#49398 = ORIENTED_EDGE ( 'NONE', *, *, #55295, .F. ) ;
#49399 = CARTESIAN_POINT ( 'NONE',  ( -99.92031302022661521, -296.9800116850897780, -225.4955720367904917 ) ) ;
#49400 = CARTESIAN_POINT ( 'NONE',  ( 15.25994442785172289, -290.2846324905020765, -323.3225548165859777 ) ) ;
#49401 = DIRECTION ( 'NONE',  ( 0.000000000000000000, -1.000000000000000000, 0.000000000000000000 ) ) ;
#49402 = ADVANCED_FACE ( 'NONE', ( #29934 ), #18037, .T. ) ;
#49403 = CARTESIAN_POINT ( 'NONE',  ( 44.71564893372296723, -278.0519495502701375, -270.3284710469131937 ) ) ;
#49404 = ORIENTED_EDGE ( 'NONE', *, *, #29058, .F. ) ;
#49405 = CARTESIAN_POINT ( 'NONE',  ( 26.94804623675772248, -273.0300826965657848, -231.3147130844005233 ) ) ;
#49406 = CARTESIAN_POINT ( 'NONE',  ( 14.91509961193351153, -292.7298278018279802, -325.8198169838761373 ) ) ;
#49407 = CARTESIAN_POINT ( 'NONE',  ( -107.2916408948669869, -272.1835785270253041, -248.9534160687415749 ) ) ;
#49408 = CARTESIAN_POINT ( 'NONE',  ( 33.75592638118311584, -289.3282176880996417, -289.9371406849874120 ) ) ;
#49409 = CARTESIAN_POINT ( 'NONE',  ( 0.9046582555454086849, -282.3296963963192070, -206.9362727628315497 ) ) ;
#49410 = CARTESIAN_POINT ( 'NONE',  ( -82.48977217368603476, -291.0807374593202326, -332.0073496755800306 ) ) ;
#49411 = CARTESIAN_POINT ( 'NONE',  ( -93.22107755772663040, -291.1493789675248536, -322.6944440754704146 ) ) ;
#49412 = CARTESIAN_POINT ( 'NONE',  ( -96.68368674968338894, -285.9235182862970532, -316.2463218228793949 ) ) ;
#49413 = CARTESIAN_POINT ( 'NONE',  ( -28.22710978558685113, -280.3313216066584914, -193.8488492315136682 ) ) ;
#49414 = CARTESIAN_POINT ( 'NONE',  ( -16.92002158697798109, -292.8704321592006750, -343.1632966093561663 ) ) ;
#49415 = CARTESIAN_POINT ( 'NONE',  ( 36.98556796121964396, -281.1330518979061708, -250.1999894972327070 ) ) ;
#49416 = CARTESIAN_POINT ( 'NONE',  ( 36.05947611051713153, -277.2675187611154684, -259.1792451408117586 ) ) ;
#49417 = CARTESIAN_POINT ( 'NONE',  ( 17.40634833298267736, -284.6948066931273047, -313.9805196606274080 ) ) ;
#49418 = CARTESIAN_POINT ( 'NONE',  ( 20.04010931073992552, -274.4743582386694243, -320.1934725044154675 ) ) ;
#49419 = DIRECTION ( 'NONE',  ( 0.000000000000000000, 1.000000000000000000, -0.000000000000000000 ) ) ;
#49420 = CARTESIAN_POINT ( 'NONE',  ( 15.30807541936421678, -280.3283352732976255, -219.6332399031979890 ) ) ;
#49421 = CARTESIAN_POINT ( 'NONE',  ( -39.93406478367798940, -278.2890813930548575, -346.9331684537138472 ) ) ;
#49422 = CARTESIAN_POINT ( 'NONE',  ( -35.39393116032591280, -275.3922497951883201, -196.8811905241217062 ) ) ;
#49423 = CARTESIAN_POINT ( 'NONE',  ( -29.47509650015330251, -285.2082409720796363, -194.0005472665238244 ) ) ;
#49424 = CARTESIAN_POINT ( 'NONE',  ( -111.3820781893685137, -292.3370658619879805, -268.4577588059781874 ) ) ;
#49425 = CARTESIAN_POINT ( 'NONE',  ( -97.19745026043671032, -274.7895696984243727, -223.2046805135603904 ) ) ;
#49426 = ADVANCED_FACE ( 'NONE', ( #53566 ), #17116, .T. ) ;
#49427 = CARTESIAN_POINT ( 'NONE',  ( -66.05776078182081790, -274.9993079865130881, -199.4338074242330947 ) ) ;
#49428 = FACE_OUTER_BOUND ( 'NONE', #50156, .T. ) ;
#49429 = EDGE_CURVE ( 'NONE', #19500, #41151, #31785, .T. ) ;
#49430 = CARTESIAN_POINT ( 'NONE',  ( -112.0438826179248366, -298.6093062999666472, -265.9325340999852187 ) ) ;
#49431 = CARTESIAN_POINT ( 'NONE',  ( -110.7835259300970279, -282.3671488988025544, -284.7251930423820454 ) ) ;
#49432 = CARTESIAN_POINT ( 'NONE',  ( -99.18507155737479764, -290.8286594947131789, -224.5008257068041644 ) ) ;
#49433 = CARTESIAN_POINT ( 'NONE',  ( 26.69966959923290872, -273.0552622143658255, -231.9131996019850703 ) ) ;
#49434 = CARTESIAN_POINT ( 'NONE',  ( -4.657533988044860962, -290.2289052117240544, -339.2099297022812152 ) ) ;
#49435 = CARTESIAN_POINT ( 'NONE',  ( -52.41997561662444127, -290.7749421919414772, -198.5672983850029993 ) ) ;
#49436 = ORIENTED_EDGE ( 'NONE', *, *, #40510, .F. ) ;
#49437 = CARTESIAN_POINT ( 'NONE',  ( -112.5565452629291912, -288.9562423503023183, -283.9011273403303335 ) ) ;
#49438 = CARTESIAN_POINT ( 'NONE',  ( -107.7711572187402140, -290.4735449506566738, -251.0795448945729049 ) ) ;
#49439 = VERTEX_POINT ( 'NONE', #58819 ) ;
#49440 = CARTESIAN_POINT ( 'NONE',  ( 0.1207374816257044542, -287.6184339904154399, -203.4278364882096639 ) ) ;
#49441 = CARTESIAN_POINT ( 'NONE',  ( -105.2859206908969298, -278.5277770804569855, -297.1131343331007315 ) ) ;
#49442 = CARTESIAN_POINT ( 'NONE',  ( -4.646843621756564069, -293.5518285725733563, -339.7479930571689124 ) ) ;
#49443 = CARTESIAN_POINT ( 'NONE',  ( -63.86905923309991806, -284.0405893864820541, -342.5387599876568174 ) ) ;
#49444 = CARTESIAN_POINT ( 'NONE',  ( -109.0103503931437814, -285.2432960619930782, -242.1207800228139035 ) ) ;
#49445 = CARTESIAN_POINT ( 'NONE',  ( 30.35571859035506037, -282.2518552521718789, -297.7316675854043524 ) ) ;
#49446 = CARTESIAN_POINT ( 'NONE',  ( -56.14975209998562633, -169.4529236618342622, -364.5118392738439752 ) ) ;
#49447 = CARTESIAN_POINT ( 'NONE',  ( 63.42894017176210752, 48.18213374631179136, -317.6803299212049865 ) ) ;
#49448 = CARTESIAN_POINT ( 'NONE',  ( -103.1447046786039579, -253.6660498445109226, -324.1576556378894907 ) ) ;
#49449 = CARTESIAN_POINT ( 'NONE',  ( -38.07374021736068670, -273.2399129551845363, -197.2033033293363644 ) ) ;
#49450 = CARTESIAN_POINT ( 'NONE',  ( -13.95386475250040093, -273.2831936092418914, -200.8828103631724105 ) ) ;
#49451 = CARTESIAN_POINT ( 'NONE',  ( -98.22960625220127895, -295.4315019411887420, -317.3950396915814736 ) ) ;
#49452 = CARTESIAN_POINT ( 'NONE',  ( -69.19725544157302011, -196.5455075490810657, -357.0703453118406969 ) ) ;
#49453 = CARTESIAN_POINT ( 'NONE',  ( -103.7928402092161235, -271.7338217202679971, -232.3398782779615601 ) ) ;
#49454 = CARTESIAN_POINT ( 'NONE',  ( -97.10864016964349332, -299.0196190437834503, -226.3080874927117918 ) ) ;
#49455 = CARTESIAN_POINT ( 'NONE',  ( -106.0049828406917101, -291.9747131526716544, -244.5347177229220392 ) ) ;
#49456 = ORIENTED_EDGE ( 'NONE', *, *, #51225, .T. ) ;
#49457 = CARTESIAN_POINT ( 'NONE',  ( -73.18147670076969291, -298.5304458648267314, -202.4177599501777536 ) ) ;
#49458 = CARTESIAN_POINT ( 'NONE',  ( 33.08691790676105171, -287.7878789450689965, -250.9240862264044836 ) ) ;
#49459 = CARTESIAN_POINT ( 'NONE',  ( -11.10271919309420063, -295.5216593545654860, -342.6371999761510665 ) ) ;
#49460 = CARTESIAN_POINT ( 'NONE',  ( -3.250406724806273129, -295.1064021985593513, -339.3489709049057410 ) ) ;
#49461 = CARTESIAN_POINT ( 'NONE',  ( 33.11725889488988628, -293.9716102246571268, -289.5014533879905230 ) ) ;
#49462 = ORIENTED_EDGE ( 'NONE', *, *, #2914, .F. ) ;
#49463 = CARTESIAN_POINT ( 'NONE',  ( 36.80095384282484616, -277.2866570656211707, -255.7946818047045952 ) ) ;
#49464 = EDGE_LOOP ( 'NONE', ( #62519, #29883, #93128 ) ) ;
#49465 = CARTESIAN_POINT ( 'NONE',  ( -71.20185806225903491, -279.1247490881081035, -201.2740959868586117 ) ) ;
#49466 = CARTESIAN_POINT ( 'NONE',  ( -16.58541738105294172, -275.2681287427270718, -200.0758771524112660 ) ) ;
#49467 = CARTESIAN_POINT ( 'NONE',  ( 6.630096824065898176, -276.4006525444441991, -208.3251524675641519 ) ) ;
#49468 = CARTESIAN_POINT ( 'NONE',  ( 24.69806964495408153, -274.1503487569419804, -313.2237394437113949 ) ) ;
#49469 = CARTESIAN_POINT ( 'NONE',  ( -68.09796366834507353, -298.2887424294363541, -204.0304306133187993 ) ) ;
#49470 = CARTESIAN_POINT ( 'NONE',  ( -103.3043138675389514, -294.6868285965343830, -303.1000690853238666 ) ) ;
#49471 = DIRECTION ( 'NONE',  ( 0.000000000000000000, 1.000000000000000000, 0.000000000000000000 ) ) ;
#49472 = CARTESIAN_POINT ( 'NONE',  ( -112.0276974366332894, -279.2764862227519416, -251.8265517239939300 ) ) ;
#49473 = CARTESIAN_POINT ( 'NONE',  ( 33.24273632964369796, -275.9647500860138507, -288.9846873093779891 ) ) ;
#49474 = CARTESIAN_POINT ( 'NONE',  ( 37.80894475152727807, -286.0564668012131051, -256.0196101091842706 ) ) ;
#49475 = CARTESIAN_POINT ( 'NONE',  ( 28.74821194883168118, -300.8778160839800648, -195.1719723918581053 ) ) ;
#49476 = CARTESIAN_POINT ( 'NONE',  ( -83.63170945779077670, -298.0521521680024080, -417.1172536214571096 ) ) ;
#49477 = CARTESIAN_POINT ( 'NONE',  ( 26.51329963375439291, -286.2607146584775819, -234.5483269106472903 ) ) ;
#49478 = CARTESIAN_POINT ( 'NONE',  ( -2.654609909276719915, -278.7572074108526863, -204.9649413578463566 ) ) ;
#49480 = CARTESIAN_POINT ( 'NONE',  ( -92.75298635848811557, -281.9342016311511543, -320.0884899109427693 ) ) ;
#49479 = CARTESIAN_POINT ( 'NONE',  ( -27.46143780333180828, -278.7547148109621844, -197.3865714288429274 ) ) ;
#49481 = CARTESIAN_POINT ( 'NONE',  ( 36.83476319661841814, -289.4056295124209441, -258.9370324115632798 ) ) ;
#49482 = CARTESIAN_POINT ( 'NONE',  ( -74.19947292626356727, -278.7589510638653678, -333.8326477372087879 ) ) ;
#49483 = FACE_OUTER_BOUND ( 'NONE', #69338, .T. ) ;
#49484 = CARTESIAN_POINT ( 'NONE',  ( -101.2569455388316726, -276.2445639505675672, -311.5523723529313429 ) ) ;
#49485 = CARTESIAN_POINT ( 'NONE',  ( 22.35929229859623746, -275.6152737403278934, -228.1531491960829214 ) ) ;
#49486 = CARTESIAN_POINT ( 'NONE',  ( 37.35778549759002942, -283.4392933612969045, -261.5392256303246654 ) ) ;
#49487 = DIRECTION ( 'NONE',  ( -0.000000000000000000, -1.000000000000000000, -0.000000000000000000 ) ) ;
#49488 = CARTESIAN_POINT ( 'NONE',  ( -10.06001275522469740, -290.6188696538366116, -340.8240425048663269 ) ) ;
#49489 = CARTESIAN_POINT ( 'NONE',  ( -28.96227084160118892, -290.1580768956535508, -195.7791394156632521 ) ) ;
#49490 = EDGE_CURVE ( 'NONE', #6854, #1135, #9053, .T. ) ;
#49491 = CARTESIAN_POINT ( 'NONE',  ( 82.15009695330279271, -299.4571376875543365, -197.3638982236675190 ) ) ;
#49492 = CARTESIAN_POINT ( 'NONE',  ( -62.18072331723876545, -272.4070535918263545, -201.1927263230633116 ) ) ;
#49493 = CARTESIAN_POINT ( 'NONE',  ( 36.94389710783553937, -291.6972964711824261, -270.7903160613001319 ) ) ;
#49494 = CARTESIAN_POINT ( 'NONE',  ( -105.6472514815422983, -266.3687386123619376, -319.2208520127341558 ) ) ;
#49495 = LINE ( 'NONE', #77925, #32295 ) ;
#49496 = CARTESIAN_POINT ( 'NONE',  ( -112.4542890685213763, -288.8614080061461777, -283.8814648792027242 ) ) ;
#49497 = CARTESIAN_POINT ( 'NONE',  ( -76.53490712612479285, -285.1857482956578451, -332.9542000552448826 ) ) ;
#49498 = CARTESIAN_POINT ( 'NONE',  ( -65.52470493161366960, -284.8532835358356579, -338.3534474379856078 ) ) ;
#49499 = CARTESIAN_POINT ( 'NONE',  ( -76.20425608541822271, -284.3885809887270852, -332.4073438537532184 ) ) ;
#49500 = CARTESIAN_POINT ( 'NONE',  ( -89.66245974754967563, -293.2991109728522474, -216.0581949996354751 ) ) ;
#49501 = CARTESIAN_POINT ( 'NONE',  ( 37.88615260635930326, -273.5349981528704575, -262.7501664701212007 ) ) ;
#49502 = CARTESIAN_POINT ( 'NONE',  ( 37.92382025403457391, -275.6826096186777590, -254.1480993044922911 ) ) ;
#49503 = CARTESIAN_POINT ( 'NONE',  ( -111.9423063141627352, -288.4790296920276091, -282.3637741688511369 ) ) ;
#49504 = CARTESIAN_POINT ( 'NONE',  ( -39.96295261462560688, -277.0842004637141258, -347.3295545798556532 ) ) ;
#49505 = CARTESIAN_POINT ( 'NONE',  ( -50.74228749793972071, -297.2040775523693128, -343.7932026459827739 ) ) ;
#49506 = CARTESIAN_POINT ( 'NONE',  ( -43.50149443762219903, -252.4652299798295019, -489.6847206897468823 ) ) ;
#49507 = CARTESIAN_POINT ( 'NONE',  ( 180.6899167944524436, 8.542400036368780647, 13.00000000000000178 ) ) ;
#49508 = CARTESIAN_POINT ( 'NONE',  ( -109.2057938497800933, -283.0345584545727888, -285.8091130482690119 ) ) ;
#49509 = CARTESIAN_POINT ( 'NONE',  ( -91.60857109470765636, -277.2794066226040854, -218.5171905846226821 ) ) ;
#49510 = DIRECTION ( 'NONE',  ( 0.000000000000000000, 0.000000000000000000, -1.000000000000000000 ) ) ;
#49511 = CARTESIAN_POINT ( 'NONE',  ( 11.35821897250883339, -273.1926209672289474, -211.5470117345105336 ) ) ;
#49512 = CARTESIAN_POINT ( 'NONE',  ( -13.76035386816042028, -276.0865810103486524, -339.6083501210218856 ) ) ;
#49513 = CARTESIAN_POINT ( 'NONE',  ( 1.955781103605104709, -296.0363515956383367, -332.7626873915692158 ) ) ;
#49514 = CARTESIAN_POINT ( 'NONE',  ( 39.40119774083780868, -280.4672661272284131, -269.9457209600016654 ) ) ;
#49515 = CARTESIAN_POINT ( 'NONE',  ( -26.15969492799074558, -295.8475481464012660, -342.7377109343363486 ) ) ;
#49516 = CARTESIAN_POINT ( 'NONE',  ( -108.9698912448646269, -297.5233737609799505, -297.3935862412163829 ) ) ;
#49517 = CARTESIAN_POINT ( 'NONE',  ( -35.81345161516997422, -297.9051277492375789, -197.3611626661092657 ) ) ;
#49518 = CARTESIAN_POINT ( 'NONE',  ( -78.36997468091350072, -293.5002010129019254, -207.5783071637992521 ) ) ;
#49519 = CARTESIAN_POINT ( 'NONE',  ( -46.50760314449774313, -286.1055498940846178, -193.9086083678337218 ) ) ;
#49520 = CARTESIAN_POINT ( 'NONE',  ( -32.73366931883641229, -272.2492001938284147, -194.7236352448972525 ) ) ;
#49521 = CARTESIAN_POINT ( 'NONE',  ( 2.742822895989173393, -286.4076286265218414, -204.6174413403601022 ) ) ;
#49522 = CARTESIAN_POINT ( 'NONE',  ( -100.8807796076376775, -281.0614440071479407, -231.0880770847348913 ) ) ;
#49523 = CARTESIAN_POINT ( 'NONE',  ( -91.68780161778320803, -284.3124121309485304, -221.1957865600609523 ) ) ;
#49524 = CARTESIAN_POINT ( 'NONE',  ( -34.76180697620001325, -287.0195713852256745, -345.3167368700294446 ) ) ;
#49525 = CARTESIAN_POINT ( 'NONE',  ( -69.18520112214993389, -196.4157418647702968, -356.4528236438462159 ) ) ;
#49526 = CARTESIAN_POINT ( 'NONE',  ( -2.151243864010800699, -286.0386496698555447, -206.2760749116829118 ) ) ;
#49527 = CARTESIAN_POINT ( 'NONE',  ( -113.8789064103646780, -289.5286037834381432, -276.9215164603783137 ) ) ;
#49528 = CARTESIAN_POINT ( 'NONE',  ( -106.8380299810364562, -279.7474731427586789, -301.7416430411084320 ) ) ;
#49529 = EDGE_CURVE ( 'NONE', #35152, #13924, #42222, .T. ) ;
#49530 = CARTESIAN_POINT ( 'NONE',  ( -109.2673725027800202, -279.5340802466330388, -296.5927324422127640 ) ) ;
#49531 = CARTESIAN_POINT ( 'NONE',  ( 21.81069152926886900, -281.9841633384567103, -313.1609556136323249 ) ) ;
#49532 = CARTESIAN_POINT ( 'NONE',  ( 36.59306450925804910, -277.3896077751226130, -257.6893042480007239 ) ) ;
#49533 = CARTESIAN_POINT ( 'NONE',  ( 11.19831191540491311, -294.4013019165051332, -330.2032949994159594 ) ) ;
#49534 = CARTESIAN_POINT ( 'NONE',  ( -64.44102773373909088, -287.4275611035830593, -339.9684785925542769 ) ) ;
#49535 = CARTESIAN_POINT ( 'NONE',  ( -98.69878289298003438, -296.0272434787479483, -230.1502765364316474 ) ) ;
#49536 = ORIENTED_EDGE ( 'NONE', *, *, #28070, .T. ) ;
#49537 = VERTEX_POINT ( 'NONE', #45981 ) ;
#49538 = CARTESIAN_POINT ( 'NONE',  ( -64.55956109852400004, -285.3304219374083459, -339.6467748141643597 ) ) ;
#49539 = CARTESIAN_POINT ( 'NONE',  ( -50.47917533872814744, -294.8912765312112469, -342.1907374426260162 ) ) ;
#49540 = CARTESIAN_POINT ( 'NONE',  ( 37.77063626484817149, -294.8261971509081718, -285.8410867322615445 ) ) ;
#49541 = CARTESIAN_POINT ( 'NONE',  ( -67.81931484460747583, -284.1145029419897696, -336.8066420584136154 ) ) ;
#49542 = CARTESIAN_POINT ( 'NONE',  ( -38.34228576782813036, -273.0986494635421877, -193.6029324753430103 ) ) ;
#49543 = CARTESIAN_POINT ( 'NONE',  ( 5.507411626225722223, -289.1397416561646878, -334.2145940682265746 ) ) ;
#49544 = CARTESIAN_POINT ( 'NONE',  ( -47.12077928171004260, -281.3147074676109582, -345.4921707492155178 ) ) ;
#49545 = CARTESIAN_POINT ( 'NONE',  ( -109.4555248953025028, -291.2278475023503006, -243.2770414514255037 ) ) ;
#49546 = CARTESIAN_POINT ( 'NONE',  ( 27.05111373861568680, -288.3559616659129574, -304.9020584416039696 ) ) ;
#49547 = CARTESIAN_POINT ( 'NONE',  ( 175.2296996224750103, 161.0000000000000853, 0.000000000000000000 ) ) ;
#49548 = DIRECTION ( 'NONE',  ( -0.000000000000000000, -1.000000000000000000, -0.000000000000000000 ) ) ;
#49549 = CARTESIAN_POINT ( 'NONE',  ( 153.3117529583858527, 204.6325910983726999, -214.2920792270980996 ) ) ;
#49550 = CARTESIAN_POINT ( 'NONE',  ( -106.6379572354042296, -282.4809262143061233, -236.9535640164627353 ) ) ;
#49551 = EDGE_LOOP ( 'NONE', ( #33450, #83967, #62867, #85210 ) ) ;
#49552 = CARTESIAN_POINT ( 'NONE',  ( -57.18372481543556773, -278.7103655612335729, -199.7883177753582800 ) ) ;
#49553 = CARTESIAN_POINT ( 'NONE',  ( 38.19881901303173777, -275.0335861821708363, -255.5498297369316276 ) ) ;
#49554 = CARTESIAN_POINT ( 'NONE',  ( -43.32900050412526127, -279.1281170140257473, -344.9545537593516542 ) ) ;
#49555 = CARTESIAN_POINT ( 'NONE',  ( -96.95435030675994881, -248.2403463976193621, -332.6261155525420463 ) ) ;
#49556 = CARTESIAN_POINT ( 'NONE',  ( 21.52843624158481362, -279.4670369831338235, -221.6485596558759994 ) ) ;
#49557 = CARTESIAN_POINT ( 'NONE',  ( -69.74548977179161113, -281.5010251890507789, -337.6198718618985595 ) ) ;
#49558 = CARTESIAN_POINT ( 'NONE',  ( -91.95294407782000690, -297.5787675882438634, -323.1965800079927931 ) ) ;
#49559 = CARTESIAN_POINT ( 'NONE',  ( 8.271472623199930041, -294.9011670952120312, -327.5000151657403080 ) ) ;
#49560 = ORIENTED_EDGE ( 'NONE', *, *, #39491, .T. ) ;
#49561 = CARTESIAN_POINT ( 'NONE',  ( -110.2809895493547998, -289.1189689047381535, -279.3668681743888556 ) ) ;
#49562 = CARTESIAN_POINT ( 'NONE',  ( -2.611013291941904235, -275.1506583338693304, -201.7381837791727435 ) ) ;
#49563 = CARTESIAN_POINT ( 'NONE',  ( -41.87046271344525650, -298.1601761463480216, -197.5017307084477238 ) ) ;
#49564 = ORIENTED_EDGE ( 'NONE', *, *, #43456, .T. ) ;
#49565 = CYLINDRICAL_SURFACE ( 'NONE', #11429, 4.999999999999986677 ) ;
#49566 = CARTESIAN_POINT ( 'NONE',  ( -113.5000000000000568, -296.0521521680024080, -537.7509286889328450 ) ) ;
#49567 = CARTESIAN_POINT ( 'NONE',  ( 202.9738562182569694, 293.9636489450776367, -44.00000000000000000 ) ) ;
#49568 = CARTESIAN_POINT ( 'NONE',  ( -64.94520369595728937, -280.7625471628977607, -202.4474031323467500 ) ) ;
#49569 = CARTESIAN_POINT ( 'NONE',  ( 3.261310291122220928, -282.3494526346327689, -206.0699364363243262 ) ) ;
#49570 = CARTESIAN_POINT ( 'NONE',  ( -73.92469122968472561, -282.6092327882400355, -333.8625342478071047 ) ) ;
#49571 = CARTESIAN_POINT ( 'NONE',  ( 19.77148438193743729, -282.7509526114511118, -222.9183055582599877 ) ) ;
#49572 = CARTESIAN_POINT ( 'NONE',  ( 31.90669141675908804, -274.3664828682270809, -295.7158029609094569 ) ) ;
#49573 = LINE ( 'NONE', #11718, #32169 ) ;
#49574 = CARTESIAN_POINT ( 'NONE',  ( 210.1640492649794396, 37.84931640281016030, 15.00000000000000000 ) ) ;
#49575 = CARTESIAN_POINT ( 'NONE',  ( -14.62765082341001310, -277.5680316141420576, -343.8213981323971780 ) ) ;
#49576 = ORIENTED_EDGE ( 'NONE', *, *, #21333, .F. ) ;
#49577 = VERTEX_POINT ( 'NONE', #44586 ) ;
#49578 = CARTESIAN_POINT ( 'NONE',  ( 175.2296996224750103, 20.99999999999998934, 0.000000000000000000 ) ) ;
#49579 = CARTESIAN_POINT ( 'NONE',  ( -35.90472487002985957, -285.0141347437764239, -345.7154563273417693 ) ) ;
#49580 = CARTESIAN_POINT ( 'NONE',  ( -1.167960896321708075, -291.7424252701682690, -206.7536673425425420 ) ) ;
#49581 = CARTESIAN_POINT ( 'NONE',  ( 0.6616879887054784026, -287.9082371396405620, -337.2722809867586875 ) ) ;
#49582 = CARTESIAN_POINT ( 'NONE',  ( -84.27335583830985399, -283.6365492073206269, -213.0634882587885102 ) ) ;
#49584 = CARTESIAN_POINT ( 'NONE',  ( -98.19466404581379493, -288.2128417990739422, -312.5128459672343411 ) ) ;
#49583 = CARTESIAN_POINT ( 'NONE',  ( -60.14411520869510497, -284.3254146904577624, -200.3938057380328814 ) ) ;
#49585 = CARTESIAN_POINT ( 'NONE',  ( -42.94801503898276707, -284.3294240698869544, -343.5941236076088217 ) ) ;
#49586 = CARTESIAN_POINT ( 'NONE',  ( 34.67285453171767529, -273.2801550712969743, -249.2293634457164728 ) ) ;
#49587 = CARTESIAN_POINT ( 'NONE',  ( -113.5554106382944468, -282.9211639783850387, -272.8030521181833592 ) ) ;
#49588 = CARTESIAN_POINT ( 'NONE',  ( -82.94830302127458310, -297.6758264042525752, -329.9668054032773057 ) ) ;
#49589 = CARTESIAN_POINT ( 'NONE',  ( -13.26622357517111617, -284.3639863414972524, -199.1543777550592722 ) ) ;
#49590 = CARTESIAN_POINT ( 'NONE',  ( -108.2032837142395749, -279.7373841354975639, -251.8173843365363211 ) ) ;
#49591 = CARTESIAN_POINT ( 'NONE',  ( 17.00785990269967840, -288.8241946479862463, -218.3615801760174122 ) ) ;
#49592 = CARTESIAN_POINT ( 'NONE',  ( 195.4781563537916043, 27.48493576247232895, 13.99999999999999822 ) ) ;
#49593 = CARTESIAN_POINT ( 'NONE',  ( 143.6449502718966755, -26.00396092263537540, 10.00000000000000178 ) ) ;
#49594 = CARTESIAN_POINT ( 'NONE',  ( 25.33126874728590039, -296.0389554458250245, -312.5679085555575512 ) ) ;
#49595 = CARTESIAN_POINT ( 'NONE',  ( -109.9012063239138683, -276.7964472443777026, -251.3339455880679338 ) ) ;
#49596 = CARTESIAN_POINT ( 'NONE',  ( -95.53192449113932128, -290.4285580735957524, -220.1607689647812833 ) ) ;
#49597 = CARTESIAN_POINT ( 'NONE',  ( 25.09330174392906798, -292.4908341288756901, -309.8056540410530033 ) ) ;
#49598 = CARTESIAN_POINT ( 'NONE',  ( -35.63466596294345123, -278.7588033778637282, -196.8753064768455658 ) ) ;
#49599 = CARTESIAN_POINT ( 'NONE',  ( -78.17190898149146960, -295.6367116617522584, -208.3012988245606891 ) ) ;
#49600 = CARTESIAN_POINT ( 'NONE',  ( -79.82936358749519457, -292.7796340671091571, -210.3317237195485916 ) ) ;
#49601 = CARTESIAN_POINT ( 'NONE',  ( -69.91165696735023971, -282.1233781216988064, -202.8022627189028810 ) ) ;
#49602 = CARTESIAN_POINT ( 'NONE',  ( -104.0066924283642322, -294.5451093671936746, -307.5971586733796812 ) ) ;
#49603 = CARTESIAN_POINT ( 'NONE',  ( -58.90361246526235561, -290.9357826069282282, -340.9944099585647450 ) ) ;
#49604 = CARTESIAN_POINT ( 'NONE',  ( 19.63394104791870731, -291.1019812454345583, -220.0647154533644994 ) ) ;
#49605 = CARTESIAN_POINT ( 'NONE',  ( -75.29896657940909677, -292.9610962875026985, -207.2570240953997143 ) ) ;
#49606 = CARTESIAN_POINT ( 'NONE',  ( 208.4306832106270804, -142.7221692137691775, 0.000000000000000000 ) ) ;
#49607 = CARTESIAN_POINT ( 'NONE',  ( -110.4671951191295989, -291.3080536491619910, -273.9269992693220388 ) ) ;
#49608 = LINE ( 'NONE', #64792, #14290 ) ;
#49609 = CIRCLE ( 'NONE', #63234, 25.00000000000000355 ) ;
#49610 = CARTESIAN_POINT ( 'NONE',  ( -99.71669408052348160, -292.3492262705923963, -225.8935022547664460 ) ) ;
#49612 = CARTESIAN_POINT ( 'NONE',  ( 34.06757603069395657, -293.7528807033340854, -285.5774379089120885 ) ) ;
#49611 = CARTESIAN_POINT ( 'NONE',  ( 34.89456460024948115, -279.8493962182371888, -291.9956943013424961 ) ) ;
#49613 = CARTESIAN_POINT ( 'NONE',  ( 33.17294455255802887, -281.1576968875261855, -239.4307949069247172 ) ) ;
#49614 = CARTESIAN_POINT ( 'NONE',  ( 39.50776930507541351, -281.2852057226770057, -275.6636721458789907 ) ) ;
#49615 = CARTESIAN_POINT ( 'NONE',  ( 8.159987322417903144, -284.6737996474529950, -210.6750414418727928 ) ) ;
#49616 = CARTESIAN_POINT ( 'NONE',  ( 35.14141974038829375, -279.8997213074912338, -286.3942966432434787 ) ) ;
#49617 = CARTESIAN_POINT ( 'NONE',  ( -59.88388321257586000, -283.7600525532362212, -198.7748273930347693 ) ) ;
#49618 = DIRECTION ( 'NONE',  ( 0.000000000000000000, -0.000000000000000000, 1.000000000000000000 ) ) ;
#49619 = CARTESIAN_POINT ( 'NONE',  ( -35.33468722438668408, -278.5567669666513666, -194.0678292584169640 ) ) ;
#49620 = CARTESIAN_POINT ( 'NONE',  ( -64.42511264268087245, -284.6271620021917101, -198.5975743485952023 ) ) ;
#49621 = CARTESIAN_POINT ( 'NONE',  ( -31.33662544711657461, -274.9327347012768428, -197.4338273301233073 ) ) ;
#49622 = FACE_OUTER_BOUND ( 'NONE', #76816, .T. ) ;
#49623 = CARTESIAN_POINT ( 'NONE',  ( 17.31711840160693328, -294.4487299873505322, -220.6993588358198508 ) ) ;
#49624 = CARTESIAN_POINT ( 'NONE',  ( 39.04135970047725124, -276.9514893513464813, -268.3033370053312865 ) ) ;
#49625 = CARTESIAN_POINT ( 'NONE',  ( -100.6032727243791811, -277.7177423027198984, -306.9326810004016011 ) ) ;
#49626 = CARTESIAN_POINT ( 'NONE',  ( -113.1329248472795399, -290.5479374808705302, -284.0256608303066059 ) ) ;
#49627 = CARTESIAN_POINT ( 'NONE',  ( -1.790921918066832985, -278.5992873217503529, -203.6868623150331246 ) ) ;
#49628 = CARTESIAN_POINT ( 'NONE',  ( -27.84698658338809096, -292.0027258700518473, -193.8950725848873162 ) ) ;
#49629 = EDGE_CURVE ( 'NONE', #31036, #14296, #64991, .T. ) ;
#49630 = CARTESIAN_POINT ( 'NONE',  ( -98.48941110709382940, -290.1691730303283521, -229.9656015824488406 ) ) ;
#49631 = CARTESIAN_POINT ( 'NONE',  ( -1.680188893756997093, -292.5794578047132291, -336.3548329139419479 ) ) ;
#49632 = ORIENTED_EDGE ( 'NONE', *, *, #79909, .F. ) ;
#49633 = CARTESIAN_POINT ( 'NONE',  ( 151.7498149058253887, 20.88232504567505288, 8.615841630451626543 ) ) ;
#49634 = CARTESIAN_POINT ( 'NONE',  ( 6.718338184219007303, -292.1777447237187175, -212.0798905985906515 ) ) ;
#49635 = CARTESIAN_POINT ( 'NONE',  ( 209.2890703971520452, 28.92173720827219086, 12.90116063919741407 ) ) ;
#49636 = CARTESIAN_POINT ( 'NONE',  ( -105.5937364680635966, -275.8380690714489560, -285.9065529553535612 ) ) ;
#49637 = CARTESIAN_POINT ( 'NONE',  ( -100.5500932208516929, -296.1880342579137846, -226.7774985727764658 ) ) ;
#49638 = CARTESIAN_POINT ( 'NONE',  ( -83.57180211223099775, -284.9862033013532709, -331.3872817576119019 ) ) ;
#49639 = CARTESIAN_POINT ( 'NONE',  ( 34.99643936965391333, -287.2512179996217014, -260.1839862995061594 ) ) ;
#49640 = CARTESIAN_POINT ( 'NONE',  ( 33.52141173430761967, -276.8052013668915379, -249.9520608366478598 ) ) ;
#49641 = CARTESIAN_POINT ( 'NONE',  ( -95.23384881368116339, -293.9198106378700572, -317.5017610726400221 ) ) ;
#49642 = CARTESIAN_POINT ( 'NONE',  ( -107.6766929757261266, -298.6158341756103027, -247.1558544014971233 ) ) ;
#49643 = CARTESIAN_POINT ( 'NONE',  ( -7.359414719053728682, -275.4448656147606016, -337.3550958277109544 ) ) ;
#49644 = EDGE_LOOP ( 'NONE', ( #30553, #25102, #21478, #10938 ) ) ;
#49645 = CARTESIAN_POINT ( 'NONE',  ( 195.0629117428269126, 293.9636489450776367, -54.00000000000000000 ) ) ;
#49646 = CARTESIAN_POINT ( 'NONE',  ( -114.2883800339493945, -296.2642707458900873, -266.7320425566662152 ) ) ;
#49647 = CARTESIAN_POINT ( 'NONE',  ( 32.31355466127269693, -289.1269743330070128, -243.9581742184847997 ) ) ;
#49648 = CARTESIAN_POINT ( 'NONE',  ( -71.68231431399064491, -295.5982969377303107, -203.6706444086711656 ) ) ;
#49649 = EDGE_CURVE ( 'NONE', #69300, #85724, #89055, .T. ) ;
#49650 = CARTESIAN_POINT ( 'NONE',  ( 24.32878666437833104, -288.7455111955325719, -309.6121527064545376 ) ) ;
#49651 = EDGE_LOOP ( 'NONE', ( #54403, #12775 ) ) ;
#49652 = CARTESIAN_POINT ( 'NONE',  ( -94.77775522932822128, -278.3030756798927996, -219.4305791311844871 ) ) ;
#49653 = CARTESIAN_POINT ( 'NONE',  ( 21.29530990945289659, -294.8750403548178838, -320.1106289427427782 ) ) ;
#49654 = CARTESIAN_POINT ( 'NONE',  ( -97.19856780072755953, -288.0613605313578773, -316.8095934867362757 ) ) ;
#49655 = CARTESIAN_POINT ( 'NONE',  ( -66.91239187261079735, -295.7624826590495672, -341.4479435667584539 ) ) ;
#49656 = CARTESIAN_POINT ( 'NONE',  ( 35.72916729967085558, -293.8906406244881282, -270.7558028428315424 ) ) ;
#49657 = DIRECTION ( 'NONE',  ( -0.000000000000000000, -0.000000000000000000, 1.000000000000000000 ) ) ;
#49658 = PRESENTATION_STYLE_ASSIGNMENT (( #78091 ) ) ;
#49659 = CARTESIAN_POINT ( 'NONE',  ( 139.4823848151520735, 130.0000000000000568, 12.50000000000000000 ) ) ;
#49660 = CARTESIAN_POINT ( 'NONE',  ( -48.74608349352957504, -290.7148443258338943, -345.8642122658699236 ) ) ;
#49661 = CARTESIAN_POINT ( 'NONE',  ( -115.3288506153726871, -280.8376638359844151, -288.1938231032136741 ) ) ;
#49662 = CARTESIAN_POINT ( 'NONE',  ( -84.49787322702056258, -278.7709811839317240, -209.5515938806253189 ) ) ;
#49663 = CARTESIAN_POINT ( 'NONE',  ( -104.6508006407196802, -286.1190163151418915, -303.1834571744745972 ) ) ;
#49664 = CARTESIAN_POINT ( 'NONE',  ( 22.54152070417518772, -285.4866857326896366, -222.8786281705411625 ) ) ;
#49665 = CARTESIAN_POINT ( 'NONE',  ( 35.93496382104577691, -285.8015801664035394, -283.4700737045235428 ) ) ;
#49666 = CARTESIAN_POINT ( 'NONE',  ( 18.97519612362179586, -278.1118691077887206, -321.0630098132747889 ) ) ;
#49668 = CARTESIAN_POINT ( 'NONE',  ( 29.06875212512782625, -280.4876672165820537, -239.6858164139459575 ) ) ;
#49667 = CARTESIAN_POINT ( 'NONE',  ( -93.94052838712022435, -279.2047528621832839, -224.2571849648247735 ) ) ;
#49669 = CARTESIAN_POINT ( 'NONE',  ( 1.028806970584595248, -275.6313910885928635, -203.9441133298500688 ) ) ;
#49670 = CARTESIAN_POINT ( 'NONE',  ( -101.5499708662807166, -277.8996932533872268, -228.4882948711697850 ) ) ;
#49671 = CARTESIAN_POINT ( 'NONE',  ( -40.74239786503150640, -139.1097897353693043, -361.8818269458895998 ) ) ;
#49672 = CARTESIAN_POINT ( 'NONE',  ( -29.87373460061922970, -275.0857525414263591, -193.9605309191074412 ) ) ;
#49673 = CARTESIAN_POINT ( 'NONE',  ( -106.2257198045210771, -274.4969280293119596, -237.5327829029802444 ) ) ;
#49674 = CARTESIAN_POINT ( 'NONE',  ( -114.2704648735229114, -287.0519495502703080, -270.3937649182068981 ) ) ;
#49675 = EDGE_LOOP ( 'NONE', ( #35595, #32058, #46453, #9948, #11003 ) ) ;
#49676 = VECTOR ( 'NONE', #31258, 1000.000000000000000 ) ;
#49677 = CARTESIAN_POINT ( 'NONE',  ( 82.62056641594917039, -301.7796436375890039, -194.2090517697148186 ) ) ;
#49678 = CARTESIAN_POINT ( 'NONE',  ( -2.049596653466665863, -287.6104143716297585, -206.0492558786767461 ) ) ;
#49679 = CARTESIAN_POINT ( 'NONE',  ( -52.00005431648487075, -287.6273099305882965, -195.7480235018652195 ) ) ;
#49680 = CARTESIAN_POINT ( 'NONE',  ( -18.45515703022170939, -288.1510543174051122, -341.0338234723051301 ) ) ;
#49681 = CARTESIAN_POINT ( 'NONE',  ( -88.28548820939360553, -283.2506877295736558, -328.0886325323236292 ) ) ;
#49682 = CARTESIAN_POINT ( 'NONE',  ( 25.83152688473413505, -279.4314095742582822, -232.1099269025458796 ) ) ;
#49683 = CARTESIAN_POINT ( 'NONE',  ( -41.41398145405877074, -287.8607831278534945, -196.2249841810826751 ) ) ;
#49684 = CARTESIAN_POINT ( 'NONE',  ( 33.40558350444596414, -279.7617100432004236, -249.7327488801840900 ) ) ;
#49685 = CARTESIAN_POINT ( 'NONE',  ( -6.051555397364877464, -277.9472573267697157, -336.8743821977475363 ) ) ;
#49686 = CARTESIAN_POINT ( 'NONE',  ( -11.47429486009469279, -274.8906215937448110, -201.9779292118369369 ) ) ;
#49687 = CARTESIAN_POINT ( 'NONE',  ( 36.00076146474930994, -286.6265590629299709, -292.5175486488519709 ) ) ;
#49688 = CARTESIAN_POINT ( 'NONE',  ( 23.28183560395387985, -282.9872311641152578, -317.5940955169109543 ) ) ;
#49689 = CARTESIAN_POINT ( 'NONE',  ( -104.3603271607003080, -284.5525202608938571, -308.2583003458410076 ) ) ;
#49690 = CARTESIAN_POINT ( 'NONE',  ( 35.35213792486316464, -281.6236964745351088, -263.1492342920464012 ) ) ;
#49691 = EDGE_LOOP ( 'NONE', ( #28744, #2059, #28949, #17902 ) ) ;
#49692 = ORIENTED_EDGE ( 'NONE', *, *, #42029, .T. ) ;
#49693 = CARTESIAN_POINT ( 'NONE',  ( 208.3936076804783966, 28.69480487596609919, 12.02381566707519944 ) ) ;
#49694 = CARTESIAN_POINT ( 'NONE',  ( -68.82211440461092877, -291.3219884770352337, -339.2903931898455880 ) ) ;
#49695 = CARTESIAN_POINT ( 'NONE',  ( -100.9160869950618746, -272.1086698645432875, -233.9038964900763915 ) ) ;
#49696 = CARTESIAN_POINT ( 'NONE',  ( 30.80817011324824861, -293.3609315278985719, -305.9828525328463797 ) ) ;
#49697 = CARTESIAN_POINT ( 'NONE',  ( -110.1067658829752673, -288.8786206709077646, -282.1005037632070298 ) ) ;
#49698 = CARTESIAN_POINT ( 'NONE',  ( 22.63890038393446602, -291.1934726271103386, -226.9771136712184330 ) ) ;
#49699 = CARTESIAN_POINT ( 'NONE',  ( 28.59114552718344981, -289.1916847768924868, -302.6099996284083886 ) ) ;
#49700 = CARTESIAN_POINT ( 'NONE',  ( -114.2704648735229114, -293.0519495502703080, -270.3937649182068981 ) ) ;
#49701 = CARTESIAN_POINT ( 'NONE',  ( -103.3825209483136689, -292.0804366682577893, -305.9084193053351441 ) ) ;
#49702 = CARTESIAN_POINT ( 'NONE',  ( -111.0747440640663655, -288.3639759312362116, -285.0369665777968748 ) ) ;
#49703 = CARTESIAN_POINT ( 'NONE',  ( -83.50245649666280201, -293.4198109312240490, -211.1843974535695168 ) ) ;
#49704 = CARTESIAN_POINT ( 'NONE',  ( -9.414723203474760993, -287.3675725798953522, -202.6460727989379507 ) ) ;
#49705 = CARTESIAN_POINT ( 'NONE',  ( 34.93415448850418414, -295.2866542660498226, -249.6689545277754121 ) ) ;
#49706 = CARTESIAN_POINT ( 'NONE',  ( -114.3276611901150659, -272.2616898454610350, -270.3574197013679168 ) ) ;
#49707 = DIRECTION ( 'NONE',  ( 0.000000000000000000, 1.000000000000000000, 0.000000000000000000 ) ) ;
#49708 = CARTESIAN_POINT ( 'NONE',  ( -111.9202768220849578, -274.6745027186147468, -259.2135409318198640 ) ) ;
#49709 = PRODUCT_DEFINITION_SHAPE ( 'NONE', 'NONE',  #12282 ) ;
#49710 = CARTESIAN_POINT ( 'NONE',  ( -3.959231174534847408, -280.6116839024791716, -337.5222035863770884 ) ) ;
#49711 = CARTESIAN_POINT ( 'NONE',  ( -113.4404092577192102, -295.8838235641732695, -259.6290520699915305 ) ) ;
#49712 = CARTESIAN_POINT ( 'NONE',  ( 20.66346370439013214, -273.1518255304276863, -224.3693719893715581 ) ) ;
#49713 = CARTESIAN_POINT ( 'NONE',  ( -51.57979615484179448, -275.3155206882368589, -343.4267789771403727 ) ) ;
#49714 = CARTESIAN_POINT ( 'NONE',  ( -101.6541489594178671, -298.3501832310023474, -234.7921370840643362 ) ) ;
#49715 = CARTESIAN_POINT ( 'NONE',  ( 17.67802907595304518, -273.3946276828778537, -217.2621713217016293 ) ) ;
#49716 = CARTESIAN_POINT ( 'NONE',  ( -109.7183769884873783, -297.8024216431435320, -283.7346490028505741 ) ) ;
#49717 = CARTESIAN_POINT ( 'NONE',  ( 196.0143093133015384, 24.42324672360809856, 11.99999999999998934 ) ) ;
#49718 = CARTESIAN_POINT ( 'NONE',  ( -101.6042868250468132, -296.8787084771199147, -305.3314150575736221 ) ) ;
#49719 = DIRECTION ( 'NONE',  ( 2.312964634635742267E-15, 0.000000000000000000, 1.000000000000000000 ) ) ;
#49721 = CARTESIAN_POINT ( 'NONE',  ( -65.57271514531647938, -297.6724027894083520, -203.0409145433498566 ) ) ;
#49720 = CARTESIAN_POINT ( 'NONE',  ( 37.70702564139116220, -285.6590223072589083, -277.1504891859455597 ) ) ;
#49722 = CARTESIAN_POINT ( 'NONE',  ( -68.50075781982525314, -285.6539466809196597, -199.9328714335240136 ) ) ;
#49723 = CARTESIAN_POINT ( 'NONE',  ( 37.12288259716916627, -287.4631987071650769, -289.8744521711566904 ) ) ;
#49724 = CARTESIAN_POINT ( 'NONE',  ( -111.2798307700559377, -298.7187674465575924, -255.7495586203262690 ) ) ;
#49725 = CARTESIAN_POINT ( 'NONE',  ( 24.43233675399941163, -292.1264055033022942, -312.6890782453603492 ) ) ;
#49726 = CARTESIAN_POINT ( 'NONE',  ( -98.44172566682247805, -278.3720035304528437, -223.7462797582116139 ) ) ;
#49727 = CARTESIAN_POINT ( 'NONE',  ( -95.99890600148557951, -287.4094976428776249, -317.0979686699210447 ) ) ;
#49728 = CARTESIAN_POINT ( 'NONE',  ( -23.40286736638519471, -135.2391364535880598, 22.50000000000000000 ) ) ;
#49729 = CARTESIAN_POINT ( 'NONE',  ( 16.27496074099764201, -285.6297388381625524, -220.2188778058160779 ) ) ;
#49730 = CARTESIAN_POINT ( 'NONE',  ( 197.3748232817348764, 214.9910457053126720, -12.45182892472558756 ) ) ;
#49731 = CARTESIAN_POINT ( 'NONE',  ( -81.60792948368583666, -287.6540168532412736, -330.9691453748866365 ) ) ;
#49732 = CARTESIAN_POINT ( 'NONE',  ( -72.05916672277926693, -299.1851909532456943, -205.2227431646824982 ) ) ;
#49733 = CARTESIAN_POINT ( 'NONE',  ( -11.72412971190821906, -281.8044268473148009, -198.3170543768111145 ) ) ;
#49735 = CARTESIAN_POINT ( 'NONE',  ( 3.390220919244847142, -282.4879635587228108, -331.0020504551936824 ) ) ;
#49734 = CARTESIAN_POINT ( 'NONE',  ( -111.0027954374962889, -294.3692174197221902, -286.2497883133154346 ) ) ;
#49736 = CARTESIAN_POINT ( 'NONE',  ( -113.6020565022060964, -296.8531797794875047, -259.6187472219308461 ) ) ;
#49737 = CARTESIAN_POINT ( 'NONE',  ( -110.9309288753746898, -273.9771951043131253, -270.3792229722685647 ) ) ;
#49738 = CARTESIAN_POINT ( 'NONE',  ( -4.555522512807772983, -282.4842437307777345, -202.8927937204268517 ) ) ;
#49739 = EDGE_CURVE ( 'NONE', #62133, #37419, #36222, .T. ) ;
#49741 = CARTESIAN_POINT ( 'NONE',  ( -97.06770705644282771, -296.2008161783655851, -227.9793702028909763 ) ) ;
#49740 = AXIS2_PLACEMENT_3D ( 'NONE', #24322, #67438, #1620 ) ;
#49742 = VERTEX_POINT ( 'NONE', #88128 ) ;
#49743 = DIRECTION ( 'NONE',  ( -1.000000000000000000, 0.000000000000000000, -0.000000000000000000 ) ) ;
#49744 = CARTESIAN_POINT ( 'NONE',  ( -18.29207605295991712, -284.7855113607416797, -342.5878238165592506 ) ) ;
#49745 = DIRECTION ( 'NONE',  ( 0.000000000000000000, 0.000000000000000000, 1.000000000000000000 ) ) ;
#49746 = CARTESIAN_POINT ( 'NONE',  ( 31.98288692825983404, -284.6237833571634042, -237.0123917617631264 ) ) ;
#49747 = CARTESIAN_POINT ( 'NONE',  ( 38.06226357854495035, -274.5641106988937850, -255.5827189383154803 ) ) ;
#49748 = CARTESIAN_POINT ( 'NONE',  ( -4.831172163236261419, -292.3259308427347491, -204.9861529717488509 ) ) ;
#49749 = CARTESIAN_POINT ( 'NONE',  ( 32.62886164679441237, -282.7662583247020507, -247.0740623273265442 ) ) ;
#49750 = CARTESIAN_POINT ( 'NONE',  ( 16.19206890419980382, -277.8765737109999918, -321.1604879431225754 ) ) ;
#49751 = CARTESIAN_POINT ( 'NONE',  ( -52.78067841596896415, -284.6713877280255360, -345.2499698865493087 ) ) ;
#49752 = CARTESIAN_POINT ( 'NONE',  ( 32.35849621574372037, -280.0415000291916954, -247.2005414872594997 ) ) ;
#49753 = CARTESIAN_POINT ( 'NONE',  ( -95.13123691389665737, -279.8924247039564079, -318.1867755589982494 ) ) ;
#49754 = CARTESIAN_POINT ( 'NONE',  ( 76.38675318495047861, -299.4392170424915776, -193.3610342431294384 ) ) ;
#49755 = CARTESIAN_POINT ( 'NONE',  ( 37.23821526959913086, -275.6251632670080767, -289.5140870422535500 ) ) ;
#49756 = CARTESIAN_POINT ( 'NONE',  ( 21.30251398466877077, -294.8382676646551204, -224.4910585793413418 ) ) ;
#49757 = CARTESIAN_POINT ( 'NONE',  ( 128.9467878515196162, -299.5541904835127980, -195.3611179825600175 ) ) ;
#49758 = ADVANCED_FACE ( 'NONE', ( #30866, #67775, #9527 ), #8147, .F. ) ;
#49759 = EDGE_CURVE ( 'NONE', #41101, #86528, #77050, .T. ) ;
#49760 = FACE_OUTER_BOUND ( 'NONE', #63339, .T. ) ;
#49761 = CARTESIAN_POINT ( 'NONE',  ( -113.0739147689394173, -294.7373817827403286, -266.7698167784902807 ) ) ;
#49762 = CARTESIAN_POINT ( 'NONE',  ( -43.48104944718411247, -273.4803023304604039, -197.5072270856211105 ) ) ;
#49763 = CARTESIAN_POINT ( 'NONE',  ( 38.96195801657260205, -295.0354543878029858, -267.4436248985124962 ) ) ;
#49764 = CARTESIAN_POINT ( 'NONE',  ( 37.96971742631737357, -294.9342013471664359, -284.4391780805657959 ) ) ;
#49765 = CARTESIAN_POINT ( 'NONE',  ( 35.80805840993487266, -289.7561556815304584, -286.2055236481873521 ) ) ;
#49766 = CARTESIAN_POINT ( 'NONE',  ( -108.1719323841925871, -276.8668976351476658, -246.0545505532937796 ) ) ;
#49767 = CARTESIAN_POINT ( 'NONE',  ( -29.53863327607716371, -278.8728663359054281, -344.4429308395170892 ) ) ;
#49768 = CARTESIAN_POINT ( 'NONE',  ( -38.38655828616665389, -293.1451975357958872, -344.7937887181799965 ) ) ;
#49769 = CARTESIAN_POINT ( 'NONE',  ( 38.05151388181356253, -283.5142879931343600, -278.3641237027651982 ) ) ;
#49770 = CARTESIAN_POINT ( 'NONE',  ( -89.87480949249908235, -284.2094730787247272, -219.1561191593192461 ) ) ;
#49771 = CARTESIAN_POINT ( 'NONE',  ( 204.9738562182569979, 293.9636489450776367, -54.00000000001201528 ) ) ;
#49772 = ORIENTED_EDGE ( 'NONE', *, *, #68258, .T. ) ;
#49773 = CARTESIAN_POINT ( 'NONE',  ( -87.70601829063315336, -284.9914670230021443, -217.4884129000527651 ) ) ;
#49774 = CARTESIAN_POINT ( 'NONE',  ( 24.01609537645098769, -283.2465998793716153, -316.3688721279685865 ) ) ;
#49775 = CARTESIAN_POINT ( 'NONE',  ( -107.8676054081266500, -282.9629749341521006, -300.3984759287489510 ) ) ;
#49776 = CARTESIAN_POINT ( 'NONE',  ( -96.64334107210639502, -280.1503675080806488, -221.5950525213766866 ) ) ;
#49777 = CARTESIAN_POINT ( 'NONE',  ( -77.43399729802185050, -279.0993625569138317, -335.3479731977087681 ) ) ;
#49778 = CARTESIAN_POINT ( 'NONE',  ( 7.450504543161046378, -296.9090924074130839, -326.4764044574609443 ) ) ;
#49779 = CARTESIAN_POINT ( 'NONE',  ( -55.29403410364363225, -169.9286504849079904, -364.5147574933134251 ) ) ;
#49780 = ORIENTED_EDGE ( 'NONE', *, *, #66104, .F. ) ;
#49781 = CARTESIAN_POINT ( 'NONE',  ( -106.0734115640449318, -274.9418047119115727, -240.6327310223400957 ) ) ;
#49782 = CARTESIAN_POINT ( 'NONE',  ( -46.63682837063362996, -277.9538278851993027, -196.2450598393899668 ) ) ;
#49783 = CARTESIAN_POINT ( 'NONE',  ( -74.20715666390071874, -293.3291786543345552, -203.9163128504025053 ) ) ;
#49784 = CARTESIAN_POINT ( 'NONE',  ( 19.43019322377892166, -292.2498925517618318, -224.2886864290337030 ) ) ;
#49785 = CARTESIAN_POINT ( 'NONE',  ( -68.03509219607683178, -288.9521356912331385, -340.9121107944810660 ) ) ;
#49786 = CARTESIAN_POINT ( 'NONE',  ( 200.4644824113734387, 249.5000000000000568, -2.942835885954282471 ) ) ;
#49788 = CARTESIAN_POINT ( 'NONE',  ( -73.93479024045835502, -283.9573723216579424, -206.2575723485693686 ) ) ;
#49787 = CARTESIAN_POINT ( 'NONE',  ( -41.92847484860295282, -293.6834815892525512, -346.6860920940337110 ) ) ;
#49789 = CARTESIAN_POINT ( 'NONE',  ( -90.72068405743362973, -293.1456056904294769, -218.7709100491314302 ) ) ;
#49790 = CARTESIAN_POINT ( 'NONE',  ( -23.95937649564948302, -284.1927967358367937, -342.6256105837574637 ) ) ;
#49791 = VERTEX_POINT ( 'NONE', #24204 ) ;
#49792 = CARTESIAN_POINT ( 'NONE',  ( -72.07655293769614957, -292.5454155814339856, -201.8899322832148471 ) ) ;
#49793 = CARTESIAN_POINT ( 'NONE',  ( -7.980464836452424215, -280.9398203629957607, -203.4452201630073773 ) ) ;
#49794 = CARTESIAN_POINT ( 'NONE',  ( 8.655424666131757760, -293.2322592690497913, -331.6169195703292871 ) ) ;
#49795 = CARTESIAN_POINT ( 'NONE',  ( -48.83472583511090903, -289.9976704382382877, -346.3890832113571605 ) ) ;
#49796 = CARTESIAN_POINT ( 'NONE',  ( -38.91262770159233497, -289.5637108024761233, -347.2835405265697659 ) ) ;
#49797 = CARTESIAN_POINT ( 'NONE',  ( 16.88919303119128301, -287.0189286124443129, -221.4751854650539826 ) ) ;
#49798 = ORIENTED_EDGE ( 'NONE', *, *, #82272, .F. ) ;
#49799 = CARTESIAN_POINT ( 'NONE',  ( 195.6201958373143270, 24.53660424933035955, 12.66340435719105351 ) ) ;
#49800 = CARTESIAN_POINT ( 'NONE',  ( 33.30836724089176926, -295.7648982284252952, -297.7266704035982912 ) ) ;
#49801 = CARTESIAN_POINT ( 'NONE',  ( -36.88358882543816009, -296.7426073036224352, -193.8543649343474158 ) ) ;
#49802 = CARTESIAN_POINT ( 'NONE',  ( -80.96912369364359563, -276.7200135657021178, -329.1833617382810644 ) ) ;
#49803 = CARTESIAN_POINT ( 'NONE',  ( -108.0184868496298662, -272.4489215396031341, -239.8237985079902614 ) ) ;
#49804 = CIRCLE ( 'NONE', #66445, 4.999999999999986677 ) ;
#49805 = CARTESIAN_POINT ( 'NONE',  ( -7.727282633707822868, -293.1367174796890254, -337.8558865948379548 ) ) ;
#49806 = CARTESIAN_POINT ( 'NONE',  ( 33.87899892761087273, -277.5754339134395536, -290.5467157374345675 ) ) ;
#49807 = CARTESIAN_POINT ( 'NONE',  ( -91.07459420315046827, -271.4183436200209485, -219.1210316221652477 ) ) ;
#49808 = CARTESIAN_POINT ( 'NONE',  ( 29.85973774946995363, -295.1521382093529269, -299.8754746736206016 ) ) ;
#49809 = CARTESIAN_POINT ( 'NONE',  ( -90.62248221880751942, -296.9088923129604041, -320.7868083438918347 ) ) ;
#49810 = CARTESIAN_POINT ( 'NONE',  ( -93.30409020842159862, -293.8543926363487344, -320.5623643558286631 ) ) ;
#49811 = CARTESIAN_POINT ( 'NONE',  ( 98.95318904190033038, -300.3680452193383417, -193.4483179873065808 ) ) ;
#49812 = CARTESIAN_POINT ( 'NONE',  ( 20.81201258752314587, -286.7571403089615956, -315.4760875844818315 ) ) ;
#49813 = CARTESIAN_POINT ( 'NONE',  ( 189.9243309297870610, 249.5000000000000568, 24.72542485937348644 ) ) ;
#49814 = CARTESIAN_POINT ( 'NONE',  ( -101.1610145235557070, -273.6121516511580580, -227.2939191672174957 ) ) ;
#49815 = CARTESIAN_POINT ( 'NONE',  ( -96.11986373800614558, -297.4927311286100462, -227.0131676883118530 ) ) ;
#49816 = CARTESIAN_POINT ( 'NONE',  ( 23.25376937781267728, -282.9236957762963129, -225.5660749455804819 ) ) ;
#49817 = CARTESIAN_POINT ( 'NONE',  ( 23.36628573990366320, -279.6116999667987102, -223.7796556094168068 ) ) ;
#49818 = ORIENTED_EDGE ( 'NONE', *, *, #8683, .F. ) ;
#49819 = CARTESIAN_POINT ( 'NONE',  ( 22.43877872555829711, -281.5504122552567878, -318.7513761988834631 ) ) ;
#49820 = CARTESIAN_POINT ( 'NONE',  ( 12.63207654232220101, -275.7249403157621828, -328.8071138383847369 ) ) ;
#49821 = CARTESIAN_POINT ( 'NONE',  ( 36.76552342114966621, -280.1768266888805670, -288.1525459193726419 ) ) ;
#49822 = CARTESIAN_POINT ( 'NONE',  ( -97.10289916224024864, -277.1748693176369329, -224.7481918372506868 ) ) ;
#49823 = EDGE_CURVE ( 'NONE', #27414, #1443, #34328, .T. ) ;
#49824 = CARTESIAN_POINT ( 'NONE',  ( 21.96674687273048932, -273.5214148574976321, -226.7964185958797714 ) ) ;
#49825 = CARTESIAN_POINT ( 'NONE',  ( -44.55529877465829713, -275.9611683749261033, -195.6574348565242758 ) ) ;
#49826 = CARTESIAN_POINT ( 'NONE',  ( 153.9143451375467748, 19.64542168185916537, 13.06799429260036050 ) ) ;
#49827 = CARTESIAN_POINT ( 'NONE',  ( -44.71056285174318390, -289.9795714653202481, -195.3152822124797012 ) ) ;
#49828 = CARTESIAN_POINT ( 'NONE',  ( -90.78593627599708782, -291.3195377114608391, -214.8550547389671692 ) ) ;
#49829 = CARTESIAN_POINT ( 'NONE',  ( 37.79212958427492453, -277.5980497971481213, -273.9308769174308509 ) ) ;
#49830 = CARTESIAN_POINT ( 'NONE',  ( 25.48235028399638580, -272.9995144579729072, -229.3960189570080104 ) ) ;
#49831 = CARTESIAN_POINT ( 'NONE',  ( 192.9623460957494956, 250.0000000000000568, 16.90571646082667812 ) ) ;
#49832 = FACE_BOUND ( 'NONE', #18428, .T. ) ;
#49833 = CARTESIAN_POINT ( 'NONE',  ( -111.9640761502929820, -282.4491171551121624, -278.3730152255371877 ) ) ;
#49834 = DIRECTION ( 'NONE',  ( 0.000000000000000000, 0.000000000000000000, 1.000000000000000000 ) ) ;
#49835 = CARTESIAN_POINT ( 'NONE',  ( 31.90961710675410501, -292.6706815374907933, -294.8316252812142011 ) ) ;
#49836 = CARTESIAN_POINT ( 'NONE',  ( 28.10849718413521003, -286.1626175983739699, -305.5009759754066749 ) ) ;
#49837 = CARTESIAN_POINT ( 'NONE',  ( 208.3332195429246383, 35.82735008953291356, 14.32883950752262514 ) ) ;
#49838 = DIRECTION ( 'NONE',  ( 0.000000000000000000, 0.000000000000000000, 1.000000000000000000 ) ) ;
#49839 = CARTESIAN_POINT ( 'NONE',  ( -76.72950313944535594, -293.5788096785367429, -334.2464492861664098 ) ) ;
#49840 = CARTESIAN_POINT ( 'NONE',  ( -37.33393347205793589, -281.5319053493707315, -346.6807339980219353 ) ) ;
#49841 = CARTESIAN_POINT ( 'NONE',  ( -46.57654910983590923, -281.5332717048788140, -197.0895256130339988 ) ) ;
#49842 = CARTESIAN_POINT ( 'NONE',  ( -64.42125486780727783, -286.9115405945510702, -198.6901562599271927 ) ) ;
#49843 = CARTESIAN_POINT ( 'NONE',  ( 27.00534518478758983, -279.2546664424246501, -229.8467278986334748 ) ) ;
#49844 = CARTESIAN_POINT ( 'NONE',  ( 35.68036566243934971, -287.5251269647072263, -268.3124598845219566 ) ) ;
#49845 = CARTESIAN_POINT ( 'NONE',  ( -36.44089622264606021, -278.4659548948858401, -343.9574030452341731 ) ) ;
#49846 = CARTESIAN_POINT ( 'NONE',  ( -108.3262700791548383, -279.1211240471191104, -288.1269243049661668 ) ) ;
#49847 = CARTESIAN_POINT ( 'NONE',  ( -102.6283106583776714, -287.0330868518112197, -232.6266498743745217 ) ) ;
#49848 = ORIENTED_EDGE ( 'NONE', *, *, #6789, .T. ) ;
#49849 = CARTESIAN_POINT ( 'NONE',  ( -57.38767208902535089, -297.6338203442297754, -195.9609744393078472 ) ) ;
#49850 = CARTESIAN_POINT ( 'NONE',  ( 21.67303688889696645, -290.1617528743838079, -316.0885798910165931 ) ) ;
#49851 = DIRECTION ( 'NONE',  ( -0.000000000000000000, -1.000000000000000000, -0.000000000000000000 ) ) ;
#49852 = CARTESIAN_POINT ( 'NONE',  ( 40.64545035920995986, -283.8376638359844719, -252.5284128619064461 ) ) ;
#49853 = EDGE_LOOP ( 'NONE', ( #7994, #31952, #51960, #5686, #77704, #86802, #853, #66700, #53512, #41617, #53975, #86951, #61626, #88215, #35671, #79612, #46147, #22169, #70084, #92499, #23692, #39272 ) ) ;
#49854 = CARTESIAN_POINT ( 'NONE',  ( 18.68676554844735094, -272.8551857226655102, -220.1763184737467043 ) ) ;
#49855 = CARTESIAN_POINT ( 'NONE',  ( 10.67820443440623279, -292.8014310114523369, -329.5943707563055227 ) ) ;
#49856 = CARTESIAN_POINT ( 'NONE',  ( -98.78845351809526676, -295.5121547124304584, -309.9795603880564840 ) ) ;
#49857 = CARTESIAN_POINT ( 'NONE',  ( 20.04300439882612395, -288.4244788781235229, -224.1058253997332770 ) ) ;
#49858 = CARTESIAN_POINT ( 'NONE',  ( 35.48653156009788745, -283.4848606421106183, -283.6240168736629244 ) ) ;
#49859 = CARTESIAN_POINT ( 'NONE',  ( -9.758969124533837913, -290.1240677433547148, -341.6197963537935607 ) ) ;
#49860 = CARTESIAN_POINT ( 'NONE',  ( -48.77862924457342331, -290.5099293751202367, -346.0618892339080048 ) ) ;
#49861 = CARTESIAN_POINT ( 'NONE',  ( -68.59519717577731512, -285.4630320083518882, -338.5389705067708519 ) ) ;
#49862 = CARTESIAN_POINT ( 'NONE',  ( -106.3444376767037198, -278.2783111592956402, -304.6515609684820447 ) ) ;
#49863 = CARTESIAN_POINT ( 'NONE',  ( 34.11644967576441445, -291.9492431073694547, -295.0783180677186692 ) ) ;
#49864 = CARTESIAN_POINT ( 'NONE',  ( -7.535029617025729820, -280.2655665605205968, -199.3498964331015486 ) ) ;
#49865 = CARTESIAN_POINT ( 'NONE',  ( -54.51997738608783806, -275.6895067215083373, -198.1408142731350779 ) ) ;
#49866 = CARTESIAN_POINT ( 'NONE',  ( 35.78497577281001440, -290.2662352645559167, -287.0191576251351080 ) ) ;
#49867 = VECTOR ( 'NONE', #2816, 1000.000000000000000 ) ;
#49868 = CARTESIAN_POINT ( 'NONE',  ( 30.35777514462878912, -273.3416883002064424, -235.8537990613072566 ) ) ;
#49869 = DIRECTION ( 'NONE',  ( 0.000000000000000000, 0.000000000000000000, 1.000000000000000000 ) ) ;
#49870 = CARTESIAN_POINT ( 'NONE',  ( 18.88747793414631815, -280.3985701247459019, -223.6912113599244947 ) ) ;
#49871 = CARTESIAN_POINT ( 'NONE',  ( 37.24475432140723541, -276.5370697889363214, -252.8435944168766980 ) ) ;
#49872 = VECTOR ( 'NONE', #49487, 1000.000000000000000 ) ;
#49873 = CARTESIAN_POINT ( 'NONE',  ( -96.58539395881665257, -298.5845457343937142, -226.6871207229745551 ) ) ;
#49874 = CARTESIAN_POINT ( 'NONE',  ( -90.28456718528400415, -282.8376740532990539, -326.0206415007153851 ) ) ;
#49875 = CARTESIAN_POINT ( 'NONE',  ( -106.0454413714065254, -291.9472761082202510, -298.0261843923643141 ) ) ;
#49876 = CARTESIAN_POINT ( 'NONE',  ( -10.64716429470371928, -275.9945981632093890, -198.9338323928342334 ) ) ;
#49877 = CARTESIAN_POINT ( 'NONE',  ( -107.6311005046765956, -274.2561518344775209, -240.0161713817290945 ) ) ;
#49878 = FACE_BOUND ( 'NONE', #52581, .T. ) ;
#49879 = CARTESIAN_POINT ( 'NONE',  ( 11.50704648305693567, -296.3728436974096212, -327.0517554645664973 ) ) ;
#49880 = CARTESIAN_POINT ( 'NONE',  ( -103.4013038288097874, -282.0833372669978303, -305.6305016335276719 ) ) ;
#49881 = CARTESIAN_POINT ( 'NONE',  ( -94.69271820775296078, -290.9155900141443567, -219.0132356817496486 ) ) ;
#49882 = CARTESIAN_POINT ( 'NONE',  ( 36.98965680128517164, -273.6604138287934802, -277.1945781595177891 ) ) ;
#49883 = CARTESIAN_POINT ( 'NONE',  ( 25.68409957670541388, -288.5813889267474224, -227.5103852169342247 ) ) ;
#49884 = EDGE_CURVE ( 'NONE', #38497, #55253, #43778, .T. ) ;
#49885 = CARTESIAN_POINT ( 'NONE',  ( -97.00495677743501233, -290.0661575415214202, -227.6780694355106505 ) ) ;
#49886 = EDGE_LOOP ( 'NONE', ( #59960, #15309, #74479, #41476 ) ) ;
#49887 = CARTESIAN_POINT ( 'NONE',  ( -107.8166305711135493, -289.5053653399637028, -240.8333264887179155 ) ) ;
#49888 = CARTESIAN_POINT ( 'NONE',  ( -109.6444847925146320, -290.0829406724311639, -280.6682380794902087 ) ) ;
#49889 = EDGE_LOOP ( 'NONE', ( #5768, #8548, #72077, #26852, #17496, #82008, #1428, #18813 ) ) ;
#49890 = CARTESIAN_POINT ( 'NONE',  ( 31.41640632547085232, -289.0714297820604202, -304.4487862585778544 ) ) ;
#49891 = CARTESIAN_POINT ( 'NONE',  ( 16.54962570921479781, -276.5922205805587737, -319.6526059576839316 ) ) ;
#49892 = EDGE_CURVE ( 'NONE', #15778, #36174, #83044, .T. ) ;
#49893 = CARTESIAN_POINT ( 'NONE',  ( -61.50725645781604101, -294.2790779780762591, -343.2006902315841899 ) ) ;
#49894 = CARTESIAN_POINT ( 'NONE',  ( -97.95894348735140511, -284.5704908871134080, -317.6777386843335194 ) ) ;
#49895 = CARTESIAN_POINT ( 'NONE',  ( -99.32974058128755246, -285.4929659885997353, -224.6310229122993576 ) ) ;
#49896 = CARTESIAN_POINT ( 'NONE',  ( 25.57940460067867861, -282.3954333990724308, -307.5153564327474101 ) ) ;
#49897 = CARTESIAN_POINT ( 'NONE',  ( 167.9348045515096999, 232.6400991984046982, -192.7129745902395541 ) ) ;
#49898 = CARTESIAN_POINT ( 'NONE',  ( 166.7220858323138657, 232.6500979171330243, -192.0954861747825362 ) ) ;
#49899 = CARTESIAN_POINT ( 'NONE',  ( 201.2091912597866781, 293.0223957429525399, -68.25549348882485390 ) ) ;
#49900 = CARTESIAN_POINT ( 'NONE',  ( -109.2866109036451547, -271.9277654570573191, -256.8038092756640935 ) ) ;
#49901 = CARTESIAN_POINT ( 'NONE',  ( -40.77571630126477942, -272.9284093343463837, -197.0825670178670634 ) ) ;
#49902 = CARTESIAN_POINT ( 'NONE',  ( -0.7409784574130733326, -294.0870274742118795, -338.0510532825337577 ) ) ;
#49903 = CARTESIAN_POINT ( 'NONE',  ( 194.1843140057649180, 275.6304509567530090, -124.2126573568886130 ) ) ;
#49904 = CARTESIAN_POINT ( 'NONE',  ( -46.80330380301038673, -272.6192283555371887, -194.4415794704493123 ) ) ;
#49905 = CARTESIAN_POINT ( 'NONE',  ( -94.58089565245009567, -299.0716829612376841, -223.0704147883828909 ) ) ;
#49906 = CARTESIAN_POINT ( 'NONE',  ( 6.149853404731024931, -289.7634432556220645, -329.6675105043229905 ) ) ;
#49907 = CARTESIAN_POINT ( 'NONE',  ( -93.68620571708281375, -292.2945742797382991, -223.4424461779046851 ) ) ;
#49908 = EDGE_LOOP ( 'NONE', ( #20779, #51629, #34908, #83150 ) ) ;
#49909 = CARTESIAN_POINT ( 'NONE',  ( -108.1533424280992790, -297.1136974343089037, -300.1386756128952129 ) ) ;
#49910 = CARTESIAN_POINT ( 'NONE',  ( -5.777737175144225468, -286.9710166889316838, -204.4557096529882756 ) ) ;
#49911 = CARTESIAN_POINT ( 'NONE',  ( -0.7739967851248829023, -295.3819980031690875, -337.9552737183033742 ) ) ;
#49912 = CARTESIAN_POINT ( 'NONE',  ( -98.22191719684298050, -296.4160370038868564, -317.4049919001111562 ) ) ;
#49913 = CARTESIAN_POINT ( 'NONE',  ( 35.62126243195009323, -293.6881613454568765, -268.0360160606145996 ) ) ;
#49914 = ORIENTED_EDGE ( 'NONE', *, *, #29336, .T. ) ;
#49915 = CARTESIAN_POINT ( 'NONE',  ( -94.94605581947607220, -275.1441773710411667, -221.4427998460582216 ) ) ;
#49916 = EDGE_LOOP ( 'NONE', ( #31567, #59491, #21241, #42805, #64829 ) ) ;
#49917 = CARTESIAN_POINT ( 'NONE',  ( -96.76589954008809968, -278.7170006614438194, -221.4704843348012560 ) ) ;
#49918 = CARTESIAN_POINT ( 'NONE',  ( 12.09740312572577459, -273.1529084986812563, -215.4998132229447378 ) ) ;
#49919 = CARTESIAN_POINT ( 'NONE',  ( 31.48700090851100342, -276.8274603059280707, -295.5289102498280727 ) ) ;
#49920 = CARTESIAN_POINT ( 'NONE',  ( 37.49020875899221750, -277.1441014553167861, -257.0899434384185724 ) ) ;
#49921 = CARTESIAN_POINT ( 'NONE',  ( 37.10662818347357472, -273.4222446961183550, -258.6221591936090931 ) ) ;
#49922 = CARTESIAN_POINT ( 'NONE',  ( -93.69746017186588460, -297.8628762267681509, -223.7807039619924581 ) ) ;
#49923 = CARTESIAN_POINT ( 'NONE',  ( -108.7422698158706709, -295.3606841369601170, -252.4957229784031085 ) ) ;
#49924 = LINE ( 'NONE', #22000, #57798 ) ;
#49925 = CARTESIAN_POINT ( 'NONE',  ( -110.4931335231892859, -279.3465685677120405, -246.3509518847648394 ) ) ;
#49926 = CARTESIAN_POINT ( 'NONE',  ( 18.30978838515730089, -276.3905736382098439, -317.6042320923178295 ) ) ;
#49927 = CARTESIAN_POINT ( 'NONE',  ( -29.49674674230796256, -284.8343792380504169, -194.2575373921601454 ) ) ;
#49928 = CARTESIAN_POINT ( 'NONE',  ( -110.4982369779130238, -274.7645059412130308, -253.8347218290428771 ) ) ;
#49929 = CARTESIAN_POINT ( 'NONE',  ( 82.67722570198282028, -297.3296337185574316, -196.5151116418807931 ) ) ;
#49930 = CARTESIAN_POINT ( 'NONE',  ( 24.36907679217138423, -287.2914998494832162, -309.6597405889123706 ) ) ;
#49931 = CARTESIAN_POINT ( 'NONE',  ( -38.34538218574085278, -278.2792632068584453, -196.3420145611505632 ) ) ;
#49932 = CARTESIAN_POINT ( 'NONE',  ( -14.10575345053863572, -278.9341216763961029, -200.4827074408945577 ) ) ;
#49934 = CARTESIAN_POINT ( 'NONE',  ( -93.97195694407641042, -285.8698452214187000, -319.5537570489542532 ) ) ;
#49933 = AXIS2_PLACEMENT_3D ( 'NONE', #3522, #59911, #9690 ) ;
#49935 = CARTESIAN_POINT ( 'NONE',  ( -59.29924859845507257, -278.5479144188467444, -340.3967986692132399 ) ) ;
#49936 = B_SPLINE_CURVE_WITH_KNOTS ( 'NONE', 3,
 ( #56300, #20776, #393, #79484, #92727, #49187, #72373, #13682, #93203, #7490, #70974, #27899, #6107, #36375, #71444, #65288, #85630, #29282, #6581, #49648, #50107, #28355, #86087, #79002, #5482, #68936, #26779, #77920, #11158, #55200, #13062, #84986, #19664, #56621, #85472, #12577, #34354, #70356, #40472, #49023, #76502, #4067, #63259, #41898, #83579, #12095, #11626, #92090, #48532, #76030, #54702, #32937, #77433, #34816, #47117, #26305, #18741, #55665, #84055, #19202, #40019, #27725, #41424, #47600, #76966, #61829, #90662, #25822, #27247, #62791, #91626, #69389, #56133, #4522, #69862, #33398, #62297, #33882, #92554, #91138, #48062, #5000, #40942, #84517, #20141, #70812, #5944, #63729, #93039, #35758, #78838, #50888, #7787, #58472, #28652, #13520, #232, #85923, #72668, #21074, #51336, #13984, #93499, #37143, #57543, #65595, #14462, #708, #80230, #71760, #29593, #86386, #66050, #49945, #79769, #36673, #21537, #7331, #29112, #57084, #1163, #42845, #50420, #30046, #79324, #87316, #43319, #22464, #15366, #6885, #44227, #72215, #36211, #73137, #8262, #58927, #65130, #58008, #64671, #78379, #86863, #22018, #14912, #20619, #49489, #42368, #43767, #71280, #6407, #64209, #35282, #28196, #23408, #9169, #17234, #10575, #44700, #32375, #31443, #8712, #9649, #45613, #1619, #30502, #51797, #38533, #81610, #24801, #67437, #46096, #15842, #2564, #53686, #80689, #2095, #82554, #31901, #60332, #3482, #87777, #53198, #45151, #23861, #3015, #89169, #24321, #73601, #75001, #17702, #59397, #52727, #52275, #38979, #82076, #22927, #88251, #37589, #10113, #75455, #66500, #66956, #46555, #39438, #81154, #16298, #38047, #68354, #67892, #74050, #16759, #30985, #59873, #88713, #60793, #89631, #74514, #68831, #55561, #90110, #83952, #3960, #25262, #33769, #54139, #41308, #4885, #19102, #32834, #83008, #61724, #62191, #76399, #11986, #39911, #11522, #25714, #91515, #5835, #47957, #76861, #61275, #69286, #26671, #40835, #40369, #84409, #41793, #27135, #91021, #47491, #69754, #62681, #55084, #56019, #19557, #47013, #18160, #75916, #48423, #90556, #54598, #11041, #77328, #12461, #83469, #70245, #34245, #26190, #18625, #4415, #5379, #33293, #91982, #63151, #20026, #84875, #48903, #77805, #12955, #70704, #43661, #64090, #35650, #56507, #6300, #78730, #120, #92446, #35168, #595, #21906, #22353, #92930, #28091, #13873, #51227, #86275, #56977, #58365, #87205, #73017, #27609, #29477, #72111, #57434, #71641, #42725, #63621, #93391, #79665, #64566, #85815, #6774, #7227, #20966, #20514, #49382, #28543, #85365, #36101, #78275, #13413, #65020, #42257, #49833, #21428, #29003, #50301, #79207, #80115, #15254, #57888, #14350, #44115, #43209, #86744, #50779, #14806, #72556, #7678, #71171, #65477, #36563, #34707, #38868, #88599, #9995, #87663, #30389, #81493, #73488, #59281, #1503, #9052, #53565, #66387, #60678, #16184, #74885, #51682, #89054, #37029, #15724, #29933, #74396, #89518, #46437, #81040, #44585, #16640, #45035, #73937, #1054, #67774, #45494, #30865, #37930, #66839, #65943, #1973, #53080, #23748, #52611, #8600, #2450, #58818, #59759, #37477, #22812, #9525, #82440, #88126, #80570, #38411, #23285, #52158, #67320, #31328, #60215, #24203, #2901, #81958, #17114, #45980, #31784, #24681, #17588, #8146, #54958, #46898, #33650, #75799, #12340, #10923, #19445, #41188, #62070, #77212, #61158, #3843, #83835, #32725, #68713, #76280, #27021, #39790, #34132, #83353, #48311, #25149, #62558, #18989, #19912, #33181, #90904, #75340, #70126, #10456, #61612, #5263, #91400, #55910, #63036, #11406, #90444, #47841, #76743, #69174, #91867, #26555, #89994, #68240, #54023, #26071, #82890, #18046, #39322, #11871, #4303, #84762, #40723, #3363, #40258, #32251, #25601, #69639, #54484, #18503, #55443, #47365, #4767, #84295, #59596, #44427, #23113, #2291, #37777, #30696, #43953, #74240, #24047, #52462, #51068, #87500, #52922, #9360, #22649, #16948, #45339, #36872, #87050, #38244, #51521, #8444, #16483, #9841, #72850, #31629, #88446, #7978, #8899, #44882, #896, #29779, #79955, #66683, #80883, #81801, #1810, #67158, #15093, #23595, #45812, #65787, #1345, #74721, #31174, #81336, #2749, #22199, #60060, #73333, #51996, #88898, #38714, #67621, #58658, #80408, #15555, #37323, #16031, #66231, #30228, #59119, #87960, #73784, #82279, #33021, #48146, #5088, #39624, #84137, #19287, #60520, #39167, #10766, #41022, #90747, #3204, #90295, #69945, #53394, #89356, #47685, #76116, #11249, #68079, #54787, #24512, #83199, #32088, #17431, #61911, #46280, #40561, #4150, #18347, #60989, #75184, #89837, #61464, #75643, #40103, #24998, #68548, #53870, #25905, #76586, #4607, #3687, #10297, #47202, #69019, #82736, #17888, #46740, #32572, #25447, #77048, #54324, #11709, #83666, #69475, #26395, #18830, #33480, #62383, #91228, #12178 ),
 .UNSPECIFIED., .F., .F.,
 ( 4, 1, 1, 1, 2, 2, 2, 2, 2, 2, 2, 2, 2, 2, 2, 2, 2, 2, 2, 2, 2, 2, 2, 2, 2, 2, 2, 2, 2, 2, 2, 2, 2, 2, 2, 2, 2, 2, 2, 2, 2, 2, 2, 2, 2, 2, 2, 2, 2, 2, 2, 2, 2, 2, 2, 2, 2, 2, 2, 2, 2, 2, 2, 2, 2, 2, 2, 2, 2, 2, 2, 2, 2, 2, 2, 2, 2, 2, 2, 2, 2, 2, 2, 2, 2, 2, 2, 2, 2, 2, 2, 2, 2, 2, 2, 2, 2, 2, 2, 2, 2, 2, 2, 2, 2, 2, 2, 2, 2, 2, 2, 2, 2, 2, 2, 2, 2, 2, 2, 2, 2, 2, 2, 2, 2, 2, 2, 2, 2, 2, 2, 2, 2, 2, 2, 2, 2, 2, 2, 2, 2, 2, 2, 2, 2, 2, 2, 2, 2, 2, 2, 2, 2, 2, 2, 2, 2, 2, 2, 2, 2, 2, 2, 2, 2, 2, 2, 2, 2, 2, 2, 2, 2, 2, 2, 2, 2, 2, 2, 2, 2, 2, 2, 2, 2, 2, 2, 2, 2, 2, 2, 2, 2, 2, 2, 2, 2, 2, 2, 2, 2, 2, 2, 2, 2, 2, 2, 2, 2, 2, 2, 2, 2, 2, 2, 2, 2, 2, 2, 2, 2, 2, 2, 2, 2, 2, 2, 2, 2, 2, 2, 2, 2, 2, 2, 2, 2, 2, 2, 2, 2, 2, 2, 2, 2, 2, 2, 2, 2, 2, 2, 2, 2, 2, 2, 2, 2, 2, 2, 2, 2, 2, 2, 2, 2, 2, 2, 2, 2, 2, 2, 2, 2, 2, 2, 2, 2, 2, 2, 2, 2, 2, 2, 2, 2, 2, 2, 2, 2, 2, 2, 2, 2, 2, 2, 2, 2, 2, 2, 2, 4 ),
 ( -0.05114148247438684430, -0.02298081116268822083, -0.008900475506838909090, -0.001860307678914256690, -0.0001002657219330849170, 0.0007797552565574905614, 0.001659776235048066040, 0.005179860149010367953, 0.008699944062972676806, 0.01222002797693497872, 0.01398006993391614355, 0.01574011189089730839, 0.01926019580485965194, 0.02278027971882199548, 0.02630036363278432515, 0.02806040558976548999, 0.02982044754674665482, 0.03334053146070899837, 0.03686061537467134192, 0.04038069928863367158, 0.04214074124561486417, 0.04390078320259605676, 0.04742086711655842807, 0.05094095103052078549, 0.05446103494448314292, 0.05622107690146430775, 0.05798111885844545871, 0.06150120277240774674, 0.06502128668637005560, 0.06854137060033232975, 0.07030141255731350847, 0.07206145451429465942, 0.07558153842825710012, 0.07910162234221954081, 0.08262170625618195374, 0.08438174821316321572, 0.08614179017014442219, 0.08966187408410689064, 0.09318195799806935908, 0.09670204191203182753, 0.09846208386901306175, 0.1002221258259942960, 0.1037422097399567644, 0.1072622936539192606, 0.1107823775678817291, 0.1143024614818441975, 0.1178225453958066660, 0.1213426293097691622, 0.1248627132237316306, 0.1283827971376941268, 0.1301428390946753610, 0.1319028810516565953, 0.1354229649656189804, 0.1389430488795813934, 0.1424631327935438063, 0.1442231747505249573, 0.1459832167075061360, 0.1495033006214684657, 0.1530233845354307953, 0.1565434684493930972, 0.1583035104063742760, 0.1600635523633553992, 0.1635836362773177288, 0.1671037201912800307, 0.1706238041052423327, 0.1723838460622234836, 0.1741438880192046346, 0.1776639719331669642, 0.1811840558471292661, 0.1847041397610916236, 0.1864641817180728023, 0.1882242236750539255, 0.1917443075890162829, 0.1952643915029785848, 0.1987844754169409145, 0.2005445173739221210, 0.2023045593309032719, 0.2058246432448655738, 0.2093447271588279313, 0.2128648110727902332, 0.2146248530297713841, 0.2163848949867525906, 0.2199049789007148925, 0.2234250628146771944, 0.2269451467286395518, 0.2287051886856207028, 0.2304652306426018538, 0.2339853145565642112, 0.2375053984705265131, 0.2410254823844888705, 0.2427855243414700215, 0.2445455662984512279, 0.2480656502124134744, 0.2515857341263758040, 0.2551058180403380504, 0.2568658599973192014, 0.2586259019543003523, 0.2621459858682626543, 0.2656660697822250117, 0.2691861536961873691, 0.2709461956531685756, 0.2727062376101497820, 0.2762263215241121950, 0.2797464054380744969, 0.2832664893520369098, 0.2850265313090181718, 0.2867865732659993228, 0.2903066571799617912, 0.2938267410939241486, 0.2973468250078865061, 0.2991068669648677680, 0.3008669089218489745, 0.3043869928358113319, 0.3079070767497736894, 0.3114271606637361023, 0.3131872026207173088, 0.3149472445776985152, 0.3184673284916609282, 0.3219874124056232856, 0.3255074963195856430, 0.3272675382765669050, 0.3290275802335480559, 0.3325476641475105244, 0.3360677480614729373, 0.3395878319754353503, 0.3413478739324165567, 0.3431079158893978187, 0.3466279998033601761, 0.3501480837173225336, 0.3536681676312848910, 0.3571882515452473039, 0.3607083354592097169, 0.3642284193731720188, 0.3677485032871344317, 0.3712685872010967891, 0.3730286291580779956, 0.3747886711150591466, 0.3783087550290215040, 0.3818288389429838059, 0.3853489228569461633, 0.3871089648139272588, 0.3888690067709084652, 0.3923890906848707671, 0.3959091745988330691, 0.3994292585127954265, 0.4011893004697765774, 0.4029493424267577839, 0.4064694263407201413, 0.4099895102546823877, 0.4135095941686447452, 0.4152696361256259516, 0.4170296780826071026, 0.4205497619965694045, 0.4240698459105317619, 0.4275899298244940083, 0.4293499717814752703, 0.4311100137384563658, 0.4346300976524188342, 0.4381501815663812471, 0.4416702654803436046, 0.4434303074373248665, 0.4451903493943059620, 0.4487104333082684304, 0.4522305172222308989, 0.4557506011361933118, 0.4575106430931744073, 0.4592706850501556137, 0.4627907689641180267, 0.4663108528780804396, 0.4698309367920429636, 0.4715909787490241700, 0.4733510207060054875, 0.4768711046199679005, 0.4803911885339304244, 0.4839112724478930594, 0.4856713144048742659, 0.4874313563618555833, 0.4909514402758181073, 0.4944715241897805202, 0.4979916081037431552, 0.4997516500607243617, 0.5015116920177056237, 0.5050317759316681476, 0.5085518598456305606, 0.5120719437595931955, 0.5138319857165745130, 0.5155920276735557195, 0.5191121115875182435, 0.5226321955014807674, 0.5261522794154432914, 0.5279123213724246089, 0.5296723633294058153, 0.5331924472433682283, 0.5367125311573306412, 0.5402326150712931652, 0.5419926570282743716, 0.5437526989852555781, 0.5472727828992179910, 0.5507928668131805150, 0.5543129507271429279, 0.5560729926841241344, 0.5578330346411054519, 0.5613531185550678648, 0.5648732024690302778, 0.5683932863829926907, 0.5701533283399738972, 0.5719133702969553257, 0.5754334542109176276, 0.5789535381248800405, 0.5824736220388425645, 0.5842336639958237710, 0.5859937059528050884, 0.5895137898667675014, 0.5930338737807299143, 0.5965539576946923273, 0.6000740416086547402, 0.6035941255226172641, 0.6071142094365796771, 0.6106342933505419790, 0.6141543772645045030, 0.6176744611784669159, 0.6211945450924293288, 0.6247146290063917418, 0.6282347129203541547, 0.6299947548773354722, 0.6317547968343166787, 0.6352748807482792026, 0.6387949646622416155, 0.6423150485762039175, 0.6440750905331852350, 0.6458351324901665524, 0.6493552164041290764, 0.6528753003180916004, 0.6563953842320541243, 0.6581554261890353308, 0.6599154681460166483, 0.6634355520599792833, 0.6669556359739419182, 0.6704757198879045532, 0.6722357618448857597, 0.6739958038018670772, 0.6775158877158296011, 0.6810359716297923471, 0.6845560555437549821, 0.6863160975007362996, 0.6880761394577177281, 0.6915962233716802521, 0.6951163072856428871, 0.6986363911996055220, 0.7003964331565868395, 0.7021564751135682680, 0.7056765590275310140, 0.7091966429414936490, 0.7127167268554563950, 0.7144767688124378235, 0.7162368107694191410, 0.7197568946833818870, 0.7232769785973446330, 0.7267970625113073790, 0.7303171464252701250, 0.7338372303392328710, 0.7373573142531956170, 0.7408773981671583631, 0.7426374401241396805, 0.7443974820811209980, 0.7479175659950836330, 0.7514376499090462680, 0.7549577338230089030, 0.7567177757799902205, 0.7584778177369715380, 0.7619979016509341729, 0.7655179855648969189, 0.7690380694788595539, 0.7707981114358408714, 0.7725581533928222999, 0.7760782373067848239, 0.7795983212207474589, 0.7831184051347100938, 0.7848784470916913003, 0.7866384890486726178, 0.7901585729626353638, 0.7936786568765978878, 0.7971987407905605227, 0.7989587827475419513, 0.8007188247045232687, 0.8042389086184859037, 0.8077589925324485387, 0.8112790764464110627, 0.8130391184033924912, 0.8147991603603738087, 0.8183192442743365547, 0.8218393281882991896, 0.8253594121022617136, 0.8271194540592430311, 0.8288794960162242376, 0.8323995799301868725, 0.8359196638441495075, 0.8394397477581122535, 0.8429598316720747775, 0.8464799155860374125, 0.8499999995000000474 ),
 .UNSPECIFIED. ) ;
#49937 = CARTESIAN_POINT ( 'NONE',  ( 0.000000000000000000, 0.000000000000000000, -10.00000000000000000 ) ) ;
#49938 = CARTESIAN_POINT ( 'NONE',  ( -98.84297425056954012, -276.1918105779139978, -315.0102310916517467 ) ) ;
#49939 = AXIS2_PLACEMENT_3D ( 'NONE', #48900, #5832, #85362 ) ;
#49940 = CARTESIAN_POINT ( 'NONE',  ( -40.78803848670462173, -274.6592142832270724, -197.2906976340829885 ) ) ;
#49941 = CARTESIAN_POINT ( 'NONE',  ( 32.60874082869640489, -283.1933631683393742, -242.7061953222809620 ) ) ;
#49942 = EDGE_CURVE ( 'NONE', #16833, #85072, #5025, .T. ) ;
#49943 = LINE ( 'NONE', #78836, #49872 ) ;
#49944 = CARTESIAN_POINT ( 'NONE',  ( -26.32980674612250382, -290.8331944710387233, -345.1143948346768866 ) ) ;
#49945 = CARTESIAN_POINT ( 'NONE',  ( 37.58299951730145949, -291.4960744939204460, -266.0064704915159268 ) ) ;
#49946 = CARTESIAN_POINT ( 'NONE',  ( 82.17440492340898572, -297.5479941798179766, -195.4018648718562758 ) ) ;
#49947 = CARTESIAN_POINT ( 'NONE',  ( 23.46973980794102133, -273.6666490244173815, -229.0685454680651958 ) ) ;
#49948 = CARTESIAN_POINT ( 'NONE',  ( 28.59433252085374377, -291.2356437154830360, -236.2538595750842205 ) ) ;
#49949 = CARTESIAN_POINT ( 'NONE',  ( 10.80643407470098794, -61.58976173765800155, -353.1561788127373802 ) ) ;
#49950 = CARTESIAN_POINT ( 'NONE',  ( 184.7149167944524493, 8.542400036368780647, 10.00000000000000000 ) ) ;
#49951 = CARTESIAN_POINT ( 'NONE',  ( -59.84147477128698256, -287.8183871765951949, -343.2752311041638222 ) ) ;
#49952 = CARTESIAN_POINT ( 'NONE',  ( -64.32915313783280453, -285.0104479084794207, -339.0496744937643712 ) ) ;
#49953 = CARTESIAN_POINT ( 'NONE',  ( -2.665074207940166140, -284.7440948665608857, -202.7336474404863225 ) ) ;
#49954 = CARTESIAN_POINT ( 'NONE',  ( -40.23953651559801870, -284.5145646323277333, -343.8932705592785055 ) ) ;
#49955 = CARTESIAN_POINT ( 'NONE',  ( -105.3602928414461957, -284.9936877729901994, -297.4447114687678209 ) ) ;
#49956 = CARTESIAN_POINT ( 'NONE',  ( -44.76074966074679651, -293.9387174026987850, -195.3202298937241039 ) ) ;
#49957 = CARTESIAN_POINT ( 'NONE',  ( 31.69400916265432144, -274.0315022388318766, -301.0756916892908635 ) ) ;
#49958 = CARTESIAN_POINT ( 'NONE',  ( 18.07142704441768544, -275.1528975929713283, -216.8511909310712440 ) ) ;
#49959 = CARTESIAN_POINT ( 'NONE',  ( -111.7496423533197145, -288.7995213023934298, -257.2168289779902466 ) ) ;
#49960 = CARTESIAN_POINT ( 'NONE',  ( -96.14919039427111613, -277.8822763525339496, -320.0873948776813904 ) ) ;
#49961 = CARTESIAN_POINT ( 'NONE',  ( 37.17494982320157249, -295.4651766209661901, -265.1775562567756310 ) ) ;
#49962 = PLANE ( 'NONE',  #89251 ) ;
#49963 = CARTESIAN_POINT ( 'NONE',  ( 10.59707575819634329, -295.1948066931273615, -210.1954327657594490 ) ) ;
#49964 = CARTESIAN_POINT ( 'NONE',  ( -93.62202789313710127, -283.9036784939293057, -223.0983611230452084 ) ) ;
#49965 = CARTESIAN_POINT ( 'NONE',  ( -36.74227282106746628, -278.0595291278528975, -195.3508019111592091 ) ) ;
#49966 = CARTESIAN_POINT ( 'NONE',  ( -68.54269788882368175, -272.1294591379420922, -200.7106174634450042 ) ) ;
#49967 = CARTESIAN_POINT ( 'NONE',  ( -59.23341496180492527, -276.6917244709753163, -340.1081285966567975 ) ) ;
#49968 = CARTESIAN_POINT ( 'NONE',  ( 7.078905814450073386, -294.1898900028027128, -211.5604588173541174 ) ) ;
#49969 = CARTESIAN_POINT ( 'NONE',  ( 32.57499248578534434, -294.7813057824154725, -292.1570933492282052 ) ) ;
#49970 = CARTESIAN_POINT ( 'NONE',  ( -70.57839402521152294, -296.7963447966814101, -339.2857686870148655 ) ) ;
#49971 = CARTESIAN_POINT ( 'NONE',  ( -110.0501054498872691, -296.4786513967191013, -263.2975445926482507 ) ) ;
#49972 = CARTESIAN_POINT ( 'NONE',  ( -26.15201131581959970, -290.9099957412431081, -344.5741468933361489 ) ) ;
#49973 = CARTESIAN_POINT ( 'NONE',  ( -110.6848982627649178, -284.4235528446827743, -293.8518830798702197 ) ) ;
#49974 = CARTESIAN_POINT ( 'NONE',  ( -94.14446629654599974, -271.3817415821985719, -220.2237941849799654 ) ) ;
#49975 = CARTESIAN_POINT ( 'NONE',  ( 23.86272689839336891, -286.7623067945394268, -223.6167196894971312 ) ) ;
#49976 = CARTESIAN_POINT ( 'NONE',  ( -107.8087820482681565, -280.2099084882878515, -295.1396067773449090 ) ) ;
#49977 = CARTESIAN_POINT ( 'NONE',  ( -98.29628346355481483, -284.1726373679227891, -229.7662018160411606 ) ) ;
#49978 = CARTESIAN_POINT ( 'NONE',  ( -107.9904147739487712, -288.2239917004074528, -295.6898193521115559 ) ) ;
#49979 = CARTESIAN_POINT ( 'NONE',  ( -51.00049622308160480, -154.6998088915060237, -359.8797964913271130 ) ) ;
#49980 = CARTESIAN_POINT ( 'NONE',  ( 16.02369730450794094, -286.3423523712069141, -220.4415237970370356 ) ) ;
#49981 = CARTESIAN_POINT ( 'NONE',  ( 23.22468854747723910, -283.1256281732290745, -317.5473166582940507 ) ) ;
#49982 = CARTESIAN_POINT ( 'NONE',  ( -114.1331516043878480, -289.6361445254684668, -268.3488820958181122 ) ) ;
#49983 = CARTESIAN_POINT ( 'NONE',  ( -73.40519736204895196, -281.1821234153238152, -203.2205836637277514 ) ) ;
#49984 = CARTESIAN_POINT ( 'NONE',  ( -110.8679762718638955, -280.1341592762694859, -249.2143690663019981 ) ) ;
#49985 = CARTESIAN_POINT ( 'NONE',  ( -1.964219354252200178, -280.3680026367551932, -206.5063307022557240 ) ) ;
#49986 = CARTESIAN_POINT ( 'NONE',  ( 21.12850565075724774, -276.8912531468064344, -223.9393622968399598 ) ) ;
#49987 = CARTESIAN_POINT ( 'NONE',  ( 6.614001572301820175, -294.4729801561877025, -333.6470975303669775 ) ) ;
#49988 = CARTESIAN_POINT ( 'NONE',  ( -61.81761491615411330, -287.3919497729942805, -340.8790334142558436 ) ) ;
#49989 = CARTESIAN_POINT ( 'NONE',  ( -68.02551635220173409, -293.2561245674103247, -200.5977489755723582 ) ) ;
#49990 = CARTESIAN_POINT ( 'NONE',  ( -88.72829054802704718, -294.7142789891280472, -322.7167368490790409 ) ) ;
#49991 = ORIENTED_EDGE ( 'NONE', *, *, #52504, .F. ) ;
#49992 = CARTESIAN_POINT ( 'NONE',  ( -5.393159943599763473, -284.5487333360299544, -337.6105856441724313 ) ) ;
#49993 = CARTESIAN_POINT ( 'NONE',  ( -106.7255447496959846, -296.5227493353484647, -247.4419006604565823 ) ) ;
#49994 = CARTESIAN_POINT ( 'NONE',  ( -22.26805625430534974, -293.3203818394849804, -195.1120797738107910 ) ) ;
#49995 = CARTESIAN_POINT ( 'NONE',  ( 35.78914642240709298, -282.1800118415428074, -268.5728174589726791 ) ) ;
#49996 = CARTESIAN_POINT ( 'NONE',  ( -60.78781625148388912, -272.8140667961619670, -197.2091506282590956 ) ) ;
#49997 = CARTESIAN_POINT ( 'NONE',  ( -41.74641657612756518, -289.7576548684417617, -347.1461356101472120 ) ) ;
#49998 = CARTESIAN_POINT ( 'NONE',  ( -97.08527888746390033, -282.0590682803995151, -316.9552193414020280 ) ) ;
#49999 = AXIS2_PLACEMENT_3D ( 'NONE', #69790, #12989, #63657 ) ;
#50000 = CARTESIAN_POINT ( 'NONE',  ( -88.63855353245243407, -291.6885423064632619, -212.9644532514443540 ) ) ;
#50001 = CARTESIAN_POINT ( 'NONE',  ( 16.02931784716777486, -288.6026706362052323, -320.2710579388211727 ) ) ;
#50002 = DIRECTION ( 'NONE',  ( 0.000000000000000000, 0.000000000000000000, 1.000000000000000000 ) ) ;
#50003 = DIRECTION ( 'NONE',  ( 0.000000000000000000, 0.000000000000000000, 1.000000000000000000 ) ) ;
#50004 = CARTESIAN_POINT ( 'NONE',  ( 196.6421184343808193, 281.7221770927952207, -110.2479207600687516 ) ) ;
#50005 = CIRCLE ( 'NONE', #68131, 0.5000000000000004441 ) ;
#50006 = CARTESIAN_POINT ( 'NONE',  ( -85.28047601435909542, -270.9094976428775681, -210.1954327657594206 ) ) ;
#50007 = CARTESIAN_POINT ( 'NONE',  ( -87.63422226383934799, -278.5255360678094689, -217.1567198283532889 ) ) ;
#50008 = ORIENTED_EDGE ( 'NONE', *, *, #8199, .T. ) ;
#50009 = CARTESIAN_POINT ( 'NONE',  ( -74.65131410698072045, -278.4637608769353960, -207.1979521230794887 ) ) ;
#50010 = CARTESIAN_POINT ( 'NONE',  ( 22.74451162792970393, -274.5739322906576945, -222.2216988036958014 ) ) ;
#50011 = CARTESIAN_POINT ( 'NONE',  ( -110.3740690499103749, -272.8271011984412553, -283.8530902933177913 ) ) ;
#50012 = CARTESIAN_POINT ( 'NONE',  ( -94.50880747682556660, -277.8191335602747927, -219.6607419386456570 ) ) ;
#50013 = CARTESIAN_POINT ( 'NONE',  ( -5.350386419023300810, -280.6493188996844879, -337.8170228336247760 ) ) ;
#50014 = CARTESIAN_POINT ( 'NONE',  ( -112.3922847719415188, -298.4640266242891471, -258.3880479038497242 ) ) ;
#50015 = CARTESIAN_POINT ( 'NONE',  ( 22.98734806831856048, -294.6185109508961659, -311.6611798477420621 ) ) ;
#50016 = ORIENTED_EDGE ( 'NONE', *, *, #91848, .F. ) ;
#50017 = CARTESIAN_POINT ( 'NONE',  ( -98.53048209343150177, -288.6754195420510314, -311.0924680925500638 ) ) ;
#50018 = CARTESIAN_POINT ( 'NONE',  ( -1.356548821269418781, -275.1681274408801414, -202.4024417720908673 ) ) ;
#50019 = CARTESIAN_POINT ( 'NONE',  ( -76.56422738799662397, -273.5111542454246205, -208.7933231922218056 ) ) ;
#50020 = VERTEX_POINT ( 'NONE', #69416 ) ;
#50021 = FACE_OUTER_BOUND ( 'NONE', #27323, .T. ) ;
#50022 = CARTESIAN_POINT ( 'NONE',  ( 184.7149167944524493, -12.49482340714361506, 10.00000000000000000 ) ) ;
#50023 = CARTESIAN_POINT ( 'NONE',  ( 154.4364498827612806, 20.25578850495988092, 11.06489058133685788 ) ) ;
#50024 = CARTESIAN_POINT ( 'NONE',  ( 19.90883224788790073, -281.9876375116658096, -224.5724445204919277 ) ) ;
#50025 = CARTESIAN_POINT ( 'NONE',  ( -53.56626286476127774, -281.6070426620511284, -196.0729217802764310 ) ) ;
#50026 = CARTESIAN_POINT ( 'NONE',  ( -107.9913014393528812, -283.3563270936316485, -289.6968913261640068 ) ) ;
#50027 = CARTESIAN_POINT ( 'NONE',  ( -43.88315029685729485, -281.8291573199855975, -196.3636013321710436 ) ) ;
#50028 = CARTESIAN_POINT ( 'NONE',  ( 32.72703048520246227, -273.7300393484001120, -247.3696343110754867 ) ) ;
#50029 = CARTESIAN_POINT ( 'NONE',  ( 175.2296996224750103, 20.00000000000000000, 0.000000000000000000 ) ) ;
#50030 = CARTESIAN_POINT ( 'NONE',  ( 207.2842799582832356, 30.47689859374760957, 12.00000000000000000 ) ) ;
#50031 = CARTESIAN_POINT ( 'NONE',  ( -51.27328725340623805, -278.0287571111343823, -345.9261211268482725 ) ) ;
#50032 = CARTESIAN_POINT ( 'NONE',  ( 197.8563597697584839, 24.47698789593438917, 12.00000000000000178 ) ) ;
#50033 = ORIENTED_EDGE ( 'NONE', *, *, #45323, .T. ) ;
#50034 = CARTESIAN_POINT ( 'NONE',  ( -23.68628624284178130, -55.96374926131388605, 21.50000000000000000 ) ) ;
#50035 = CARTESIAN_POINT ( 'NONE',  ( -33.12502947872636838, -284.9792081295841513, -345.6111072953592043 ) ) ;
#50036 = CARTESIAN_POINT ( 'NONE',  ( 30.98283435409080511, -292.4007101989516286, -244.2008482125474131 ) ) ;
#50037 = CARTESIAN_POINT ( 'NONE',  ( 38.98833348891655248, -287.0229320956844390, -280.1184906954568987 ) ) ;
#50038 = CARTESIAN_POINT ( 'NONE',  ( -100.4619602754840741, -283.3184626201401670, -231.6137203340301483 ) ) ;
#50040 = CARTESIAN_POINT ( 'NONE',  ( 8.591538043416290904, -286.6526909978351796, -328.3965523477402257 ) ) ;
#50039 = CARTESIAN_POINT ( 'NONE',  ( -90.07250555346972476, -283.8639279031973501, -218.9573483226625683 ) ) ;
#50041 = CARTESIAN_POINT ( 'NONE',  ( 22.91950354912111010, -283.3380699810228407, -312.2624047959108111 ) ) ;
#50042 = CARTESIAN_POINT ( 'NONE',  ( -38.30548008206496036, -272.0399123560097223, -195.3673063639620864 ) ) ;
#50043 = CARTESIAN_POINT ( 'NONE',  ( -69.43711815090962602, -284.0367239618503277, -201.2359448963899808 ) ) ;
#50044 = CARTESIAN_POINT ( 'NONE',  ( -94.05208249591784408, -297.8715440663210074, -319.4420020705679804 ) ) ;
#50045 = CARTESIAN_POINT ( 'NONE',  ( -18.61358390961857268, -284.2925103463169876, -197.5111273657321078 ) ) ;
#50046 = CARTESIAN_POINT ( 'NONE',  ( -110.5147438345516093, -279.4537126266886276, -273.3800784291963737 ) ) ;
#50047 = CARTESIAN_POINT ( 'NONE',  ( 12.99968803966445208, -288.7529821462077280, -214.4721992003050275 ) ) ;
#50048 = CARTESIAN_POINT ( 'NONE',  ( 197.5992351617976226, 290.6681976320160743, -7.304042938976587074 ) ) ;
#50049 = EDGE_CURVE ( 'NONE', #13111, #55526, #80086, .T. ) ;
#50050 = EDGE_CURVE ( 'NONE', #75749, #4469, #21086, .T. ) ;
#50051 = FACE_BOUND ( 'NONE', #85089, .T. ) ;
#50052 = CARTESIAN_POINT ( 'NONE',  ( 36.90562894240503766, -295.2935817163242405, -256.3379825907792906 ) ) ;
#50053 = CARTESIAN_POINT ( 'NONE',  ( -111.0943360317898936, -276.7268931420227887, -256.7394679982444927 ) ) ;
#50054 = CARTESIAN_POINT ( 'NONE',  ( -112.7644876348830110, -289.9341866814194191, -255.6105936382482184 ) ) ;
#50055 = CARTESIAN_POINT ( 'NONE',  ( -56.02530817874509950, -293.6965266030794623, -341.8099003453828004 ) ) ;
#50056 = CARTESIAN_POINT ( 'NONE',  ( -69.94408142513989901, -278.2982957920120839, -204.4811941811498173 ) ) ;
#50057 = CARTESIAN_POINT ( 'NONE',  ( -72.22481840170092937, -295.7252059208834680, -204.8178063481725815 ) ) ;
#50058 = CARTESIAN_POINT ( 'NONE',  ( -98.72057099681400416, -292.4252351299080033, -229.8473941049495863 ) ) ;
#50059 = CARTESIAN_POINT ( 'NONE',  ( -4.771743288812468897, -279.1233781216988064, -337.9199732462171255 ) ) ;
#50060 = CARTESIAN_POINT ( 'NONE',  ( -92.21201882117370019, -294.2990334148379930, -323.3889962992760161 ) ) ;
#50061 = CARTESIAN_POINT ( 'NONE',  ( -80.86302828035412915, -291.2537262982968400, -330.0261598545494053 ) ) ;
#50062 = CARTESIAN_POINT ( 'NONE',  ( -40.56667927183256950, -290.2520131233092684, -194.4299062573696517 ) ) ;
#50063 = CARTESIAN_POINT ( 'NONE',  ( -15.66086487428782981, -290.1914726447376438, -340.7373172693251604 ) ) ;
#50064 = FACE_OUTER_BOUND ( 'NONE', #9576, .T. ) ;
#50065 = CARTESIAN_POINT ( 'NONE',  ( -108.5051090615654488, -291.1314463266905932, -287.3426066244903723 ) ) ;
#50066 = CARTESIAN_POINT ( 'NONE',  ( 196.5738969053448102, 20.46081150943064841, 13.02005007215800880 ) ) ;
#50067 = CARTESIAN_POINT ( 'NONE',  ( -98.04307686021779489, -292.3841646566975214, -223.6135392585177897 ) ) ;
#50069 = CARTESIAN_POINT ( 'NONE',  ( -108.9387314423978665, -290.3634189425060868, -284.6681278710166794 ) ) ;
#50068 = CARTESIAN_POINT ( 'NONE',  ( 20.71985670166316140, -278.9125068340608777, -222.3271464094816565 ) ) ;
#50070 = CARTESIAN_POINT ( 'NONE',  ( -56.55548076943339453, -280.1444690109732392, -195.7636948748492500 ) ) ;
#50071 = AXIS2_PLACEMENT_3D ( 'NONE', #14387, #15763, #73525 ) ;
#50072 = CARTESIAN_POINT ( 'NONE',  ( 38.12398136993925135, -281.4088717274607347, -285.5491134939606468 ) ) ;
#50073 = CARTESIAN_POINT ( 'NONE',  ( 33.74412471680724934, -285.2428112635882371, -246.4486493887201277 ) ) ;
#50074 = DIRECTION ( 'NONE',  ( 0.000000000000000000, 0.000000000000000000, 1.000000000000000000 ) ) ;
#50075 = CARTESIAN_POINT ( 'NONE',  ( 36.58470641641360999, -279.5969270664867281, -263.0529110095594092 ) ) ;
#50076 = CARTESIAN_POINT ( 'NONE',  ( -92.43286910708727078, -283.2641184405466674, -219.3933482365070518 ) ) ;
#50077 = CARTESIAN_POINT ( 'NONE',  ( -96.26953907633355811, -277.6893924657188109, -221.8617626637910689 ) ) ;
#50078 = CARTESIAN_POINT ( 'NONE',  ( -30.89607534256120047, -285.0521122590863570, -193.9283342800665935 ) ) ;
#50079 = CARTESIAN_POINT ( 'NONE',  ( -59.53433503689885953, -274.5602605802951643, -200.5937402867422463 ) ) ;
#50080 = CARTESIAN_POINT ( 'NONE',  ( 183.0442525570908288, 264.6571197653884155, -7.500000000000000000 ) ) ;
#50081 = CARTESIAN_POINT ( 'NONE',  ( -84.35415942627538755, -292.9926427142486887, -213.4729022980585285 ) ) ;
#50082 = CARTESIAN_POINT ( 'NONE',  ( 21.38625716607874949, -276.3148224881030615, -221.4772420431311275 ) ) ;
#50083 = CARTESIAN_POINT ( 'NONE',  ( -40.51093074706013653, -276.7597824351230429, -343.3259228193078343 ) ) ;
#50084 = CARTESIAN_POINT ( 'NONE',  ( -8.437181790818337745, -296.6739735600254448, -339.5815254536943826 ) ) ;
#50085 = CARTESIAN_POINT ( 'NONE',  ( -74.68075533999848403, -291.7359748100731736, -203.0202317365652789 ) ) ;
#50086 = CARTESIAN_POINT ( 'NONE',  ( 9.941316325251293051, -278.7771292210996990, -211.3565232439137560 ) ) ;
#50087 = CARTESIAN_POINT ( 'NONE',  ( -19.38471394154651151, -292.1101746741380225, -195.4294187287191846 ) ) ;
#50088 = CARTESIAN_POINT ( 'NONE',  ( -30.77397403837677103, -291.1959548843082075, -197.4209135535824942 ) ) ;
#50089 = EDGE_CURVE ( 'NONE', #27188, #60755, #73996, .T. ) ;
#50090 = CARTESIAN_POINT ( 'NONE',  ( -67.44736475006726550, -293.4468762711809973, -339.0535455788008221 ) ) ;
#50091 = EDGE_LOOP ( 'NONE', ( #41627, #18893, #26637, #31497 ) ) ;
#50092 = DIRECTION ( 'NONE',  ( -1.000000000000000000, 0.000000000000000000, 0.000000000000000000 ) ) ;
#50093 = CARTESIAN_POINT ( 'NONE',  ( -25.39285698143028114, -291.7160795765324792, -198.2317651843381441 ) ) ;
#50094 = DIRECTION ( 'NONE',  ( -0.000000000000000000, -0.000000000000000000, -1.000000000000000000 ) ) ;
#50095 = CARTESIAN_POINT ( 'NONE',  ( -53.28691492658257545, -277.3380690714490129, -200.3538533559491555 ) ) ;
#50096 = CARTESIAN_POINT ( 'NONE',  ( -99.82399397337347580, -295.0173689200474882, -315.0464437874867940 ) ) ;
#50097 = CARTESIAN_POINT ( 'NONE',  ( -76.49105543292736797, -284.8791118413384424, -336.1540047253961916 ) ) ;
#50098 = CARTESIAN_POINT ( 'NONE',  ( 34.28374414271376480, -287.5723195959528198, -284.5252214534595510 ) ) ;
#50099 = CARTESIAN_POINT ( 'NONE',  ( -9.710604166538601589, -278.2046676643375349, -338.6919445080791320 ) ) ;
#50100 = CARTESIAN_POINT ( 'NONE',  ( 21.81156617014763555, -292.1991452502515472, -315.9093683592335537 ) ) ;
#50101 = CARTESIAN_POINT ( 'NONE',  ( -45.17601688878938404, -296.9127319196196026, -344.0098322273660187 ) ) ;
#50102 = CARTESIAN_POINT ( 'NONE',  ( 32.47115505635213140, -274.6460367698050504, -293.0171493173815520 ) ) ;
#50103 = ORIENTED_EDGE ( 'NONE', *, *, #39485, .F. ) ;
#50104 = CARTESIAN_POINT ( 'NONE',  ( 195.4404140996584829, 39.85136009038485838, 13.95084252573039763 ) ) ;
#50105 = CARTESIAN_POINT ( 'NONE',  ( -107.7519723514942456, -296.6174498148145062, -239.1144293489067536 ) ) ;
#50106 = CARTESIAN_POINT ( 'NONE',  ( -7.621527589300812089, -290.5798119572557425, -338.6659626074806511 ) ) ;
#50107 = CARTESIAN_POINT ( 'NONE',  ( -75.31992539360024352, -295.5460990252308306, -205.6290498907350752 ) ) ;
#50108 = CARTESIAN_POINT ( 'NONE',  ( -33.36826310765233217, -299.1804698133331613, -193.6695182843095608 ) ) ;
#50109 = CARTESIAN_POINT ( 'NONE',  ( 35.55423826032691181, -288.2841963085366501, -276.4816238167906022 ) ) ;
#50110 = ORIENTED_EDGE ( 'NONE', *, *, #20685, .T. ) ;
#50111 = CARTESIAN_POINT ( 'NONE',  ( -22.59958698792389242, -279.2950380960122061, -194.9711768236336979 ) ) ;
#50112 = CARTESIAN_POINT ( 'NONE',  ( -56.03746276239288449, -295.9382499612493120, -344.9518764302059139 ) ) ;
#50113 = CARTESIAN_POINT ( 'NONE',  ( -34.73345589466567418, -287.1592933305926181, -346.0810132864847333 ) ) ;
#50114 = CARTESIAN_POINT ( 'NONE',  ( -93.67110267242016164, -296.1698454997695080, -322.8471171985851242 ) ) ;
#50115 = CARTESIAN_POINT ( 'NONE',  ( 26.25088217052891437, -293.3930780179210274, -234.3681800691777539 ) ) ;
#50116 = CARTESIAN_POINT ( 'NONE',  ( 196.6009088602460508, 70.32516635541138328, -11.14992109073990534 ) ) ;
#50117 =( NAMED_UNIT ( * ) SI_UNIT ( $, .STERADIAN. ) SOLID_ANGLE_UNIT ( ) );
#50118 = FACE_BOUND ( 'NONE', #49651, .T. ) ;
#50119 = CARTESIAN_POINT ( 'NONE',  ( 9.370910816047025804, -288.2012664821090198, -210.0234039914137725 ) ) ;
#50120 = CARTESIAN_POINT ( 'NONE',  ( -72.08107566293803359, -292.9809262143061233, -342.4248175857292154 ) ) ;
#50121 = EDGE_LOOP ( 'NONE', ( #21391, #77531, #25219, #44496 ) ) ;
#50122 = CARTESIAN_POINT ( 'NONE',  ( -39.57597471101205855, -279.3734097633271176, -193.4824822536768636 ) ) ;
#50123 = CARTESIAN_POINT ( 'NONE',  ( -69.78142324358472592, -285.4804333033791295, -337.8118482579887427 ) ) ;
#50124 = CARTESIAN_POINT ( 'NONE',  ( -73.31940589933238073, -284.1596851414851699, -202.8917585195025879 ) ) ;
#50125 = CARTESIAN_POINT ( 'NONE',  ( -29.03626621203342850, -287.0259064076869890, -344.3363433242545284 ) ) ;
#50126 = CARTESIAN_POINT ( 'NONE',  ( -14.93206348330923738, -278.6254446777232943, -342.7908673877399224 ) ) ;
#50127 = CARTESIAN_POINT ( 'NONE',  ( -76.57916370595302169, -273.8443817128995761, -208.7777684575960961 ) ) ;
#50128 = ORIENTED_EDGE ( 'NONE', *, *, #76364, .T. ) ;
#50130 = CARTESIAN_POINT ( 'NONE',  ( -69.77806339610459929, -278.9619490247505951, -204.8356139435566377 ) ) ;
#50129 = CARTESIAN_POINT ( 'NONE',  ( -109.4920624883786360, -278.4056562853003243, -281.4663064671287884 ) ) ;
#50131 = CARTESIAN_POINT ( 'NONE',  ( -2.709484420801844706, -275.5788472459974514, -201.9205873271932887 ) ) ;
#50132 = CARTESIAN_POINT ( 'NONE',  ( -71.04598935865531928, -278.4121359248661634, -201.5713686886269613 ) ) ;
#50133 = CARTESIAN_POINT ( 'NONE',  ( 199.8333890556094445, 292.4321710294452146, -82.70894493957585780 ) ) ;
#50134 = CARTESIAN_POINT ( 'NONE',  ( -68.75876545373007787, -274.5904350790960393, -200.3054333886574057 ) ) ;
#50135 = CONTEXT_DEPENDENT_SHAPE_REPRESENTATION ( #10570, #85995 ) ;
#50136 = CARTESIAN_POINT ( 'NONE',  ( -93.24416139441676421, -298.6936684336129133, -218.1924502067773517 ) ) ;
#50137 = CARTESIAN_POINT ( 'NONE',  ( -114.2704648735229114, -281.0519495502701943, -270.3937649182068981 ) ) ;
#50138 = ORIENTED_EDGE ( 'NONE', *, *, #76026, .T. ) ;
#50139 = DIRECTION ( 'NONE',  ( 0.000000000000000000, 0.000000000000000000, 1.000000000000000000 ) ) ;
#50140 = AXIS2_PLACEMENT_3D ( 'NONE', #40834, #91514, #3014 ) ;
#50141 = CARTESIAN_POINT ( 'NONE',  ( -67.68815348001666621, -286.7239670075643403, -203.6279265148333479 ) ) ;
#50142 = CARTESIAN_POINT ( 'NONE',  ( -109.9643034278956435, -286.5988573135857109, -247.8246976550084355 ) ) ;
#50143 = CARTESIAN_POINT ( 'NONE',  ( 22.82909333039162192, -287.4783642228019858, -311.8966500789242104 ) ) ;
#50144 = CARTESIAN_POINT ( 'NONE',  ( -113.0775286048948090, -283.8865432466141669, -284.2040875715013613 ) ) ;
#50145 = CARTESIAN_POINT ( 'NONE',  ( 30.76755446176559872, -279.5749607082762509, -241.9433444497237531 ) ) ;
#50146 = CARTESIAN_POINT ( 'NONE',  ( -52.36161242444706687, -287.7181875857285718, -197.6612712695019241 ) ) ;
#50147 = CARTESIAN_POINT ( 'NONE',  ( 36.04468346152054181, -279.9371662121584450, -263.1021184434431461 ) ) ;
#50148 = CARTESIAN_POINT ( 'NONE',  ( -4.832970197590103822, -277.9300333096678060, -336.2873630374841696 ) ) ;
#50149 = CARTESIAN_POINT ( 'NONE',  ( 20.72662636625302568, -275.4212153638341078, -226.0002756500364569 ) ) ;
#50150 = CARTESIAN_POINT ( 'NONE',  ( 9.970589359451627942, -287.2119452762335072, -330.6743853095651389 ) ) ;
#50151 = CIRCLE ( 'NONE', #60776, 25.00000000000000355 ) ;
#50152 = CARTESIAN_POINT ( 'NONE',  ( -70.39137737591944699, -284.2795210547388933, -339.7432474565546272 ) ) ;
#50153 = CARTESIAN_POINT ( 'NONE',  ( -83.84101961225024979, -284.1635088935872773, -331.7251853140549542 ) ) ;
#50154 = CARTESIAN_POINT ( 'NONE',  ( 20.51462576511756808, -281.0920973096517059, -225.8251247738890868 ) ) ;
#50155 = ORIENTED_EDGE ( 'NONE', *, *, #80951, .F. ) ;
#50156 = EDGE_LOOP ( 'NONE', ( #5918, #64596, #9579, #31866 ) ) ;
#50157 = DIRECTION ( 'NONE',  ( 0.000000000000000000, 0.000000000000000000, 1.000000000000000000 ) ) ;
#50158 = CARTESIAN_POINT ( 'NONE',  ( -62.33348748119884419, -291.2340923457712734, -341.9408250797640676 ) ) ;
#50159 = CARTESIAN_POINT ( 'NONE',  ( -91.26292635598746017, -288.4839421182418846, -324.7108808063657079 ) ) ;
#50160 = CARTESIAN_POINT ( 'NONE',  ( -40.77400899137278856, -273.0668063828048275, -197.1564365014620250 ) ) ;
#50161 = EDGE_CURVE ( 'NONE', #77282, #32191, #55899, .T. ) ;
#50162 = CARTESIAN_POINT ( 'NONE',  ( 39.50471661373507715, -292.9360296936184795, -273.1790995700564508 ) ) ;
#50163 = CARTESIAN_POINT ( 'NONE',  ( -102.2630339598794365, -288.5597252499873662, -305.3395242598816139 ) ) ;
#50164 = CARTESIAN_POINT ( 'NONE',  ( 24.19606324295878963, -291.2287696727721595, -229.2384029351687786 ) ) ;
#50165 = CARTESIAN_POINT ( 'NONE',  ( 20.64497273588014536, -288.1268572152636693, -225.3647150568420159 ) ) ;
#50166 = CARTESIAN_POINT ( 'NONE',  ( -110.4542110544635705, -286.8376638359844719, -287.0812184334320705 ) ) ;
#50167 = CARTESIAN_POINT ( 'NONE',  ( 29.90575366690926984, -289.9917707621133331, -303.6864665132742971 ) ) ;
#50168 = CARTESIAN_POINT ( 'NONE',  ( -110.7797619687470956, -288.3466611540799249, -286.3885789207768084 ) ) ;
#50169 = CARTESIAN_POINT ( 'NONE',  ( -35.89714563425030747, -294.0703967668365522, -195.3623998638208548 ) ) ;
#50170 = CARTESIAN_POINT ( 'NONE',  ( -65.39477605066088017, -284.3693414041481446, -338.0241005783956325 ) ) ;
#50171 = CARTESIAN_POINT ( 'NONE',  ( 24.95875597068581087, -294.9835569251786751, -228.2139041085275153 ) ) ;
#50172 = CARTESIAN_POINT ( 'NONE',  ( 200.2296996224750103, 68.12454877784578855, -2.194831983251746443 ) ) ;
#50173 = EDGE_CURVE ( 'NONE', #6854, #10377, #26802, .T. ) ;
#50174 = DIRECTION ( 'NONE',  ( 0.000000000000000000, 0.000000000000000000, -1.000000000000000000 ) ) ;
#50175 = CARTESIAN_POINT ( 'NONE',  ( -105.3694235135199904, -274.9566242683296196, -237.9476076708264429 ) ) ;
#50176 = CARTESIAN_POINT ( 'NONE',  ( -36.20124657383839661, -282.2346565089146679, -343.5137057234255735 ) ) ;
#50177 = CARTESIAN_POINT ( 'NONE',  ( -90.32473010579826678, -281.8011817670309256, -323.5169858690355227 ) ) ;
#50178 = CARTESIAN_POINT ( 'NONE',  ( -68.17079532744206460, -294.6440106118486142, -340.7438268683401930 ) ) ;
#50179 = CARTESIAN_POINT ( 'NONE',  ( 23.90328057740336831, -273.2217536208866591, -228.7808688120199463 ) ) ;
#50180 = CARTESIAN_POINT ( 'NONE',  ( -92.04230275899415403, -275.9202631479766978, -320.9253149356404720 ) ) ;
#50181 = CARTESIAN_POINT ( 'NONE',  ( -69.48826278308541760, -298.9350781951204681, -204.2714668322632576 ) ) ;
#50182 = CARTESIAN_POINT ( 'NONE',  ( 10.68972029633187937, -295.7980480551170785, -326.1137642656909179 ) ) ;
#50183 = CARTESIAN_POINT ( 'NONE',  ( 175.2296996224750103, 154.6894116713782807, 0.000000000000000000 ) ) ;
#50184 = CARTESIAN_POINT ( 'NONE',  ( -42.39068516581224344, -295.9202903350091560, -343.3481680476940028 ) ) ;
#50185 = CARTESIAN_POINT ( 'NONE',  ( 208.6208076322478746, 32.98517505407394168, 14.26380412667038655 ) ) ;
#50187 = CARTESIAN_POINT ( 'NONE',  ( -105.8058295604936063, -296.8916587374533265, -244.8842449792233822 ) ) ;
#50186 = CARTESIAN_POINT ( 'NONE',  ( 38.05633600158335383, -285.5874632921277794, -271.5510281369199106 ) ) ;
#50188 = CARTESIAN_POINT ( 'NONE',  ( 38.95487779611155332, -287.0909434536848153, -260.1348533389456179 ) ) ;
#50189 = CARTESIAN_POINT ( 'NONE',  ( 21.02892139838816021, -296.1858743455904914, -318.0393037442775039 ) ) ;
#50190 = CARTESIAN_POINT ( 'NONE',  ( 37.02594314257099484, -291.6650951413106441, -279.1505413507780418 ) ) ;
#50191 = CARTESIAN_POINT ( 'NONE',  ( -61.98614075014549485, -278.9370407720724074, -197.5258170954137711 ) ) ;
#50192 = CARTESIAN_POINT ( 'NONE',  ( -20.25526795762938548, -286.3380690714490697, -345.3683826091709648 ) ) ;
#50193 = CARTESIAN_POINT ( 'NONE',  ( 17.19589066053204007, -285.6473943493583647, -221.2222758851342235 ) ) ;
#50194 = DIRECTION ( 'NONE',  ( -0.000000000000000000, -1.000000000000000000, -0.000000000000000000 ) ) ;
#50195 = CARTESIAN_POINT ( 'NONE',  ( 207.6175730408113509, 30.32598770090650575, 14.41714557868298741 ) ) ;
#50196 = CARTESIAN_POINT ( 'NONE',  ( -109.8353168242309010, -298.3335539051417982, -256.4692476335356446 ) ) ;
#50197 = CARTESIAN_POINT ( 'NONE',  ( -17.16518032620580669, -281.7329341780680920, -196.6623097148463160 ) ) ;
#50199 = CARTESIAN_POINT ( 'NONE',  ( 35.70282396646855716, -281.5647190748069306, -271.3137581944124008 ) ) ;
#50198 = CARTESIAN_POINT ( 'NONE',  ( -112.6929954034260390, -294.5820657255896435, -269.5935894327433857 ) ) ;
#50200 = CARTESIAN_POINT ( 'NONE',  ( -114.2336749270550769, -296.6565454245620117, -275.3414882687744125 ) ) ;
#50201 = CARTESIAN_POINT ( 'NONE',  ( -107.7656868571581157, -274.2599289040125541, -248.8360794169643100 ) ) ;
#50202 = CARTESIAN_POINT ( 'NONE',  ( -35.16475450806476033, -284.1591034817870423, -194.8195829246140534 ) ) ;
#50203 = CARTESIAN_POINT ( 'NONE',  ( 34.25858975496183234, -283.2643670651485195, -248.0362632730956136 ) ) ;
#50204 = CARTESIAN_POINT ( 'NONE',  ( -94.62790106707559801, -296.2531683619527030, -224.7354713465992120 ) ) ;
#50205 = AXIS2_PLACEMENT_3D ( 'NONE', #34444, #85556, #93581 ) ;
#50206 = DIRECTION ( 'NONE',  ( 0.000000000000000000, 0.000000000000000000, 1.000000000000000000 ) ) ;
#50208 = CARTESIAN_POINT ( 'NONE',  ( -54.03348678089458446, -285.2472652557833044, -343.1689661315664921 ) ) ;
#50207 = VECTOR ( 'NONE', #65942, 1000.000000000000000 ) ;
#50209 = DIRECTION ( 'NONE',  ( -1.000000000000000000, -0.000000000000000000, 0.000000000000000000 ) ) ;
#50210 = CARTESIAN_POINT ( 'NONE',  ( 31.95455697924147032, -291.4809262143061233, -303.7686719486574702 ) ) ;
#50211 = CARTESIAN_POINT ( 'NONE',  ( 27.50704705598299782, -275.2917780826409171, -311.6764883431170574 ) ) ;
#50212 = CARTESIAN_POINT ( 'NONE',  ( -44.29809233384927580, -291.7951796514071816, -197.6425038824307876 ) ) ;
#50213 = CIRCLE ( 'NONE', #89517, 1.500000000000001332 ) ;
#50214 = CARTESIAN_POINT ( 'NONE',  ( 0.7418328627382330120, -282.0897158423945825, -207.2120225293148508 ) ) ;
#50215 = CARTESIAN_POINT ( 'NONE',  ( -4.694036087942145663, -278.2149415568750896, -336.5610401846183777 ) ) ;
#50216 = CARTESIAN_POINT ( 'NONE',  ( 27.63362223826922559, -283.6789670515210560, -310.2687905128263424 ) ) ;
#50217 = CARTESIAN_POINT ( 'NONE',  ( 18.27539814306031829, -279.6684910955020200, -222.4474687750023350 ) ) ;
#50218 = CARTESIAN_POINT ( 'NONE',  ( -110.2394639135455208, -280.7787490049236112, -252.7282881482385619 ) ) ;
#50219 = CARTESIAN_POINT ( 'NONE',  ( -20.50992399667585886, -298.2574375460679335, -193.3611160711894854 ) ) ;
#50220 = CARTESIAN_POINT ( 'NONE',  ( 20.81885638852990184, -276.0675619174349436, -320.8424411334291335 ) ) ;
#50221 = CARTESIAN_POINT ( 'NONE',  ( 20.83417430341074095, -296.1158046415303602, -316.8236891720168273 ) ) ;
#50222 = CARTESIAN_POINT ( 'NONE',  ( 202.8019728163925777, 61.40723988820082724, -9.000000000000000000 ) ) ;
#50223 = DIRECTION ( 'NONE',  ( 0.000000000000000000, 0.000000000000000000, -1.000000000000000000 ) ) ;
#50224 = CARTESIAN_POINT ( 'NONE',  ( 3.540531325833613074, -292.6486151179939839, -334.2111870952561503 ) ) ;
#50225 = CARTESIAN_POINT ( 'NONE',  ( 20.73426050244066587, -274.4366802819465647, -226.0102708529038296 ) ) ;
#50226 = CARTESIAN_POINT ( 'NONE',  ( 37.37900150782583353, -294.8761462264361626, -254.8205746371423004 ) ) ;
#50227 = CARTESIAN_POINT ( 'NONE',  ( -8.674131915659689440, -293.6241456497128297, -199.3246537432844718 ) ) ;
#50228 = CARTESIAN_POINT ( 'NONE',  ( -70.76904965004152359, -291.4942087341351566, -337.3278481484095437 ) ) ;
#50229 = CARTESIAN_POINT ( 'NONE',  ( -110.8488235094794163, -276.3706251407230639, -284.4550345326309184 ) ) ;
#50230 = CARTESIAN_POINT ( 'NONE',  ( -10.71659673397097734, -278.6223347687520686, -339.8767138388106446 ) ) ;
#50231 = EDGE_CURVE ( 'NONE', #20997, #30715, #85011, .T. ) ;
#50232 = CARTESIAN_POINT ( 'NONE',  ( -26.01189438197866366, -292.9866028714436652, -343.9338690352085450 ) ) ;
#50233 = CARTESIAN_POINT ( 'NONE',  ( 28.69708180864721214, -283.9034567176025234, -307.6054775750404815 ) ) ;
#50234 = CARTESIAN_POINT ( 'NONE',  ( -70.10830499006489447, -284.5303195975483845, -204.7683412375857301 ) ) ;
#50235 = ORIENTED_EDGE ( 'NONE', *, *, #59139, .T. ) ;
#50236 = CARTESIAN_POINT ( 'NONE',  ( -2.422284508983608031, -282.2433995548834673, -334.5059178052410971 ) ) ;
#50237 = CARTESIAN_POINT ( 'NONE',  ( -73.63155621386408711, -280.6617505313870993, -202.7848550276897868 ) ) ;
#50238 = CARTESIAN_POINT ( 'NONE',  ( -80.70074920807873298, -284.2735415023436190, -207.1464733336419783 ) ) ;
#50239 = CARTESIAN_POINT ( 'NONE',  ( -109.3895241792176733, -279.8310018279798896, -243.7136017212736476 ) ) ;
#50240 = CARTESIAN_POINT ( 'NONE',  ( -68.71248336467130002, -278.9771483566601091, -339.9353054930013514 ) ) ;
#50241 = CARTESIAN_POINT ( 'NONE',  ( 17.36665895637874613, -295.4090924074130839, -226.6919474004047572 ) ) ;
#50242 = ORIENTED_EDGE ( 'NONE', *, *, #82641, .F. ) ;
#50243 = ORIENTED_EDGE ( 'NONE', *, *, #53950, .F. ) ;
#50244 = CARTESIAN_POINT ( 'NONE',  ( -83.18623497663864441, -299.4249573779193270, -210.9380631999358968 ) ) ;
#50245 = CARTESIAN_POINT ( 'NONE',  ( -36.97551065040104845, -278.0768702752188801, -195.7172119192860862 ) ) ;
#50246 = CARTESIAN_POINT ( 'NONE',  ( -50.41435204032848816, -293.6475800832835148, -195.5073954061652444 ) ) ;
#50247 = CARTESIAN_POINT ( 'NONE',  ( 25.87666342129961805, -293.4036242026455739, -307.0671280911795407 ) ) ;
#50248 = CARTESIAN_POINT ( 'NONE',  ( -113.9449388050913825, -290.1564855603656952, -262.6368981308480670 ) ) ;
#50249 = LINE ( 'NONE', #48847, #27876 ) ;
#50251 = CARTESIAN_POINT ( 'NONE',  ( -30.43635620055726676, -284.5406554786366655, -196.8335303357073087 ) ) ;
#50250 = CARTESIAN_POINT ( 'NONE',  ( 37.48983357727624366, -292.3216586563302144, -285.8158214122535696 ) ) ;
#50252 = CARTESIAN_POINT ( 'NONE',  ( -88.80365871201126993, -293.1810922391674126, -216.7874161164737643 ) ) ;
#50253 = CARTESIAN_POINT ( 'NONE',  ( -42.95397476381405966, -284.4395045866243095, -343.6900928545240959 ) ) ;
#50254 = CARTESIAN_POINT ( 'NONE',  ( -111.3120250584146191, -291.2354814739172753, -290.8845495444705875 ) ) ;
#50255 = CARTESIAN_POINT ( 'NONE',  ( -30.26265832149410073, -280.6363286675345989, -197.5929399114839669 ) ) ;
#50256 = CARTESIAN_POINT ( 'NONE',  ( 39.04626408082600619, -292.2749854261301721, -264.6263432063596497 ) ) ;
#50257 = CARTESIAN_POINT ( 'NONE',  ( -70.55998728160321321, -290.2818027360690962, -339.6626870678834393 ) ) ;
#50258 = CARTESIAN_POINT ( 'NONE',  ( -111.8608620435123697, -290.8041557688309240, -289.5559425867264167 ) ) ;
#50259 = CARTESIAN_POINT ( 'NONE',  ( -106.5329923461504791, -285.0298482026460078, -246.9312712180887104 ) ) ;
#50260 = VERTEX_POINT ( 'NONE', #69886 ) ;
#50261 = CARTESIAN_POINT ( 'NONE',  ( 186.6539576904058890, 293.9636489450775230, 9.103929867429224387 ) ) ;
#50262 = CARTESIAN_POINT ( 'NONE',  ( 38.20757594392513568, -295.3399833929092893, -264.6503944321192989 ) ) ;
#50263 = CARTESIAN_POINT ( 'NONE',  ( -97.89448193200388459, -294.6088082618283579, -317.1228426132867639 ) ) ;
#50264 = CARTESIAN_POINT ( 'NONE',  ( -91.46264729407023708, -278.3161502095563833, -221.0221726530852777 ) ) ;
#50265 = EDGE_CURVE ( 'NONE', #83798, #63080, #70378, .T. ) ;
#50266 = CARTESIAN_POINT ( 'NONE',  ( -95.97671714198153836, -272.7320661652116200, -220.5265633770405032 ) ) ;
#50267 = CARTESIAN_POINT ( 'NONE',  ( -95.33090054539448488, -294.3968480552210281, -315.8359504680674945 ) ) ;
#50268 = CARTESIAN_POINT ( 'NONE',  ( 32.06085759139318725, -276.9740805369317513, -244.6461613591418995 ) ) ;
#50269 = CARTESIAN_POINT ( 'NONE',  ( -83.94798291180906347, -271.5435275721050061, -212.5794610098595285 ) ) ;
#50270 = AXIS2_PLACEMENT_3D ( 'NONE', #79753, #57067, #22445 ) ;
#50271 = CARTESIAN_POINT ( 'NONE',  ( 34.60267695094090357, -294.5665856550675699, -255.8305600918416758 ) ) ;
#50272 = CARTESIAN_POINT ( 'NONE',  ( -95.84273018092272878, -297.0135626204751702, -314.5616018979806654 ) ) ;
#50273 = CARTESIAN_POINT ( 'NONE',  ( 221.5917695054402543, 1.242640687119284992, 9.999999999999998224 ) ) ;
#50274 = CIRCLE ( 'NONE', #35141, 1.499999999999998002 ) ;
#50275 = CARTESIAN_POINT ( 'NONE',  ( -111.5748610248523249, -294.7043319690050112, -258.4701674731024355 ) ) ;
#50276 = CARTESIAN_POINT ( 'NONE',  ( -75.73621665072249698, -298.2054887986585641, -203.6728771563084592 ) ) ;
#50277 = CARTESIAN_POINT ( 'NONE',  ( 33.64550499664232319, -286.3832993171898806, -289.9456977756863125 ) ) ;
#50278 = CARTESIAN_POINT ( 'NONE',  ( -60.10630012970916169, -275.7573956496621577, -198.8450460799258224 ) ) ;
#50279 = CARTESIAN_POINT ( 'NONE',  ( -110.6034901111379440, -291.5183084014535666, -268.4675968260048080 ) ) ;
#50280 = CARTESIAN_POINT ( 'NONE',  ( -73.92113913693324889, -274.0723617322286145, -202.6153224273677722 ) ) ;
#50282 = CARTESIAN_POINT ( 'NONE',  ( -99.91710299353974278, -297.4042943384935143, -232.6276017677705568 ) ) ;
#50281 = VECTOR ( 'NONE', #56137, 1000.000000000000000 ) ;
#50283 = AXIS2_PLACEMENT_3D ( 'NONE', #66129, #59010, #93124 ) ;
#50284 = CARTESIAN_POINT ( 'NONE',  ( -109.8508240012940149, -280.2693194364147189, -290.8753510809888212 ) ) ;
#50285 = CARTESIAN_POINT ( 'NONE',  ( 35.70984346184874170, -279.9495675700271136, -247.6285366970083714 ) ) ;
#50286 = VERTEX_POINT ( 'NONE', #40964 ) ;
#50287 = CARTESIAN_POINT ( 'NONE',  ( -16.17786546318904684, -282.1342298324216813, -344.3447053673556297 ) ) ;
#50288 = CARTESIAN_POINT ( 'NONE',  ( 39.27823336103507046, -274.9825707383294571, -276.8955329131857184 ) ) ;
#50289 = CARTESIAN_POINT ( 'NONE',  ( -92.48064189481800668, -277.6793742011579980, -217.6916684475944805 ) ) ;
#50290 = CARTESIAN_POINT ( 'NONE',  ( -58.75490761657733430, -277.7756543150019866, -198.3090328693548940 ) ) ;
#50291 = EDGE_CURVE ( 'NONE', #37664, #48386, #26331, .T. ) ;
#50292 = CARTESIAN_POINT ( 'NONE',  ( -75.45214434226805622, -296.2175574461771816, -207.4623457955987362 ) ) ;
#50293 = CARTESIAN_POINT ( 'NONE',  ( 22.97339870047947130, -278.1607918486978406, -314.9591988313621869 ) ) ;
#50294 = CARTESIAN_POINT ( 'NONE',  ( 208.6208076322478746, 32.98517505407394168, 14.49999999999999822 ) ) ;
#50295 = CARTESIAN_POINT ( 'NONE',  ( -61.14460228282200660, -289.7648841358002301, -198.8091138861177569 ) ) ;
#50296 = CARTESIAN_POINT ( 'NONE',  ( -100.0310483308176828, -291.1443451806417784, -225.6504299771615365 ) ) ;
#50297 = CARTESIAN_POINT ( 'NONE',  ( -16.31521333151226827, -276.3233417229643578, -198.1412156074836446 ) ) ;
#50298 = CARTESIAN_POINT ( 'NONE',  ( -110.4797419884152845, -270.7652409156175395, -253.7530631127523577 ) ) ;
#50299 = CARTESIAN_POINT ( 'NONE',  ( -107.7740140549030770, -284.1432294191976098, -239.5125219399257901 ) ) ;
#50300 = CARTESIAN_POINT ( 'NONE',  ( 215.9306832106270804, -198.2391364535880598, 9.184850993605173582E-16 ) ) ;
#50301 = CARTESIAN_POINT ( 'NONE',  ( -110.5914043820631605, -282.3444769689195937, -286.5279133427056308 ) ) ;
#50302 = AXIS2_PLACEMENT_3D ( 'NONE', #12856, #83373, #54502 ) ;
#50303 = CARTESIAN_POINT ( 'NONE',  ( 183.0442525570908288, 296.7472757692770529, 7.499999999999996447 ) ) ;
#50304 = CARTESIAN_POINT ( 'NONE',  ( 22.13543961663703996, -291.7484484370533551, -227.3327597997061105 ) ) ;
#50305 = CARTESIAN_POINT ( 'NONE',  ( -38.62285886196762164, -284.1755375516056006, -196.1242769990700197 ) ) ;
#50306 = CARTESIAN_POINT ( 'NONE',  ( 164.2231345125756263, 293.9636489450775230, 0.000000000000000000 ) ) ;
#50307 = CARTESIAN_POINT ( 'NONE',  ( 204.7786681169002350, 32.98517505407394168, 13.99999999999999822 ) ) ;
#50308 = CARTESIAN_POINT ( 'NONE',  ( -56.33370758817049051, -293.2965588918303297, -342.9704675057781742 ) ) ;
#50309 = CARTESIAN_POINT ( 'NONE',  ( -111.5494764710839917, -282.8070314947411248, -288.1904484659032164 ) ) ;
#50310 = CARTESIAN_POINT ( 'NONE',  ( -97.06497439797817606, -280.7524148827258728, -227.0070994037915568 ) ) ;
#50311 = CARTESIAN_POINT ( 'NONE',  ( -113.4270414053005425, -285.8689813377288260, -261.4712607929455999 ) ) ;
#50312 = CARTESIAN_POINT ( 'NONE',  ( -9.215084572556941467, -278.6547507738487184, -199.7716888058341453 ) ) ;
#50313 = CARTESIAN_POINT ( 'NONE',  ( 26.36738027536458873, -287.0634180033556504, -234.6184865306303209 ) ) ;
#50314 = CARTESIAN_POINT ( 'NONE',  ( -110.4876238152767485, -279.8660062091835243, -278.8758744569841497 ) ) ;
#50315 = CARTESIAN_POINT ( 'NONE',  ( -109.4434800205092984, -279.1907055100448929, -282.8421648300742959 ) ) ;
#50316 = CARTESIAN_POINT ( 'NONE',  ( -10.60172030037941404, -288.3789836559200808, -199.8542767404049982 ) ) ;
#50317 = VERTEX_POINT ( 'NONE', #5964 ) ;
#50318 = CARTESIAN_POINT ( 'NONE',  ( -26.20759799648282851, -298.0212679064690633, -193.3614219870460147 ) ) ;
#50319 = CARTESIAN_POINT ( 'NONE',  ( -7.539123811414215837, -290.6395404315176165, -338.8536064857112819 ) ) ;
#50320 = CARTESIAN_POINT ( 'NONE',  ( 197.4836817735085219, 24.47698789593438917, 11.66666666666666963 ) ) ;
#50321 = CARTESIAN_POINT ( 'NONE',  ( -99.86837403722181250, -286.4090924074130839, -320.2651865833026363 ) ) ;
#50322 = EDGE_LOOP ( 'NONE', ( #9615, #26843, #11694, #5670 ) ) ;
#50323 = CARTESIAN_POINT ( 'NONE',  ( -54.88053346861718040, -271.8270095330213962, -197.2692733724240384 ) ) ;
#50324 = CARTESIAN_POINT ( 'NONE',  ( 35.94046486524361228, -291.6869468967016701, -249.4289712438227298 ) ) ;
#50325 = CARTESIAN_POINT ( 'NONE',  ( 36.34866108994013700, -289.0809342277619294, -271.0232464093949716 ) ) ;
#50326 = CARTESIAN_POINT ( 'NONE',  ( 35.05171798619566914, -283.1111659630980171, -254.9005914110520905 ) ) ;
#50327 = CARTESIAN_POINT ( 'NONE',  ( 9.878179787375804821, -289.8418700464339395, -330.5024744715683482 ) ) ;
#50328 = CARTESIAN_POINT ( 'NONE',  ( 36.67161757024006619, -289.1113873841904933, -289.7344779729380093 ) ) ;
#50329 = CARTESIAN_POINT ( 'NONE',  ( -109.6837122555746191, -286.2972642358467397, -290.1992865056311075 ) ) ;
#50330 = CARTESIAN_POINT ( 'NONE',  ( -113.7659728382104447, -278.5960129198955997, -280.1816053145672072 ) ) ;
#50331 = ORIENTED_EDGE ( 'NONE', *, *, #22726, .F. ) ;
#50332 = CARTESIAN_POINT ( 'NONE',  ( -50.24610959810592448, -293.2953341788693820, -344.8639751174833918 ) ) ;
#50333 = CARTESIAN_POINT ( 'NONE',  ( 39.52902354657486939, -281.4517800365271682, -275.6630135752549791 ) ) ;
#50335 = CARTESIAN_POINT ( 'NONE',  ( 97.65637974683852462, -301.6750618930004748, -195.8765629805787682 ) ) ;
#50334 = CIRCLE ( 'NONE', #9491, 3.000000000000000000 ) ;
#50336 = CARTESIAN_POINT ( 'NONE',  ( 10.64812456238590066, -284.9090924074130271, -330.4860931364851808 ) ) ;
#50337 = CARTESIAN_POINT ( 'NONE',  ( -92.42198639639629221, -271.5171745323133905, -217.9958269592325166 ) ) ;
#50339 = AXIS2_PLACEMENT_3D ( 'NONE', #62660, #90091, #41289 ) ;
#50338 = DIRECTION ( 'NONE',  ( 0.000000000000000000, 1.000000000000000000, 0.000000000000000000 ) ) ;
#50340 = CARTESIAN_POINT ( 'NONE',  ( -72.15351379383706387, -279.0860899361107954, -206.1261892359662511 ) ) ;
#50341 = AXIS2_PLACEMENT_3D ( 'NONE', #26152, #39873, #11486 ) ;
#50342 = CARTESIAN_POINT ( 'NONE',  ( -14.69237671000794521, -277.9702099961260160, -343.5946400563753969 ) ) ;
#50343 = CARTESIAN_POINT ( 'NONE',  ( -35.14369412956378369, -299.5054696142980220, -196.7713390149831696 ) ) ;
#50344 = CARTESIAN_POINT ( 'NONE',  ( -112.9075215949943782, -283.4377109778860131, -284.1671756000792470 ) ) ;
#50345 = CARTESIAN_POINT ( 'NONE',  ( -103.3229610897474373, -292.7628101456688228, -236.7148213140268069 ) ) ;
#50346 = CARTESIAN_POINT ( 'NONE',  ( -52.40759924451852925, -275.4625770938109213, -195.6114626430798182 ) ) ;
#50347 = VECTOR ( 'NONE', #66392, 1000.000000000000000 ) ;
#50348 = CARTESIAN_POINT ( 'NONE',  ( -64.73922498883916887, -275.0169447323681311, -198.9140188814967019 ) ) ;
#50349 = CARTESIAN_POINT ( 'NONE',  ( 37.36314606568671337, -295.4854416488993252, -265.1642700852298162 ) ) ;
#50350 = CARTESIAN_POINT ( 'NONE',  ( -93.04636888076693424, -281.8542081291388968, -320.3505817338285624 ) ) ;
#50351 = AXIS2_PLACEMENT_3D ( 'NONE', #29704, #73260, #88368 ) ;
#50352 = CARTESIAN_POINT ( 'NONE',  ( -90.76820565737011748, -290.9863102207815473, -214.8673551589249371 ) ) ;
#50353 = CARTESIAN_POINT ( 'NONE',  ( -16.15009226224445626, -272.3474548112154139, -198.7337390904931738 ) ) ;
#50354 = CARTESIAN_POINT ( 'NONE',  ( -49.24012302223133730, -287.5032021760997623, -195.0426219151532052 ) ) ;
#50355 = CARTESIAN_POINT ( 'NONE',  ( -110.0046263325880034, -289.6049936938659357, -260.2730099703517794 ) ) ;
#50356 = ORIENTED_EDGE ( 'NONE', *, *, #49297, .T. ) ;
#50357 = CARTESIAN_POINT ( 'NONE',  ( -91.19622158036550275, -288.3738615785473485, -324.6416262466795501 ) ) ;
#50358 = CARTESIAN_POINT ( 'NONE',  ( -39.96306329981003103, -288.7525814210067097, -343.3847879840174642 ) ) ;
#50359 = ORIENTED_EDGE ( 'NONE', *, *, #65811, .T. ) ;
#50360 = CARTESIAN_POINT ( 'NONE',  ( -18.27223636199831702, -287.3718466160934213, -196.0240202023492202 ) ) ;
#50361 = AXIS2_PLACEMENT_3D ( 'NONE', #29313, #50622, #93689 ) ;
#50362 = CARTESIAN_POINT ( 'NONE',  ( -27.01432979943238522, -277.2505004070605992, -342.6482738873991707 ) ) ;
#50363 = EDGE_CURVE ( 'NONE', #29264, #78013, #13531, .T. ) ;
#50364 = CARTESIAN_POINT ( 'NONE',  ( 30.63134982468524470, -292.0111811076992581, -234.7339838467658240 ) ) ;
#50365 = CARTESIAN_POINT ( 'NONE',  ( -114.2388749865937285, -285.2082041814914533, -269.9905980131128445 ) ) ;
#50366 = CARTESIAN_POINT ( 'NONE',  ( -111.4699639621629217, -284.6252924125633399, -291.1155101083857062 ) ) ;
#50367 = CARTESIAN_POINT ( 'NONE',  ( -51.83570800445956195, -280.1949714541942171, -198.7411442248631772 ) ) ;
#50368 = CARTESIAN_POINT ( 'NONE',  ( 154.3179510270316825, 206.9283153158852997, -217.4371041850278630 ) ) ;
#50369 = CARTESIAN_POINT ( 'NONE',  ( -72.06973415904727176, -195.5151140978756246, -359.6196184014357300 ) ) ;
#50370 = CARTESIAN_POINT ( 'NONE',  ( -109.3056031691116488, -263.8853751231396814, -305.5667918931541749 ) ) ;
#50371 = CARTESIAN_POINT ( 'NONE',  ( -14.00427616992897839, -273.5599878219673542, -201.0216171930390772 ) ) ;
#50372 = CARTESIAN_POINT ( 'NONE',  ( 34.42677511111907052, -274.2752844536925636, -255.3494618599178523 ) ) ;
#50373 = CARTESIAN_POINT ( 'NONE',  ( -105.9057119658662884, -295.6086158138003270, -305.3855614695280565 ) ) ;
#50374 = CARTESIAN_POINT ( 'NONE',  ( -109.1997399844073584, -269.5207596422944789, -295.4475377585682736 ) ) ;
#50375 = CARTESIAN_POINT ( 'NONE',  ( -43.98314901247594833, -272.6548208346287652, -194.0901128034429064 ) ) ;
#50376 = CARTESIAN_POINT ( 'NONE',  ( -72.26672099815004913, -299.4454364413379608, -204.8401254970598870 ) ) ;
#50377 = CARTESIAN_POINT ( 'NONE',  ( 34.18488191215580940, -289.0886210737508577, -287.2487330086863153 ) ) ;
#50378 = ORIENTED_EDGE ( 'NONE', *, *, #43406, .F. ) ;
#50379 = CARTESIAN_POINT ( 'NONE',  ( -113.9980744054674631, -297.4309926713159484, -275.3361058418064999 ) ) ;
#50380 = CARTESIAN_POINT ( 'NONE',  ( -70.01557291589455190, -286.1020837837185127, -204.9988144284792497 ) ) ;
#50381 = CARTESIAN_POINT ( 'NONE',  ( -67.40176349790807819, -272.5873438394476125, -199.8069891131355291 ) ) ;
#50382 = AXIS2_PLACEMENT_3D ( 'NONE', #34613, #27037, #10943 ) ;
#50383 = CARTESIAN_POINT ( 'NONE',  ( 36.92387453727684488, -294.1070301515349570, -250.5927937790800684 ) ) ;
#50384 = CARTESIAN_POINT ( 'NONE',  ( 6.584014889699429496, -294.9652480824167924, -333.5929473193716035 ) ) ;
#50385 = CARTESIAN_POINT ( 'NONE',  ( -79.53243520000641809, -291.6313249584576965, -210.7261612519274649 ) ) ;
#50386 = ORIENTED_EDGE ( 'NONE', *, *, #28465, .F. ) ;
#50387 = CARTESIAN_POINT ( 'NONE',  ( -75.72275237452288366, -275.4646790912669871, -205.2144843793558948 ) ) ;
#50388 = VERTEX_POINT ( 'NONE', #84539 ) ;
#50389 = EDGE_CURVE ( 'NONE', #57506, #84890, #49804, .T. ) ;
#50390 = CARTESIAN_POINT ( 'NONE',  ( -112.1168617958987568, -277.8323660846900225, -288.5326667410064942 ) ) ;
#50391 = CARTESIAN_POINT ( 'NONE',  ( 35.49336973230709447, -274.1112568995672518, -282.5644690008441557 ) ) ;
#50392 = CARTESIAN_POINT ( 'NONE',  ( -37.84053400009924673, -299.2508443843946111, -196.9657388980841404 ) ) ;
#50393 = CARTESIAN_POINT ( 'NONE',  ( 33.12752987348345357, -276.7566769568019822, -290.3443410881425280 ) ) ;
#50394 = CARTESIAN_POINT ( 'NONE',  ( 36.64306673344027132, -277.0920454183344646, -252.9774930820295538 ) ) ;
#50395 = CARTESIAN_POINT ( 'NONE',  ( -26.04203593737108591, -274.9290531893300340, -344.8643017382003109 ) ) ;
#50396 = CARTESIAN_POINT ( 'NONE',  ( -15.55454980169585788, -295.4141749147962059, -340.1941099898121479 ) ) ;
#50397 = CARTESIAN_POINT ( 'NONE',  ( -4.086493197662068866, -293.1795092828187421, -336.0217518665535295 ) ) ;
#50398 = PLANE ( 'NONE',  #19994 ) ;
#50399 = CARTESIAN_POINT ( 'NONE',  ( -113.6568941996796269, -279.1719006691246250, -260.1822273235796388 ) ) ;
#50400 = CARTESIAN_POINT ( 'NONE',  ( -36.46404459810915455, -277.2075663479450327, -343.3683091744609328 ) ) ;
#50401 = CARTESIAN_POINT ( 'NONE',  ( -3.691058235656173192, -285.1717261881592549, -201.6376383291749335 ) ) ;
#50402 = CARTESIAN_POINT ( 'NONE',  ( -100.7830366863755955, -299.0935691332473425, -230.0470355627635115 ) ) ;
#50403 = CARTESIAN_POINT ( 'NONE',  ( 82.62320746513702829, -301.5722161194245245, -196.8457140964393943 ) ) ;
#50404 = AXIS2_PLACEMENT_3D ( 'NONE', #21180, #57643, #70921 ) ;
#50405 = CARTESIAN_POINT ( 'NONE',  ( 22.08690161819221842, -287.3445316385027581, -313.0324552212792355 ) ) ;
#50406 = EDGE_CURVE ( 'NONE', #54596, #55951, #92104, .T. ) ;
#50407 = CARTESIAN_POINT ( 'NONE',  ( -79.22363092633919734, -275.8653573966271892, -331.4471224264939337 ) ) ;
#50408 = CARTESIAN_POINT ( 'NONE',  ( -78.98023517226346257, -276.2001724052498730, -331.0994277800444365 ) ) ;
#50409 = CARTESIAN_POINT ( 'NONE',  ( -20.07103143784055632, -284.8305155240813065, -343.3982667085224989 ) ) ;
#50410 = CARTESIAN_POINT ( 'NONE',  ( -48.65397875235746739, -278.4043432548106125, -342.9328708925188494 ) ) ;
#50411 = DIRECTION ( 'NONE',  ( 0.000000000000000000, 1.000000000000000000, 0.000000000000000000 ) ) ;
#50412 = AXIS2_PLACEMENT_3D ( 'NONE', #26182, #47948, #19548 ) ;
#50413 = CARTESIAN_POINT ( 'NONE',  ( 30.54688990539132476, -273.5016753868712840, -235.7550526658807541 ) ) ;
#50414 = CIRCLE ( 'NONE', #27718, 35.00000000000000000 ) ;
#50415 = CARTESIAN_POINT ( 'NONE',  ( 25.35899675022165667, -275.6861437755006818, -232.6796445339590775 ) ) ;
#50416 = CARTESIAN_POINT ( 'NONE',  ( 29.45978265135702401, -284.0073380408512094, -304.8225503676121662 ) ) ;
#50417 = CARTESIAN_POINT ( 'NONE',  ( 123.4306832106270946, -134.2641364535880939, 0.000000000000000000 ) ) ;
#50418 = CARTESIAN_POINT ( 'NONE',  ( 0.02878841654864764885, -290.4793893536851783, -336.0918662167628099 ) ) ;
#50419 = CIRCLE ( 'NONE', #33794, 1.500000000000003997 ) ;
#50420 = CARTESIAN_POINT ( 'NONE',  ( 29.79767475420488054, -291.1094346075341832, -236.8199325610007691 ) ) ;
#50421 = CARTESIAN_POINT ( 'NONE',  ( 169.8384340989974817, 250.5000000000000568, -24.41176470588234437 ) ) ;
#50422 = CARTESIAN_POINT ( 'NONE',  ( -110.8348508120440101, -271.2371897950222888, -270.3444116073703185 ) ) ;
#50423 = CARTESIAN_POINT ( 'NONE',  ( -4.261730838314683467, -290.6324690631940371, -203.8895927681387548 ) ) ;
#50424 = CARTESIAN_POINT ( 'NONE',  ( -108.4555765497910471, -262.4588243622614527, -317.8183916042563055 ) ) ;
#50425 = CARTESIAN_POINT ( 'NONE',  ( 156.9431851590352665, 250.0000000000000568, 17.51463615629799975 ) ) ;
#50426 = CARTESIAN_POINT ( 'NONE',  ( -62.55301335731594747, -287.8540992579118551, -342.4385068502485296 ) ) ;
#50427 = CARTESIAN_POINT ( 'NONE',  ( -68.09941197489402498, -285.0630646150916050, -337.4461653420434004 ) ) ;
#50428 = CARTESIAN_POINT ( 'NONE',  ( -87.06963639359018714, -283.6109735456283829, -212.8362216305413597 ) ) ;
#50429 = CIRCLE ( 'NONE', #21715, 6.154241149514405151 ) ;
#50430 = CARTESIAN_POINT ( 'NONE',  ( -91.16010416744582301, -285.2614126684633220, -320.5503031129671854 ) ) ;
#50431 = EDGE_CURVE ( 'NONE', #51603, #43740, #71301, .T. ) ;
#50432 = CARTESIAN_POINT ( 'NONE',  ( -110.0319674729293808, -285.2401243299765952, -279.0877432656427573 ) ) ;
#50433 = CARTESIAN_POINT ( 'NONE',  ( -61.19241030814799132, -293.7240306000317673, -198.8250346200564138 ) ) ;
#50434 = CARTESIAN_POINT ( 'NONE',  ( -64.89647830068022927, -274.0352103075979358, -198.4687159848319027 ) ) ;
#50435 = AXIS2_PLACEMENT_3D ( 'NONE', #93601, #14562, #20256 ) ;
#50436 = CARTESIAN_POINT ( 'NONE',  ( -81.07662245399937717, -289.5429708344407800, -208.7447990020838233 ) ) ;
#50437 = CARTESIAN_POINT ( 'NONE',  ( -56.92402925571688144, -277.2978082133980138, -344.8845020303465390 ) ) ;
#50438 = CARTESIAN_POINT ( 'NONE',  ( 36.84450477800405821, -295.6445062859062318, -279.0781348419051255 ) ) ;
#50439 = CARTESIAN_POINT ( 'NONE',  ( -48.18343439339133738, -268.4940904799720442, -439.4148130071538958 ) ) ;
#50440 = CARTESIAN_POINT ( 'NONE',  ( -85.33152481854864391, -293.9090924074130839, -210.2361428286349110 ) ) ;
#50441 = CARTESIAN_POINT ( 'NONE',  ( -110.8017595996040257, -283.2658667256583271, -268.1558653716044205 ) ) ;
#50442 = CARTESIAN_POINT ( 'NONE',  ( -81.05204825041448657, -277.4582436470126936, -209.4151902017766815 ) ) ;
#50443 = CARTESIAN_POINT ( 'NONE',  ( -43.96312658206134216, -272.4499059399690850, -194.2894473756018670 ) ) ;
#50444 = CARTESIAN_POINT ( 'NONE',  ( 32.16131357893130627, -274.5986080161726477, -247.5437793123001882 ) ) ;
#50445 = CARTESIAN_POINT ( 'NONE',  ( -17.26210013418049272, -293.8360477393512156, -199.4030420448374628 ) ) ;
#50446 = VECTOR ( 'NONE', #56887, 999.9999999999998863 ) ;
#50447 = CARTESIAN_POINT ( 'NONE',  ( -7.184270956131327601, -293.3990244232187479, -203.6232882716992663 ) ) ;
#50448 = CARTESIAN_POINT ( 'NONE',  ( 30.47301169727677816, -295.3272022080167858, -305.7795190125078761 ) ) ;
#50449 = CARTESIAN_POINT ( 'NONE',  ( -103.9374875671850020, -295.9812336854413388, -300.3845429058175682 ) ) ;
#50450 = CARTESIAN_POINT ( 'NONE',  ( -76.90265548686402042, -291.5822160142303119, -334.0787094229563081 ) ) ;
#50451 = CARTESIAN_POINT ( 'NONE',  ( -74.27411833339516534, -283.6955025699494968, -337.9853668908753548 ) ) ;
#50452 = CARTESIAN_POINT ( 'NONE',  ( -4.342332206735987299, -272.6220107447962846, -202.1460536848136940 ) ) ;
#50453 = CARTESIAN_POINT ( 'NONE',  ( 37.72010669771049152, -287.1701095952975606, -253.1350320327633199 ) ) ;
#50454 = CARTESIAN_POINT ( 'NONE',  ( -101.9951472667570300, -280.0305432084947483, -307.7714173920122676 ) ) ;
#50455 = CARTESIAN_POINT ( 'NONE',  ( -49.44866146962257147, -284.9528909403255739, -198.0818289740959131 ) ) ;
#50456 = CARTESIAN_POINT ( 'NONE',  ( -105.9134105031455135, -288.1525095434603827, -300.8685683642787581 ) ) ;
#50457 = CARTESIAN_POINT ( 'NONE',  ( 192.1331913634949160, 286.0196433216794389, -110.9393339982713940 ) ) ;
#50458 = CARTESIAN_POINT ( 'NONE',  ( -106.5886274555256392, -284.3709272072370027, -246.9035698887442720 ) ) ;
#50459 = CARTESIAN_POINT ( 'NONE',  ( 37.59302098626444888, -282.5565572778405112, -254.3988544766780819 ) ) ;
#50460 = CARTESIAN_POINT ( 'NONE',  ( -98.84782537177314055, -288.9977118160620648, -316.3156013001191695 ) ) ;
#50461 = CARTESIAN_POINT ( 'NONE',  ( -111.6992376003494201, -279.9417900779183128, -287.0163585937223161 ) ) ;
#50462 = CARTESIAN_POINT ( 'NONE',  ( -112.5147846417367674, -280.0472341064390776, -256.0675557195702368 ) ) ;
#50463 = CARTESIAN_POINT ( 'NONE',  ( -14.30686415809234902, -280.1925111863634470, -201.0372202223673241 ) ) ;
#50464 = CARTESIAN_POINT ( 'NONE',  ( -75.12727705376188680, -275.5263574673310245, -205.9265705689643369 ) ) ;
#50465 = CARTESIAN_POINT ( 'NONE',  ( 19.41566216221196584, -292.8442308958108811, -218.3264965671178572 ) ) ;
#50466 = CARTESIAN_POINT ( 'NONE',  ( 25.61230844166575338, -286.1146300050408513, -310.4689676739845936 ) ) ;
#50467 = CARTESIAN_POINT ( 'NONE',  ( -69.30635844397487233, -293.2387339056230076, -201.1753907227580100 ) ) ;
#50468 = CARTESIAN_POINT ( 'NONE',  ( -106.0909435701332484, -295.8121612422846738, -244.7634910073658716 ) ) ;
#50469 = CARTESIAN_POINT ( 'NONE',  ( 21.33077079710802693, -284.1055228959285728, -316.1743841523888818 ) ) ;
#50470 = CARTESIAN_POINT ( 'NONE',  ( -70.94430627564580050, -295.1750121629748946, -335.2052875502798202 ) ) ;
#50471 = CARTESIAN_POINT ( 'NONE',  ( -0.9626585369666372793, -293.6032557839350261, -202.8477278792764764 ) ) ;
#50472 = CARTESIAN_POINT ( 'NONE',  ( 35.53135705636167074, -282.2877554778768854, -276.7518076517758345 ) ) ;
#50473 = EDGE_CURVE ( 'NONE', #75506, #49742, #51852, .T. ) ;
#50474 = CARTESIAN_POINT ( 'NONE',  ( 7.776902166684397599, -297.5249256984344584, -193.6782679355795267 ) ) ;
#50475 = CARTESIAN_POINT ( 'NONE',  ( -37.49305186129453915, -289.7053735041076834, -347.2720912057832265 ) ) ;
#50476 = CARTESIAN_POINT ( 'NONE',  ( -100.4044040935508662, -282.1289812152826357, -312.4481629479118965 ) ) ;
#50477 = CARTESIAN_POINT ( 'NONE',  ( -95.43955505201894596, -290.2026216236845357, -320.8624401911598056 ) ) ;
#50478 = CARTESIAN_POINT ( 'NONE',  ( 20.35475171295237828, -287.2552037600265749, -225.6039182061704764 ) ) ;
#50479 = DIRECTION ( 'NONE',  ( 0.9951408606192334583, 1.205805641958521361E-17, 0.09846150276129006507 ) ) ;
#50480 = AXIS2_PLACEMENT_3D ( 'NONE', #37678, #73689, #15934 ) ;
#50481 = CARTESIAN_POINT ( 'NONE',  ( 151.9477299421133125, 206.7868891706451109, -215.8238548150086160 ) ) ;
#50482 = CARTESIAN_POINT ( 'NONE',  ( 5.705534526590854583, -59.28686408112852035, -350.9003461107548105 ) ) ;
#50483 = CARTESIAN_POINT ( 'NONE',  ( -100.7278341873435323, -277.2482665041739551, -306.9978013252224400 ) ) ;
#50484 = CARTESIAN_POINT ( 'NONE',  ( -64.91970509698334979, -278.6035530277573571, -202.4370448132260663 ) ) ;
#50485 = CARTESIAN_POINT ( 'NONE',  ( 24.46543051742215269, -274.6085872508367629, -224.4740512538465111 ) ) ;
#50486 = CARTESIAN_POINT ( 'NONE',  ( -101.2518121434645622, -256.0555729666142497, -325.2581032958395895 ) ) ;
#50487 = CARTESIAN_POINT ( 'NONE',  ( -53.61713600356608822, -278.4221417151254059, -195.6496420831716136 ) ) ;
#50489 = CARTESIAN_POINT ( 'NONE',  ( -32.05378935133700935, -281.0052107264659185, -344.8183862846131547 ) ) ;
#50488 = AXIS2_PLACEMENT_3D ( 'NONE', #64905, #50666, #27481 ) ;
#50490 = CARTESIAN_POINT ( 'NONE',  ( -113.3519438283958038, -298.2856382529115535, -272.4644083437675022 ) ) ;
#50491 = PRODUCT_DEFINITION_SHAPE ( 'NONE', 'NONE',  #93719 ) ;
#50492 = CARTESIAN_POINT ( 'NONE',  ( -102.4672627273991310, -291.4952201178479640, -237.1334079464599824 ) ) ;
#50493 = CARTESIAN_POINT ( 'NONE',  ( -90.96396670529055939, -288.5179594598225208, -320.6937476754358158 ) ) ;
#50494 = CARTESIAN_POINT ( 'NONE',  ( 38.39027062501985199, -276.0355525575665183, -256.9449555593651553 ) ) ;
#50495 = CARTESIAN_POINT ( 'NONE',  ( -106.3063850458897832, -272.8704651711901192, -246.4263684708686810 ) ) ;
#50496 = ORIENTED_EDGE ( 'NONE', *, *, #70607, .T. ) ;
#50497 = DIRECTION ( 'NONE',  ( 0.000000000000000000, 0.000000000000000000, 1.000000000000000000 ) ) ;
#50498 = DIRECTION ( 'NONE',  ( -1.000000000000000000, 0.000000000000000000, 0.000000000000000000 ) ) ;
#50499 = TOROIDAL_SURFACE ( 'NONE', #9658, 1.500000000000000000, 0.5000000000000000000 ) ;
#50500 = AXIS2_PLACEMENT_3D ( 'NONE', #7846, #65189, #14968 ) ;
#50501 = CARTESIAN_POINT ( 'NONE',  ( -81.41904606568036229, -281.3779270763285467, -208.9892859210765153 ) ) ;
#50502 = CIRCLE ( 'NONE', #85308, 24.99999999999999645 ) ;
#50503 = CARTESIAN_POINT ( 'NONE',  ( 21.56920778077186895, -282.0223799252533468, -226.7082292495792899 ) ) ;
#50504 = CARTESIAN_POINT ( 'NONE',  ( 22.06881807706979259, -282.6693004940840979, -222.9657175083636957 ) ) ;
#50505 = CARTESIAN_POINT ( 'NONE',  ( -96.11772671889373498, -283.0000627802093618, -314.0507866341251884 ) ) ;
#50506 = CARTESIAN_POINT ( 'NONE',  ( -111.1975082463037836, -280.5162199175214823, -262.3712252633940807 ) ) ;
#50507 = CARTESIAN_POINT ( 'NONE',  ( -81.47085739290587014, -271.9196980618636985, -211.2773968101878950 ) ) ;
#50508 = FACE_OUTER_BOUND ( 'NONE', #10011, .T. ) ;
#50509 = CARTESIAN_POINT ( 'NONE',  ( 169.7306087885279453, 275.5000000000000568, -24.89999999999999147 ) ) ;
#50510 = CARTESIAN_POINT ( 'NONE',  ( -113.1381988192177630, -279.1969261138105480, -282.9726050801349402 ) ) ;
#50511 = AXIS2_PLACEMENT_3D ( 'NONE', #53831, #89791, #69904 ) ;
#50512 = CARTESIAN_POINT ( 'NONE',  ( 193.9402003287077605, 250.0000000000000568, 16.58062614384823874 ) ) ;
#50513 = CARTESIAN_POINT ( 'NONE',  ( -23.06691515001490345, -275.4478672871723575, -345.4804364020085359 ) ) ;
#50514 = ORIENTED_EDGE ( 'NONE', *, *, #65811, .F. ) ;
#50515 = LINE ( 'NONE', #79413, #38357 ) ;
#50516 = CARTESIAN_POINT ( 'NONE',  ( -100.0363718466172713, -285.9686698797094095, -312.2612172582324206 ) ) ;
#50517 = CARTESIAN_POINT ( 'NONE',  ( 33.26986962350301269, -293.0022542990965917, -289.5557344872793806 ) ) ;
#50518 = CARTESIAN_POINT ( 'NONE',  ( 22.32079750397118900, -287.5527026076826473, -318.8967759123659107 ) ) ;
#50519 = CARTESIAN_POINT ( 'NONE',  ( -109.9182901622778701, -282.9808317574454009, -255.8486201017754524 ) ) ;
#50521 = CARTESIAN_POINT ( 'NONE',  ( -75.25395888720483129, -287.8047391010647402, -333.9419976261119700 ) ) ;
#50520 = CARTESIAN_POINT ( 'NONE',  ( -110.0000325931605687, -283.2806057418363821, -258.6134457570994982 ) ) ;
#50522 = CARTESIAN_POINT ( 'NONE',  ( -32.10212280684519470, -284.1896645540531381, -343.5709351837858776 ) ) ;
#50523 = CARTESIAN_POINT ( 'NONE',  ( 18.56257173616869949, -272.8551857237717400, -220.2876351543102658 ) ) ;
#50524 = CARTESIAN_POINT ( 'NONE',  ( -100.3236513827977632, -283.5246852950218113, -227.3760539709128352 ) ) ;
#50525 = CARTESIAN_POINT ( 'NONE',  ( -52.85015154766669809, -297.2509308176731224, -343.7933149615362822 ) ) ;
#50526 = CARTESIAN_POINT ( 'NONE',  ( -51.79520111552989192, -283.8676133546560436, -196.5440465423693581 ) ) ;
#50527 = CARTESIAN_POINT ( 'NONE',  ( -76.95918794734335222, -280.4487369461126036, -208.7063157858078739 ) ) ;
#50528 = CARTESIAN_POINT ( 'NONE',  ( -1.858048916852585331, -288.5212814252029716, -204.0969577940154807 ) ) ;
#50529 = CARTESIAN_POINT ( 'NONE',  ( 195.7521072783280545, 26.33975396946494385, 13.62141033231749887 ) ) ;
#50530 = DIRECTION ( 'NONE',  ( 0.000000000000000000, 0.000000000000000000, -1.000000000000000000 ) ) ;
#50531 = CARTESIAN_POINT ( 'NONE',  ( 36.01790000063211039, -295.2415303477548605, -252.2590940450626249 ) ) ;
#50532 = CARTESIAN_POINT ( 'NONE',  ( -106.1152682234376385, -276.1589251797670386, -300.4111981247043559 ) ) ;
#50533 = CARTESIAN_POINT ( 'NONE',  ( -107.1095149875896482, -290.1634929540900885, -238.0379447303488121 ) ) ;
#50534 = CARTESIAN_POINT ( 'NONE',  ( -71.31703719393351548, -293.9083698143986680, -335.8895066952438810 ) ) ;
#50535 = CARTESIAN_POINT ( 'NONE',  ( -98.39400186341818255, -277.8025112392520555, -229.3579486722650245 ) ) ;
#50536 = CARTESIAN_POINT ( 'NONE',  ( -111.3140475351107455, -270.7397676659972490, -262.0300906769599010 ) ) ;
#50537 = CARTESIAN_POINT ( 'NONE',  ( -32.13897964363114568, -293.4342942713402635, -197.0396463758820573 ) ) ;
#50538 = CARTESIAN_POINT ( 'NONE',  ( -112.3417001280813849, -275.0519495502701943, -270.3929463913730729 ) ) ;
#50539 = CARTESIAN_POINT ( 'NONE',  ( 17.05359745089726076, -292.7741437696052458, -323.9512907131414750 ) ) ;
#50540 = CARTESIAN_POINT ( 'NONE',  ( -87.25561993988239351, -291.3615362500224251, -324.7907146433126968 ) ) ;
#50541 = CARTESIAN_POINT ( 'NONE',  ( -27.95178620049705742, -290.4095214165646439, -194.9038811779794855 ) ) ;
#50542 = CARTESIAN_POINT ( 'NONE',  ( -70.21951838705865612, -290.9194136976122422, -336.2114292482568203 ) ) ;
#50543 = EDGE_CURVE ( 'NONE', #74935, #9133, #15070, .T. ) ;
#50544 = DIRECTION ( 'NONE',  ( 0.5831039236546639026, -0.7661730729848326149, -0.2701270746362063879 ) ) ;
#50545 = CARTESIAN_POINT ( 'NONE',  ( -50.77109552316714769, -290.0308122029234141, -342.3312875913430844 ) ) ;
#50546 = CARTESIAN_POINT ( 'NONE',  ( -47.80257052418233599, -229.5268262511776527, 22.50000000000000000 ) ) ;
#50547 = CARTESIAN_POINT ( 'NONE',  ( -8.369016963255182517, -289.8862558127065654, -341.2878803557987339 ) ) ;
#50548 = CARTESIAN_POINT ( 'NONE',  ( 25.33943359759332736, -280.1348659051067784, -312.1879308853149837 ) ) ;
#50549 = CARTESIAN_POINT ( 'NONE',  ( -53.76010863433338471, -280.1804122124978562, -195.0989829989659654 ) ) ;
#50550 = CARTESIAN_POINT ( 'NONE',  ( 38.64628956567906215, -281.3739149592637432, -282.7547952723463709 ) ) ;
#50551 = CARTESIAN_POINT ( 'NONE',  ( 36.93770649846224785, -285.6863584785522789, -280.8260127570521263 ) ) ;
#50552 = CARTESIAN_POINT ( 'NONE',  ( 209.3315607876652109, 29.46185999635553898, 14.69807322781335301 ) ) ;
#50553 = CARTESIAN_POINT ( 'NONE',  ( 10.69016339196880061, -280.5200760759428249, -327.0308687734026876 ) ) ;
#50554 = CARTESIAN_POINT ( 'NONE',  ( -111.6223074729752938, -282.4142092783552584, -281.0918381816071019 ) ) ;
#50555 = CARTESIAN_POINT ( 'NONE',  ( 168.7561003588637334, 230.7615523021927686, -190.5427080440589407 ) ) ;
#50556 = CARTESIAN_POINT ( 'NONE',  ( -107.8644361924002766, -277.4057979433205219, -241.2191988774684432 ) ) ;
#50557 = CIRCLE ( 'NONE', #9720, 154.4364916446740210 ) ;
#50558 = CARTESIAN_POINT ( 'NONE',  ( -108.7356630204407537, -283.8305709983785619, -242.2097183485544747 ) ) ;
#50559 = CARTESIAN_POINT ( 'NONE',  ( -97.98275434827525032, -273.9237005488904515, -229.3407278936872444 ) ) ;
#50560 = PLANE ( 'NONE',  #1955 ) ;
#50561 = CARTESIAN_POINT ( 'NONE',  ( -34.85046563102983441, -293.6840978692334261, -196.6031749020170025 ) ) ;
#50562 = CARTESIAN_POINT ( 'NONE',  ( -34.14614178834995784, -275.5168702564121190, -194.0171941846750769 ) ) ;
#50563 = CARTESIAN_POINT ( 'NONE',  ( 34.18441814380773280, -275.4127365300766428, -285.0615224604768514 ) ) ;
#50564 = CARTESIAN_POINT ( 'NONE',  ( -93.67655316886165906, -297.8643277003683352, -319.8725811360475291 ) ) ;
#50565 = CARTESIAN_POINT ( 'NONE',  ( -23.30985349296062736, -289.0443066083440726, -346.1259142551897412 ) ) ;
#50566 = CARTESIAN_POINT ( 'NONE',  ( 29.78643164495066742, -280.0876544692137600, -305.0472552696973025 ) ) ;
#50567 = AXIS2_PLACEMENT_3D ( 'NONE', #72969, #9011, #65897 ) ;
#50568 = CARTESIAN_POINT ( 'NONE',  ( 32.18687852758876744, -292.9599644061058257, -237.1497882578106555 ) ) ;
#50569 = CARTESIAN_POINT ( 'NONE',  ( -67.88844043238822223, -290.6998108127315845, -203.7868035206649324 ) ) ;
#50570 = CARTESIAN_POINT ( 'NONE',  ( -60.98585703193001706, -293.3587371765879084, -341.5909353593992250 ) ) ;
#50571 = ORIENTED_EDGE ( 'NONE', *, *, #39491, .F. ) ;
#50572 = FACE_OUTER_BOUND ( 'NONE', #87584, .T. ) ;
#50573 = AXIS2_PLACEMENT_3D ( 'NONE', #90297, #55284, #84138 ) ;
#50574 = CARTESIAN_POINT ( 'NONE',  ( -64.08830546451953580, -291.2012709614912183, -202.3578134652283325 ) ) ;
#50575 = CARTESIAN_POINT ( 'NONE',  ( -22.78264641048746597, -118.9815703160634541, 21.50000000000000000 ) ) ;
#50576 = CARTESIAN_POINT ( 'NONE',  ( 25.34601139933747760, -287.9050087200863572, -226.0319019468360295 ) ) ;
#50577 = CARTESIAN_POINT ( 'NONE',  ( -107.3381139276884824, -270.1608578419545665, -262.4421837807431075 ) ) ;
#50578 = CARTESIAN_POINT ( 'NONE',  ( -37.69994709945558498, -294.1152526399672524, -347.1380271246727034 ) ) ;
#50579 = CARTESIAN_POINT ( 'NONE',  ( -66.37350456906163743, -284.7395711543567245, -341.1597620802547794 ) ) ;
#50580 = CARTESIAN_POINT ( 'NONE',  ( -108.0281295831141222, -284.6261586026583927, -252.1284907602799876 ) ) ;
#50581 = CARTESIAN_POINT ( 'NONE',  ( 32.76367154741866727, -277.3707948775800674, -293.0755322310818087 ) ) ;
#50582 = CARTESIAN_POINT ( 'NONE',  ( -3.615561839231120178, -292.6249790993928173, -336.9666782701792727 ) ) ;
#50583 = CARTESIAN_POINT ( 'NONE',  ( -35.60466796355051144, -296.7902389358005735, -344.3667378590021144 ) ) ;
#50584 = AXIS2_PLACEMENT_3D ( 'NONE', #49757, #64006, #14733 ) ;
#50585 = CARTESIAN_POINT ( 'NONE',  ( 30.64003728721610642, -274.7173237397886965, -298.1660121536711472 ) ) ;
#50586 = EDGE_LOOP ( 'NONE', ( #76468, #56283 ) ) ;
#50587 = CARTESIAN_POINT ( 'NONE',  ( 175.2296996224750103, 247.0000000000001137, 0.000000000000000000 ) ) ;
#50588 = CARTESIAN_POINT ( 'NONE',  ( 37.76235922683074619, -293.4308532070033948, -287.3062319609697397 ) ) ;
#50589 = CARTESIAN_POINT ( 'NONE',  ( 37.12011636808607307, -289.4449720439729390, -268.2476503550930715 ) ) ;
#50590 = CARTESIAN_POINT ( 'NONE',  ( 200.9868139007817263, 294.2258809633341343, -54.00000000000627409 ) ) ;
#50591 = CARTESIAN_POINT ( 'NONE',  ( 75.80595655901278462, -300.5172811257933176, -193.6499684678605036 ) ) ;
#50592 = CARTESIAN_POINT ( 'NONE',  ( -57.43035015493347828, -286.4374757898834218, -200.0208854630392068 ) ) ;
#50593 = ORIENTED_EDGE ( 'NONE', *, *, #34052, .T. ) ;
#50594 = CARTESIAN_POINT ( 'NONE',  ( -61.96078719651509203, -278.7986436637582983, -197.5952210541718728 ) ) ;
#50595 = CARTESIAN_POINT ( 'NONE',  ( -53.26003357299727980, -295.9024005646747923, -345.6480237536758864 ) ) ;
#50596 = CARTESIAN_POINT ( 'NONE',  ( -51.47843674278839643, -287.3706754109274470, -344.7953718971581338 ) ) ;
#50597 = B_SPLINE_CURVE_WITH_KNOTS ( 'NONE', 3,
 ( #8011, #6171, #21301, #36904, #22681, #64896 ),
 .UNSPECIFIED., .F., .F.,
 ( 4, 2, 4 ),
 ( 1.734723475976807094E-18, 0.0006612700175534703311, 0.001322540035106938927 ),
 .UNSPECIFIED. ) ;
#50598 = CARTESIAN_POINT ( 'NONE',  ( -94.63300086554374957, -296.1874574772651272, -321.7952590677210765 ) ) ;
#50599 = CARTESIAN_POINT ( 'NONE',  ( 6.685613656262284543, -293.0032402247386472, -212.1057909504669112 ) ) ;
#50600 = CARTESIAN_POINT ( 'NONE',  ( 129.4467878515196162, -299.5541904835127980, -195.3611179825600175 ) ) ;
#50601 = PLANE ( 'NONE',  #40199 ) ;
#50602 = CARTESIAN_POINT ( 'NONE',  ( 139.6925840978351232, -135.2391364535880882, 21.50000000000000000 ) ) ;
#50603 = CARTESIAN_POINT ( 'NONE',  ( -30.96129520394098478, -287.6514862100369783, -194.3084914561176504 ) ) ;
#50604 = CARTESIAN_POINT ( 'NONE',  ( -2.659677404128736544, -292.1237833571632336, -342.4524372437778652 ) ) ;
#50605 = ORIENTED_EDGE ( 'NONE', *, *, #52172, .F. ) ;
#50606 = EDGE_CURVE ( 'NONE', #20929, #1176, #75489, .T. ) ;
#50607 = CARTESIAN_POINT ( 'NONE',  ( -28.22883870408087503, -279.5133601797209053, -193.9513684470461783 ) ) ;
#50608 = CARTESIAN_POINT ( 'NONE',  ( -29.22100949224067179, -284.9493176896522186, -344.8043067740237575 ) ) ;
#50609 = EDGE_CURVE ( 'NONE', #47563, #64125, #58833, .T. ) ;
#50610 = CARTESIAN_POINT ( 'NONE',  ( -91.47267292630989743, -283.8744249994660436, -216.4311256210886540 ) ) ;
#50611 = CARTESIAN_POINT ( 'NONE',  ( 11.03284419091577995, -286.4567719829759653, -327.0085594551189274 ) ) ;
#50612 = CARTESIAN_POINT ( 'NONE',  ( 35.70122412836058601, -277.6693433025096169, -290.5350726345512840 ) ) ;
#50613 = CARTESIAN_POINT ( 'NONE',  ( -102.5901131178605681, -297.4916430258418814, -237.3754689325374443 ) ) ;
#50614 = VERTEX_POINT ( 'NONE', #52629 ) ;
#50615 = CARTESIAN_POINT ( 'NONE',  ( 33.58828221144553794, -292.4899956675226917, -289.6490160998978354 ) ) ;
#50617 = CARTESIAN_POINT ( 'NONE',  ( -99.55011862251508603, -278.4305625841293477, -231.8717899216632929 ) ) ;
#50616 = CARTESIAN_POINT ( 'NONE',  ( -100.8118069179065799, -279.0460627205999913, -234.2980406861314009 ) ) ;
#50618 = CARTESIAN_POINT ( 'NONE',  ( -36.95515232414381046, -275.1365832126898567, -193.6582033488697050 ) ) ;
#50619 = CARTESIAN_POINT ( 'NONE',  ( -112.4076225778830889, -277.1543271996079625, -285.6941421875354763 ) ) ;
#50620 = CARTESIAN_POINT ( 'NONE',  ( 200.9738562182569694, 294.2969822784109510, -54.00000000000292744 ) ) ;
#50621 = CARTESIAN_POINT ( 'NONE',  ( -98.63077282400308832, -298.5892371604248865, -224.7075320890699572 ) ) ;
#50622 = DIRECTION ( 'NONE',  ( 0.000000000000000000, 0.000000000000000000, 1.000000000000000000 ) ) ;
#50623 = ORIENTED_EDGE ( 'NONE', *, *, #44755, .T. ) ;
#50624 = FACE_OUTER_BOUND ( 'NONE', #6109, .T. ) ;
#50625 = CARTESIAN_POINT ( 'NONE',  ( -4.468222450009211144, -287.5756352958367756, -204.8358515586194812 ) ) ;
#50626 = CARTESIAN_POINT ( 'NONE',  ( -36.59816230708373297, -287.8214984955697560, -194.3652189482223491 ) ) ;
#50627 = CARTESIAN_POINT ( 'NONE',  ( 32.40837719230589897, -287.1923481898029422, -292.4114728223817679 ) ) ;
#50628 = CARTESIAN_POINT ( 'NONE',  ( -112.1607808670383690, -283.8346397242334547, -288.3510100265839924 ) ) ;
#50629 = CARTESIAN_POINT ( 'NONE',  ( -108.7414440732028851, -277.1964146775194422, -251.6429237998689814 ) ) ;
#50630 = CARTESIAN_POINT ( 'NONE',  ( -103.3473028478311448, -286.8666932402496741, -236.3886896451549546 ) ) ;
#50631 = CARTESIAN_POINT ( 'NONE',  ( 22.36239618090853654, -280.6309400931646110, -313.5814276142867243 ) ) ;
#50632 = CARTESIAN_POINT ( 'NONE',  ( -35.08583151312780046, -278.3384105242751616, -343.8196405377458404 ) ) ;
#50633 = CARTESIAN_POINT ( 'NONE',  ( 19.89980603403492054, -275.4039490821534173, -224.9384763172944020 ) ) ;
#50634 = CARTESIAN_POINT ( 'NONE',  ( -12.36775838504746261, -287.5294454251916818, -342.8343117162604017 ) ) ;
#50635 = CARTESIAN_POINT ( 'NONE',  ( -92.31106530986541259, -284.6169264535692491, -324.0502948419393192 ) ) ;
#50636 = CARTESIAN_POINT ( 'NONE',  ( 36.42148273580804840, -282.3212365474557828, -292.4195444758761369 ) ) ;
#50637 = ORIENTED_EDGE ( 'NONE', *, *, #80735, .T. ) ;
#50638 = ORIENTED_EDGE ( 'NONE', *, *, #59261, .T. ) ;
#50639 = CARTESIAN_POINT ( 'NONE',  ( 156.6297654408069491, 214.9642006536927852, 17.09991073265227968 ) ) ;
#50640 = CARTESIAN_POINT ( 'NONE',  ( -73.81161595310983614, -291.3914379336896445, -336.7856464069825506 ) ) ;
#50641 = CARTESIAN_POINT ( 'NONE',  ( -112.6508663995820996, -289.0663228429464198, -283.9195570222651668 ) ) ;
#50642 = AXIS2_PLACEMENT_3D ( 'NONE', #30819, #15675, #45454 ) ;
#50643 = CARTESIAN_POINT ( 'NONE',  ( -83.32906147637478966, -272.4625435929074797, -213.3648808822834440 ) ) ;
#50644 = CARTESIAN_POINT ( 'NONE',  ( 30.81243232566732715, -292.4393703750646409, -234.6328833485093242 ) ) ;
#50645 = CARTESIAN_POINT ( 'NONE',  ( -106.6915217162919021, -288.7031856193524959, -295.2872086778048129 ) ) ;
#50647 = EDGE_CURVE ( 'NONE', #36421, #71850, #19789, .T. ) ;
#50646 = CARTESIAN_POINT ( 'NONE',  ( 5.102856127595141622, -290.8742407376810206, -209.6646775858870626 ) ) ;
#50648 = CARTESIAN_POINT ( 'NONE',  ( 34.40205780873399277, -288.9611997452870469, -285.9108841845203415 ) ) ;
#50649 = CARTESIAN_POINT ( 'NONE',  ( -37.37352853689063892, -294.5519495502701943, -195.3611179825600175 ) ) ;
#50650 = CARTESIAN_POINT ( 'NONE',  ( 34.47777196055003657, -289.8312778949887161, -292.0151259681339297 ) ) ;
#50651 = CARTESIAN_POINT ( 'NONE',  ( -109.0409849057111842, -288.2595304861441718, -293.0977176048550632 ) ) ;
#50652 = CARTESIAN_POINT ( 'NONE',  ( -20.80378870078060771, -294.2644622551550810, -197.1545517989554526 ) ) ;
#50653 = CARTESIAN_POINT ( 'NONE',  ( -108.6516683530374081, -285.2733919744090940, -287.0981029724775340 ) ) ;
#50654 = CARTESIAN_POINT ( 'NONE',  ( -14.44962477803068879, -294.3482656831655504, -198.7105233637303741 ) ) ;
#50655 = DIRECTION ( 'NONE',  ( 0.8435586647355846068, 0.000000000000000000, -0.5370370370370349811 ) ) ;
#50656 = LINE ( 'NONE', #29809, #57920 ) ;
#50657 = CARTESIAN_POINT ( 'NONE',  ( -77.97628912913027932, -275.4888363911822466, -206.9006028719965968 ) ) ;
#50658 = AXIS2_PLACEMENT_3D ( 'NONE', #81419, #16569, #8527 ) ;
#50659 = CARTESIAN_POINT ( 'NONE',  ( 21.93678298466754484, -281.3481135854267450, -313.2621999167705553 ) ) ;
#50660 = CARTESIAN_POINT ( 'NONE',  ( -62.22157222968028378, -281.3754123324009129, -341.1688601846573761 ) ) ;
#50661 = CARTESIAN_POINT ( 'NONE',  ( -98.15294642187133434, -295.1210667941875272, -317.3308012409939920 ) ) ;
#50662 = CARTESIAN_POINT ( 'NONE',  ( -62.35131544482404564, -271.9621581253859404, -200.7012790894118837 ) ) ;
#50663 = CARTESIAN_POINT ( 'NONE',  ( -110.1787384329058881, -276.4332307719452615, -285.7260147363729743 ) ) ;
#50664 = CARTESIAN_POINT ( 'NONE',  ( -110.5431099916445419, -297.9602667386751591, -263.2686088970505125 ) ) ;
#50665 = CARTESIAN_POINT ( 'NONE',  ( 12.76929281322739840, -295.7621540178243436, -324.3221933111759654 ) ) ;
#50666 = DIRECTION ( 'NONE',  ( 0.000000000000000000, 1.000000000000000000, 0.000000000000000000 ) ) ;
#50667 = CARTESIAN_POINT ( 'NONE',  ( 18.10147307412642448, -295.0334770871054957, -318.1154958204226659 ) ) ;
#50668 = DIRECTION ( 'NONE',  ( -0.3024135303179465439, -0.9531768234071978929, 0.000000000000000000 ) ) ;
#50670 = CARTESIAN_POINT ( 'NONE',  ( -82.35981002355005387, -295.6861283191742586, -327.8918156675024420 ) ) ;
#50669 = CARTESIAN_POINT ( 'NONE',  ( -21.30880671319026476, -284.2769166707300883, -196.7312794081399545 ) ) ;
#50671 = CARTESIAN_POINT ( 'NONE',  ( -97.58040072872390169, -285.1942720901694202, -222.3996860820615780 ) ) ;
#50672 = CARTESIAN_POINT ( 'NONE',  ( 31.66658393045714703, -287.6587045706564822, -304.5929185477433521 ) ) ;
#50673 = CARTESIAN_POINT ( 'NONE',  ( 10.02857173849627159, -290.7060881060497763, -212.3621536886592196 ) ) ;
#50674 = CARTESIAN_POINT ( 'NONE',  ( -84.45983355236950274, -278.6195861815552917, -209.5974960875428508 ) ) ;
#50675 = CARTESIAN_POINT ( 'NONE',  ( -69.91165696735023971, -280.9809262143061233, -337.9199732462171255 ) ) ;
#50676 = DIRECTION ( 'NONE',  ( -1.000000000000000000, 0.000000000000000000, 0.000000000000000000 ) ) ;
#50677 = CARTESIAN_POINT ( 'NONE',  ( 36.07798791811234906, -286.3202451397177697, -268.3166277008521092 ) ) ;
#50679 = CARTESIAN_POINT ( 'NONE',  ( 197.5223219362740963, 69.56630120087481828, -11.61486628297207524 ) ) ;
#50678 = CARTESIAN_POINT ( 'NONE',  ( -74.29050612810728182, -288.4518254657351690, -337.5793730325070783 ) ) ;
#50680 = LINE ( 'NONE', #30759, #82383 ) ;
#50681 = CARTESIAN_POINT ( 'NONE',  ( -103.4761154527324152, -297.7117424962871723, -303.2283240874078274 ) ) ;
#50682 = CARTESIAN_POINT ( 'NONE',  ( 30.19247539282088155, -282.5109778659253834, -234.5028554381205481 ) ) ;
#50684 = CARTESIAN_POINT ( 'NONE',  ( 34.25056937097342313, -281.4092718712283272, -284.7988101712308548 ) ) ;
#50683 = CARTESIAN_POINT ( 'NONE',  ( -94.31070658806939377, -295.2538411404576664, -220.9584413619001566 ) ) ;
#50685 = CARTESIAN_POINT ( 'NONE',  ( 11.19995734515881658, -294.5679551348339373, -330.2019603090411124 ) ) ;
#50686 = CARTESIAN_POINT ( 'NONE',  ( 19.22528429898121516, -284.9398263185986480, -220.1890358981652298 ) ) ;
#50687 = CARTESIAN_POINT ( 'NONE',  ( -40.93863963214825219, -282.0070757780899271, -195.4345638159099678 ) ) ;
#50688 = CARTESIAN_POINT ( 'NONE',  ( -110.6197293275990745, -295.5965144270879250, -271.4547072078576093 ) ) ;
#50689 = ORIENTED_EDGE ( 'NONE', *, *, #37043, .T. ) ;
#50690 = DIRECTION ( 'NONE',  ( 0.4995866236608238475, 0.04065491159389757192, -0.8653094149623422604 ) ) ;
#50691 = CARTESIAN_POINT ( 'NONE',  ( 6.579800234881638232, -284.4316580313373493, -330.7163050484019209 ) ) ;
#50692 = DIRECTION ( 'NONE',  ( 0.000000000000000000, 0.000000000000000000, 1.000000000000000000 ) ) ;
#50693 = CARTESIAN_POINT ( 'NONE',  ( -69.91165696735023971, -292.9809262143061801, -337.9199732462171255 ) ) ;
#50694 = CARTESIAN_POINT ( 'NONE',  ( 35.90560846230874859, -275.0417417524660095, -293.5772891723465818 ) ) ;
#50695 = CARTESIAN_POINT ( 'NONE',  ( -2.437568201589315198, -292.3608657699249420, -206.2321693465572139 ) ) ;
#50696 = CARTESIAN_POINT ( 'NONE',  ( 28.39116024668721749, -282.6228366929426556, -236.9328830591988151 ) ) ;
#50697 = CARTESIAN_POINT ( 'NONE',  ( 12.06716573470712461, -276.3526501189858777, -215.4725813228913580 ) ) ;
#50698 = CARTESIAN_POINT ( 'NONE',  ( -70.10745526814440609, -285.0766877169907616, -339.1711087785158725 ) ) ;
#50699 = CARTESIAN_POINT ( 'NONE',  ( 27.19694827246567925, -280.8214523779101910, -305.3167093293772041 ) ) ;
#50700 = CARTESIAN_POINT ( 'NONE',  ( -103.6125706703960105, -280.0867013966838499, -305.4776719624892394 ) ) ;
#50701 = CARTESIAN_POINT ( 'NONE',  ( -31.90953307493142432, -298.1184045043421520, -193.3611177971762629 ) ) ;
#50702 = CARTESIAN_POINT ( 'NONE',  ( 39.70736890770487548, -275.3956356849034819, -271.1737616800800197 ) ) ;
#50703 = CARTESIAN_POINT ( 'NONE',  ( 35.18383762991108910, -295.6899563490876517, -287.1911619270002802 ) ) ;
#50704 = CARTESIAN_POINT ( 'NONE',  ( 0.000000000000000000, -142.7221692137691775, 0.000000000000000000 ) ) ;
#50705 = DIRECTION ( 'NONE',  ( 0.000000000000000000, 0.000000000000000000, 1.000000000000000000 ) ) ;
#50706 = CARTESIAN_POINT ( 'NONE',  ( 18.60137137966103893, -292.3984765948715676, -321.5323030299247762 ) ) ;
#50707 = CARTESIAN_POINT ( 'NONE',  ( -8.941124562624166217, -273.9414469537405807, -202.9915158831300630 ) ) ;
#50708 = PRODUCT_DEFINITION_FORMATION_WITH_SPECIFIED_SOURCE ( 'ANY', '', #1958, .NOT_KNOWN. ) ;
#50709 = CARTESIAN_POINT ( 'NONE',  ( -61.48770697605829127, -293.2643344410296322, -197.9198407806392197 ) ) ;
#50711 = CARTESIAN_POINT ( 'NONE',  ( -6.063184400527456219, -293.6592104890349901, -200.4207782973604992 ) ) ;
#50710 = CARTESIAN_POINT ( 'NONE',  ( -37.30987171927208124, -285.5519495502701943, -345.3611179825600175 ) ) ;
#50712 = ADVANCED_FACE ( 'NONE', ( #8616 ), #15270, .F. ) ;
#50713 = CARTESIAN_POINT ( 'NONE',  ( -64.46213936458900662, -291.4069716188662369, -340.1626961888671303 ) ) ;
#50714 = CARTESIAN_POINT ( 'NONE',  ( -106.9830185894094967, -276.1947112019400379, -297.7493487986541254 ) ) ;
#50715 = CARTESIAN_POINT ( 'NONE',  ( -46.05280787783291885, -279.0835004935420329, -344.3412935959492529 ) ) ;
#50716 = CARTESIAN_POINT ( 'NONE',  ( 33.71419598572568788, -291.9203614786669618, -292.5506160771714690 ) ) ;
#50717 = CARTESIAN_POINT ( 'NONE',  ( 36.00213520313938176, -283.6542354542758062, -289.3607838231470737 ) ) ;
#50718 = AXIS2_PLACEMENT_3D ( 'NONE', #5189, #70985, #92265 ) ;
#50719 = VERTEX_POINT ( 'NONE', #52175 ) ;
#50720 = CARTESIAN_POINT ( 'NONE',  ( -86.94631203140275488, -283.4320030987371979, -324.0163969824542960 ) ) ;
#50721 = CARTESIAN_POINT ( 'NONE',  ( -69.84393356210931358, -280.7138156454767568, -200.8838649187784142 ) ) ;
#50722 = CARTESIAN_POINT ( 'NONE',  ( -107.5559965380076335, -283.7410510017319325, -239.6023945491425309 ) ) ;
#50723 = CARTESIAN_POINT ( 'NONE',  ( -113.5311806594003485, -279.3704599795316881, -280.1613874285964698 ) ) ;
#50724 = SHAPE_REPRESENTATION_RELATIONSHIP ( 'NONE' , 'NONE' ,  #80896, #57659 ) ;
#50725 = CARTESIAN_POINT ( 'NONE',  ( 38.03963286382045084, -276.9216938620741644, -258.4295648329849087 ) ) ;
#50726 = CARTESIAN_POINT ( 'NONE',  ( -92.08974858914540107, -281.6948066931272479, -226.7417163044926838 ) ) ;
#50727 = ORIENTED_EDGE ( 'NONE', *, *, #91976, .F. ) ;
#50728 = VERTEX_POINT ( 'NONE', #81973 ) ;
#50729 = CARTESIAN_POINT ( 'NONE',  ( -80.91001088341863579, -299.4608118134544270, -209.3135713977811179 ) ) ;
#50730 = CARTESIAN_POINT ( 'NONE',  ( -110.9114014661921601, -276.4084302246379821, -283.0600420439504887 ) ) ;
#50731 = CARTESIAN_POINT ( 'NONE',  ( -90.09873469613977193, -293.0793954024132972, -215.6010580598285173 ) ) ;
#50732 = CARTESIAN_POINT ( 'NONE',  ( 26.32740895562920258, -292.4085421475554654, -234.3392601364453753 ) ) ;
#50733 = CARTESIAN_POINT ( 'NONE',  ( -106.4609867064203712, -289.6241382072789179, -304.2764854710000009 ) ) ;
#50734 = DIRECTION ( 'NONE',  ( 0.000000000000000000, 0.000000000000000000, 1.000000000000000000 ) ) ;
#50736 = CARTESIAN_POINT ( 'NONE',  ( -52.23063916488089120, -284.2582001884280203, -198.0786172828219946 ) ) ;
#50735 = CARTESIAN_POINT ( 'NONE',  ( -2.254333340841217836, -293.1716730803213977, -338.2395607049411410 ) ) ;
#50737 = CARTESIAN_POINT ( 'NONE',  ( -47.18124592499035685, -293.7862433429260705, -196.7808976971628567 ) ) ;
#50738 = CARTESIAN_POINT ( 'NONE',  ( -38.61767950440530939, -284.5157764704475198, -196.6662290483114077 ) ) ;
#50739 = CARTESIAN_POINT ( 'NONE',  ( -76.37494997296566623, -284.9008398512291365, -332.6920662321321629 ) ) ;
#50740 = ORIENTED_EDGE ( 'NONE', *, *, #52524, .T. ) ;
#50741 = CARTESIAN_POINT ( 'NONE',  ( -102.0963135441440244, -290.9502177219982855, -311.6858505583379610 ) ) ;
#50742 = CARTESIAN_POINT ( 'NONE',  ( -46.47035794410771103, -280.4256689822112207, -197.8209659284459860 ) ) ;
#50743 = CARTESIAN_POINT ( 'NONE',  ( 38.42154991089551430, -292.4892729283961330, -281.6721153807094424 ) ) ;
#50744 = CARTESIAN_POINT ( 'NONE',  ( -12.26674238007786499, -289.5370301748904467, -343.0488609188486748 ) ) ;
#50745 = CARTESIAN_POINT ( 'NONE',  ( 31.63503424509521977, -288.4842000853440140, -304.5655557062778485 ) ) ;
#50746 = CARTESIAN_POINT ( 'NONE',  ( -62.56486507424283161, -285.8814005000231759, -201.8032535258574285 ) ) ;
#50747 = VERTEX_POINT ( 'NONE', #73952 ) ;
#50748 = CARTESIAN_POINT ( 'NONE',  ( 16.69743347904245923, -296.1541367301069272, -323.5401653480811319 ) ) ;
#50749 = CARTESIAN_POINT ( 'NONE',  ( -70.60867867298426859, -294.1664226859015798, -339.2711560559325221 ) ) ;
#50750 = CARTESIAN_POINT ( 'NONE',  ( -107.4489064527324160, -277.8903522662457135, -249.1859421936339913 ) ) ;
#50751 = CARTESIAN_POINT ( 'NONE',  ( -52.52733496536654911, -273.3704382455338759, -194.8817693074799422 ) ) ;
#50752 = CARTESIAN_POINT ( 'NONE',  ( -4.040505564498671376, -293.0846749569743679, -336.1151760675631408 ) ) ;
#50753 = CARTESIAN_POINT ( 'NONE',  ( 33.06900828615941634, -277.6107754190001060, -293.1713383672232567 ) ) ;
#50754 = CARTESIAN_POINT ( 'NONE',  ( -95.56702226212388496, -271.3308114531208162, -224.3103053257931663 ) ) ;
#50755 = CARTESIAN_POINT ( 'NONE',  ( 6.903457906644599795, -293.8748944755399748, -211.7992148872943119 ) ) ;
#50756 = CARTESIAN_POINT ( 'NONE',  ( -36.98027337336755238, -296.1271627618154412, -343.6818172421015447 ) ) ;
#50757 = FACE_OUTER_BOUND ( 'NONE', #81817, .T. ) ;
#50758 = CARTESIAN_POINT ( 'NONE',  ( -106.0857824942959695, -294.9508387485374783, -239.8305610484518695 ) ) ;
#50759 = CARTESIAN_POINT ( 'NONE',  ( -57.37117490026938071, -298.4517819281128936, -196.0621710246494160 ) ) ;
#50760 = CARTESIAN_POINT ( 'NONE',  ( -64.04190175609727476, -275.7040825153271157, -200.2608782645664007 ) ) ;
#50761 = CARTESIAN_POINT ( 'NONE',  ( -94.27967900351522701, -290.8439995039550467, -316.4205905208636977 ) ) ;
#50762 = CARTESIAN_POINT ( 'NONE',  ( -38.33832540295010460, -295.3982680791398252, -343.3754605799539377 ) ) ;
#50763 = CARTESIAN_POINT ( 'NONE',  ( -95.76287256738045528, -279.8791551393359214, -317.9772558348826124 ) ) ;
#50764 = CARTESIAN_POINT ( 'NONE',  ( -74.75207895309200978, -278.2497119911328127, -203.6246075156549864 ) ) ;
#50765 = ORIENTED_EDGE ( 'NONE', *, *, #24713, .T. ) ;
#50766 = CARTESIAN_POINT ( 'NONE',  ( -0.4316617390987354530, -281.9233504309728460, -337.8368537223751105 ) ) ;
#50767 = CARTESIAN_POINT ( 'NONE',  ( 37.80429224485347106, -275.1059065389146667, -286.7441482194013815 ) ) ;
#50768 = CARTESIAN_POINT ( 'NONE',  ( -69.60491725636561000, -278.0344500815253923, -201.3140957296970157 ) ) ;
#50769 = CARTESIAN_POINT ( 'NONE',  ( 0.4742104381092190901, -278.5542552046782134, -205.3404340612911767 ) ) ;
#50770 = CARTESIAN_POINT ( 'NONE',  ( -96.48730095058181178, -295.8445424001401420, -226.7160153247493497 ) ) ;
#50771 = CARTESIAN_POINT ( 'NONE',  ( 36.98253148569139626, -277.6860573295540462, -280.7773555883468930 ) ) ;
#50772 = CARTESIAN_POINT ( 'NONE',  ( 188.3531807883583440, 45.29379214021909661, 10.50000000000000000 ) ) ;
#50773 = CARTESIAN_POINT ( 'NONE',  ( -70.15814442175897625, -289.6420187720629542, -202.5268508920531758 ) ) ;
#50774 = CARTESIAN_POINT ( 'NONE',  ( -82.85264511769260309, -289.6556945937999785, -332.4719373794459329 ) ) ;
#50775 = CARTESIAN_POINT ( 'NONE',  ( 35.50210460976308724, -277.3146272681639743, -251.8190430911533326 ) ) ;
#50776 = CARTESIAN_POINT ( 'NONE',  ( -83.04413536489295211, -295.4252800982309282, -211.0391032491959606 ) ) ;
#50777 = CARTESIAN_POINT ( 'NONE',  ( -73.52791007730634476, -284.7820242808957119, -202.5178488926247269 ) ) ;
#50778 = DIRECTION ( 'NONE',  ( -6.167905692361989633E-15, 0.000000000000000000, 1.000000000000000000 ) ) ;
#50779 = CARTESIAN_POINT ( 'NONE',  ( -97.44968100573896663, -281.9391343560257042, -315.2379391244991211 ) ) ;
#50780 = CIRCLE ( 'NONE', #59856, 12.40608546931776957 ) ;
#50781 = DIRECTION ( 'NONE',  ( 0.000000000000000000, 1.000000000000000000, 0.000000000000000000 ) ) ;
#50782 = CARTESIAN_POINT ( 'NONE',  ( -17.30956238412722570, -291.1112886620433642, -199.6977270563631635 ) ) ;
#50783 = CARTESIAN_POINT ( 'NONE',  ( -105.7263268552588897, -283.0745539338489607, -241.3429665046753598 ) ) ;
#50784 = DIRECTION ( 'NONE',  ( 0.000000000000000000, 0.000000000000000000, 1.000000000000000000 ) ) ;
#50785 = CARTESIAN_POINT ( 'NONE',  ( -74.94434090351494149, -277.8906705383787994, 30.50000000000000000 ) ) ;
#50786 = CARTESIAN_POINT ( 'NONE',  ( -8.947307919121019637, -290.4232240490219965, -200.8885671734395260 ) ) ;
#50787 = CARTESIAN_POINT ( 'NONE',  ( -63.69093037313236749, -281.8694044047651346, -341.9741462506141829 ) ) ;
#50788 = CARTESIAN_POINT ( 'NONE',  ( -94.20959947682335667, -279.4924573109801145, -317.4179434772631225 ) ) ;
#50789 = CARTESIAN_POINT ( 'NONE',  ( -108.6644279661540082, -286.1149502404304030, -242.2690279585470989 ) ) ;
#50790 = CARTESIAN_POINT ( 'NONE',  ( -57.39438582579897030, -285.7861674244165897, -200.1166974895409396 ) ) ;
#50791 = CARTESIAN_POINT ( 'NONE',  ( -109.8636942137055712, -279.8130446852018167, -282.9229001058603785 ) ) ;
#50792 = CARTESIAN_POINT ( 'NONE',  ( -83.54761871295198716, -280.2026885517768164, -213.5715159063096849 ) ) ;
#50793 = CARTESIAN_POINT ( 'NONE',  ( -111.1636761064662977, -286.3786482079773918, -283.8864502161146106 ) ) ;
#50794 = ORIENTED_EDGE ( 'NONE', *, *, #4124, .T. ) ;
#50795 = CARTESIAN_POINT ( 'NONE',  ( -30.48245140136254605, -297.9691305585425880, -193.3613054221744960 ) ) ;
#50796 = CARTESIAN_POINT ( 'NONE',  ( -18.02406063249808099, -290.7819362710985160, -342.5167353693213954 ) ) ;
#50797 = CARTESIAN_POINT ( 'NONE',  ( 197.4375396935993763, 24.88665474053331650, 11.71825508031673024 ) ) ;
#50798 = CARTESIAN_POINT ( 'NONE',  ( -72.08107566293803359, -288.1233781216987495, -198.2974183793908196 ) ) ;
#50799 = ORIENTED_EDGE ( 'NONE', *, *, #470, .F. ) ;
#50800 = CARTESIAN_POINT ( 'NONE',  ( 33.72419005074169718, -291.5983825486693490, -242.7182971222643744 ) ) ;
#50801 = CARTESIAN_POINT ( 'NONE',  ( 36.37336663727020181, -289.0450043253065928, -268.2736880560483996 ) ) ;
#50802 = CARTESIAN_POINT ( 'NONE',  ( 34.08569886428286821, -283.0590458122868540, -250.9193692827377333 ) ) ;
#50803 = CARTESIAN_POINT ( 'NONE',  ( 36.22210640171046947, -289.2389047819781354, -291.0724606052908712 ) ) ;
#50804 = CARTESIAN_POINT ( 'NONE',  ( 38.19086499478468255, -289.0245762020866209, -282.8544962804359670 ) ) ;
#50805 = CARTESIAN_POINT ( 'NONE',  ( -94.05523728357189839, -285.8714485915557475, -319.4578920669638364 ) ) ;
#50806 = CARTESIAN_POINT ( 'NONE',  ( -97.92759369401956349, -278.0835456849674188, -317.8832129001044677 ) ) ;
#50807 = ORIENTED_EDGE ( 'NONE', *, *, #43456, .F. ) ;
#50808 = CARTESIAN_POINT ( 'NONE',  ( -5.138864125718958675, -292.7114819676794468, -338.7294772909415315 ) ) ;
#50809 = CARTESIAN_POINT ( 'NONE',  ( 37.67798015011608470, -281.1678237666186533, -252.9524576551812061 ) ) ;
#50810 = CARTESIAN_POINT ( 'NONE',  ( -83.98476371509421767, -275.2637606583527941, -212.6091474824507941 ) ) ;
#50811 = DIRECTION ( 'NONE',  ( 0.000000000000000000, 0.000000000000000000, 1.000000000000000000 ) ) ;
#50812 = ADVANCED_FACE ( 'NONE', ( #37493 ), #31344, .T. ) ;
#50813 = CARTESIAN_POINT ( 'NONE',  ( -69.85430415644619018, -291.9805209788416391, -337.9475929042657754 ) ) ;
#50814 = CARTESIAN_POINT ( 'NONE',  ( -57.82659860805578234, -272.0311321130779447, -197.1330511315456704 ) ) ;
#50815 = DIRECTION ( 'NONE',  ( 0.000000000000000000, -0.000000000000000000, 1.000000000000000000 ) ) ;
#50816 = CARTESIAN_POINT ( 'NONE',  ( -14.28351504931984017, -279.8668964921849351, -200.9800866251921434 ) ) ;
#50817 = CARTESIAN_POINT ( 'NONE',  ( -11.98307774365967937, -277.9345030618075612, -342.7005696370524106 ) ) ;
#50818 = CARTESIAN_POINT ( 'NONE',  ( -63.30420472870662252, -299.1325798379118055, -201.4499332045505753 ) ) ;
#50819 = CARTESIAN_POINT ( 'NONE',  ( -65.17807595261378140, -282.4658927849517340, -341.9151730905829254 ) ) ;
#50820 = CARTESIAN_POINT ( 'NONE',  ( -93.16140682518464189, -291.6280854516674594, -319.0394720045267150 ) ) ;
#50821 = CARTESIAN_POINT ( 'NONE',  ( -99.36935526849525502, -298.6665412092883116, -225.9170210588498833 ) ) ;
#50822 = CARTESIAN_POINT ( 'NONE',  ( -14.96982002085689700, -299.5314604421131435, -193.7537215998492570 ) ) ;
#50823 = CARTESIAN_POINT ( 'NONE',  ( 34.10455622380240470, -295.8400433987417841, -292.6200685462527531 ) ) ;
#50824 = CARTESIAN_POINT ( 'NONE',  ( -43.09875214564075208, -281.1247050262921334, -345.0240214393301699 ) ) ;
#50825 = CARTESIAN_POINT ( 'NONE',  ( -79.57926831555381852, -291.1653667752359524, -205.9411111316073004 ) ) ;
#50826 = CARTESIAN_POINT ( 'NONE',  ( -36.69709821686532081, -272.0803988026510751, -195.7064017538280041 ) ) ;
#50827 = CARTESIAN_POINT ( 'NONE',  ( -65.59982650302146112, -287.2888733781849169, -199.5804589851779269 ) ) ;
#50828 = CARTESIAN_POINT ( 'NONE',  ( -72.51921916857611450, -288.4498391899437024, -334.6788311593118692 ) ) ;
#50829 = CARTESIAN_POINT ( 'NONE',  ( -82.59061302912155611, -220.2773766338590633, -352.3396032511032558 ) ) ;
#50830 = ORIENTED_EDGE ( 'NONE', *, *, #75705, .T. ) ;
#50831 = CARTESIAN_POINT ( 'NONE',  ( -96.11393532843437981, -289.7887860191331697, -221.5102719404187610 ) ) ;
#50832 = CARTESIAN_POINT ( 'NONE',  ( -42.66969263814385727, -288.7877950589927423, -343.2382426531012811 ) ) ;
#50833 = ORIENTED_EDGE ( 'NONE', *, *, #7831, .F. ) ;
#50834 = CARTESIAN_POINT ( 'NONE',  ( -15.51464989385819848, -287.4077357868389413, -196.7867540621706723 ) ) ;
#50835 = CARTESIAN_POINT ( 'NONE',  ( 0.8861114934221715478, -276.8604751478663957, -332.6356594363435306 ) ) ;
#50836 = EDGE_CURVE ( 'NONE', #43740, #67960, #10447, .T. ) ;
#50837 = CARTESIAN_POINT ( 'NONE',  ( 33.04616037973165987, -292.0829378409865171, -239.9137600995213120 ) ) ;
#50838 = CARTESIAN_POINT ( 'NONE',  ( -112.4237661626760314, -284.9955161575650209, -286.9742497502320475 ) ) ;
#50839 = CARTESIAN_POINT ( 'NONE',  ( 6.542239102787454463, -283.9881232360132230, -332.8509590032899723 ) ) ;
#50840 = CARTESIAN_POINT ( 'NONE',  ( -76.74342330689559333, -283.8973773675526218, -336.5534597473719032 ) ) ;
#50841 = CARTESIAN_POINT ( 'NONE',  ( 22.12824792924733330, -281.2936889681581647, -227.9888066828895319 ) ) ;
#50842 = CARTESIAN_POINT ( 'NONE',  ( -112.4251224187018465, -271.4489424832871691, -296.3911511650422881 ) ) ;
#50843 = CARTESIAN_POINT ( 'NONE',  ( 200.9643288768799607, 293.5986974642797236, -83.07126776150519731 ) ) ;
#50844 = CARTESIAN_POINT ( 'NONE',  ( -71.24468398583613293, -195.3788060869234755, -356.9306778524392030 ) ) ;
#50845 = CARTESIAN_POINT ( 'NONE',  ( -64.61951886301119430, -272.8838609646115856, -202.4615110291326801 ) ) ;
#50846 = CARTESIAN_POINT ( 'NONE',  ( -3.261686557078808946, -294.1218671727963283, -339.3545440673736948 ) ) ;
#50847 = CARTESIAN_POINT ( 'NONE',  ( -54.50862104011823561, -170.0898157090607299, -361.0194490113770485 ) ) ;
#50848 = CARTESIAN_POINT ( 'NONE',  ( -55.20214254111591146, -272.5118857717246783, -195.9682227019258391 ) ) ;
#50849 = CARTESIAN_POINT ( 'NONE',  ( -111.3282006056732314, -298.3260144464038035, -277.0338532795914261 ) ) ;
#50850 = CARTESIAN_POINT ( 'NONE',  ( 34.18643073227132589, -288.6454207686007294, -253.4257274208140416 ) ) ;
#50851 = VERTEX_POINT ( 'NONE', #38427 ) ;
#50852 = CARTESIAN_POINT ( 'NONE',  ( -22.13240718812397034, -295.8031420716584989, -345.6040420389776955 ) ) ;
#50853 = AXIS2_PLACEMENT_3D ( 'NONE', #7958, #45317, #36853 ) ;
#50854 = CARTESIAN_POINT ( 'NONE',  ( -6.996661576786002534, -286.9537537187511589, -203.8856087334964968 ) ) ;
#50855 = CARTESIAN_POINT ( 'NONE',  ( -73.78580049746170744, -272.5005970861380433, -202.8237949150263262 ) ) ;
#50856 = CARTESIAN_POINT ( 'NONE',  ( 37.30557950669378187, -294.5839869356539680, -288.6354919991429142 ) ) ;
#50857 = CARTESIAN_POINT ( 'NONE',  ( -99.95476595430773159, -296.4507365763180928, -315.1624850692325026 ) ) ;
#50858 = CARTESIAN_POINT ( 'NONE',  ( -77.25693139233162299, -291.6670159748055653, -209.2401369890033038 ) ) ;
#50859 = VERTEX_POINT ( 'NONE', #80586 ) ;
#50860 = CARTESIAN_POINT ( 'NONE',  ( -65.70971136271141688, -275.6041903581665338, -200.3145743447263953 ) ) ;
#50861 = CARTESIAN_POINT ( 'NONE',  ( 24.17023763975591777, -273.7369336271359543, -224.7070904316422570 ) ) ;
#50862 = VERTEX_POINT ( 'NONE', #88616 ) ;
#50863 = CARTESIAN_POINT ( 'NONE',  ( -103.5560301905008629, -277.5477989348951269, -309.6471017368729122 ) ) ;
#50864 = CARTESIAN_POINT ( 'NONE',  ( 28.58498052853238391, -273.5067583028380227, -237.1931637098956855 ) ) ;
#50865 = CARTESIAN_POINT ( 'NONE',  ( -110.4982612007245990, -273.7035134877704081, -264.9040783715561247 ) ) ;
#50866 = CARTESIAN_POINT ( 'NONE',  ( 7.465445680261517225, -275.6219831932619968, -212.4324710806345422 ) ) ;
#50867 = CARTESIAN_POINT ( 'NONE',  ( 97.40392376569691635, -301.3126994743653313, -194.1250687223027001 ) ) ;
#50868 = CARTESIAN_POINT ( 'NONE',  ( 36.29292874655875778, -273.7776425915074014, -286.4321930518889872 ) ) ;
#50869 = CARTESIAN_POINT ( 'NONE',  ( -45.09330768877237006, -295.8041826238767271, -343.1014528061047031 ) ) ;
#50870 = CARTESIAN_POINT ( 'NONE',  ( 34.79767957394593481, -291.9366630849207240, -255.8254785111904823 ) ) ;
#50871 = LINE ( 'NONE', #79303, #6420 ) ;
#50872 = CARTESIAN_POINT ( 'NONE',  ( -108.4581650032118603, -279.4179430854298403, -241.0017016610278802 ) ) ;
#50873 = CARTESIAN_POINT ( 'NONE',  ( 35.02022914173060286, -275.5917875855570287, -260.7303757030665565 ) ) ;
#50874 = CARTESIAN_POINT ( 'NONE',  ( -95.43107978121291524, -283.9138448870438083, -220.4929019986416847 ) ) ;
#50875 = CARTESIAN_POINT ( 'NONE',  ( -112.5315993034798367, -298.5256188962545139, -272.4450014759427745 ) ) ;
#50876 = CARTESIAN_POINT ( 'NONE',  ( 41.08708295871279859, -293.9068999365417199, -465.6442049081569508 ) ) ;
#50877 = CARTESIAN_POINT ( 'NONE',  ( -9.422326905928947838, -285.6237696785283902, -202.7228032636003263 ) ) ;
#50878 = CARTESIAN_POINT ( 'NONE',  ( -109.4789013923819709, -276.5758298443051899, -286.9762884760010024 ) ) ;
#50879 = CARTESIAN_POINT ( 'NONE',  ( -73.14442872080606151, -276.1113507012303216, -334.6682263215733428 ) ) ;
#50880 = CARTESIAN_POINT ( 'NONE',  ( -22.79041941096711810, -284.8662421930104074, -343.9882306272708661 ) ) ;
#50881 = CARTESIAN_POINT ( 'NONE',  ( 16.83455455260827804, -277.4638744020754757, -319.8981872453594519 ) ) ;
#50882 = CARTESIAN_POINT ( 'NONE',  ( 155.0589890788434388, 20.95955078618711553, 14.77888609071400872 ) ) ;
#50883 = CARTESIAN_POINT ( 'NONE',  ( 26.27401679483157437, -273.3946727148648392, -228.4149503928773299 ) ) ;
#50884 = CARTESIAN_POINT ( 'NONE',  ( -16.61970088106266275, -274.9783366215162346, -200.2049044040248020 ) ) ;
#50885 = CARTESIAN_POINT ( 'NONE',  ( -38.17574050438641109, -282.0418783454302911, -195.1990743197127927 ) ) ;
#50886 = CARTESIAN_POINT ( 'NONE',  ( 144.2857639756989272, -299.5541904835127980, -195.3611179825600175 ) ) ;
#50887 = CARTESIAN_POINT ( 'NONE',  ( 29.10818525265068146, -289.9476976713093563, -306.4390229381738777 ) ) ;
#50888 = CARTESIAN_POINT ( 'NONE',  ( 7.065082734878200377, -292.4477149551959769, -330.8652190956427148 ) ) ;
#50889 = CARTESIAN_POINT ( 'NONE',  ( 156.4851178187871312, 0.000000000000000000, 7.000000000000000000 ) ) ;
#50890 = CARTESIAN_POINT ( 'NONE',  ( -96.66962088441499645, -271.8413216895959863, -226.9010071387581036 ) ) ;
#50891 = CARTESIAN_POINT ( 'NONE',  ( -111.6028274538085299, -288.7170912920631167, -268.4059816993565164 ) ) ;
#50892 = CARTESIAN_POINT ( 'NONE',  ( -87.49538389815894845, -233.3606102865802825, -350.3678815354037965 ) ) ;
#50893 = DIRECTION ( 'NONE',  ( -0.000000000000000000, -1.000000000000000000, -0.000000000000000000 ) ) ;
#50894 = CARTESIAN_POINT ( 'NONE',  ( -110.1264292753925815, -288.7394915632573316, -293.4487458996985083 ) ) ;
#50895 = CARTESIAN_POINT ( 'NONE',  ( -93.15992892245486701, -283.5040989628280386, -218.7253317404775430 ) ) ;
#50896 = CARTESIAN_POINT ( 'NONE',  ( -56.45459091555333941, -284.7286266506664560, -341.4249788494714721 ) ) ;
#50897 = CARTESIAN_POINT ( 'NONE',  ( -87.03102608431292708, -284.5679339385695243, -324.1293253957367142 ) ) ;
#50898 = CARTESIAN_POINT ( 'NONE',  ( -67.37466906241759546, -291.4239754838623639, -339.4728216384142456 ) ) ;
#50899 = CARTESIAN_POINT ( 'NONE',  ( 22.73918388317162709, -275.2403867254857914, -222.2150498502134610 ) ) ;
#50900 = CARTESIAN_POINT ( 'NONE',  ( -83.36943941162631688, -289.5071921624210063, -210.3722277984543894 ) ) ;
#50901 = CARTESIAN_POINT ( 'NONE',  ( -45.64961730087578218, -277.1545523770471959, -346.9646729534728706 ) ) ;
#50902 = CARTESIAN_POINT ( 'NONE',  ( 20.11494765181627642, -296.1929397740404966, -318.0117258705380436 ) ) ;
#50903 = CARTESIAN_POINT ( 'NONE',  ( 170.1758599444071081, 214.8829713991971744, -24.64732457002846644 ) ) ;
#50904 = CARTESIAN_POINT ( 'NONE',  ( 31.98288692825981272, -296.4805209788415823, -303.7098442033569654 ) ) ;
#50905 = CARTESIAN_POINT ( 'NONE',  ( -1.022770520093521540, -281.2440253241451273, -334.2530488546613014 ) ) ;
#50906 = CARTESIAN_POINT ( 'NONE',  ( -112.2152288144974221, -276.6442006766164354, -263.1635230051749090 ) ) ;
#50907 = CARTESIAN_POINT ( 'NONE',  ( -110.3678891299274056, -271.3144546575006189, -248.0473400826790851 ) ) ;
#50908 = CARTESIAN_POINT ( 'NONE',  ( 9.723352830516123646, -275.7325617673797638, -326.2965580706182323 ) ) ;
#50909 = CARTESIAN_POINT ( 'NONE',  ( -63.06066959920939041, -293.2311483973861641, -201.3014165520490053 ) ) ;
#50910 = CARTESIAN_POINT ( 'NONE',  ( 2.358014669068211333, -293.5393642680079438, -208.7596732287359771 ) ) ;
#50911 = CARTESIAN_POINT ( 'NONE',  ( -33.58661477011126806, -293.5238168183002472, -194.0426691797958370 ) ) ;
#50912 = CARTESIAN_POINT ( 'NONE',  ( 26.07468385097006092, -294.2986809761601990, -227.4700500995605807 ) ) ;
#50913 = CARTESIAN_POINT ( 'NONE',  ( -63.57097602943072445, -295.2369566199428164, -338.5397463182231377 ) ) ;
#50914 = CARTESIAN_POINT ( 'NONE',  ( -17.93200341822250010, -290.8022012981047624, -342.8600548049010968 ) ) ;
#50915 = CARTESIAN_POINT ( 'NONE',  ( -102.9169673524919801, -284.1913278749609617, -310.7205571875689998 ) ) ;
#50916 = CARTESIAN_POINT ( 'NONE',  ( -80.52658104247448989, -271.6135753591577782, -208.0450735875317037 ) ) ;
#50917 = CARTESIAN_POINT ( 'NONE',  ( -3.487441953261195327, -286.3200341203349240, -201.1881542722341862 ) ) ;
#50918 = CARTESIAN_POINT ( 'NONE',  ( -67.44334330470294958, -279.4288450031614843, -338.6673247536235749 ) ) ;
#50919 = EDGE_CURVE ( 'NONE', #5640, #3067, #30404, .T. ) ;
#50920 = CARTESIAN_POINT ( 'NONE',  ( -85.97784978780988752, -284.1555368381430071, -215.3236148577962297 ) ) ;
#50921 = CARTESIAN_POINT ( 'NONE',  ( -29.21975367704297710, -286.9492078422037480, -344.9721863633606063 ) ) ;
#50922 = CARTESIAN_POINT ( 'NONE',  ( -70.66955292945459632, -277.7569018184060496, -202.3202500256892051 ) ) ;
#50923 = CARTESIAN_POINT ( 'NONE',  ( 116.7412556412048872, 151.1295779098236665, -261.7160256675778101 ) ) ;
#50924 = CARTESIAN_POINT ( 'NONE',  ( -70.00431895928686288, -285.1175487550798380, -204.9931896772217215 ) ) ;
#50925 = CARTESIAN_POINT ( 'NONE',  ( 35.79203067962625084, -282.4694106255584529, -247.5693182130149239 ) ) ;
#50926 = CARTESIAN_POINT ( 'NONE',  ( 12.25465303853404642, -287.4398882375414246, -328.9531137232041260 ) ) ;
#50927 = CARTESIAN_POINT ( 'NONE',  ( -97.28681268844545116, -279.5167619965732229, -317.4039059383642893 ) ) ;
#50928 = CARTESIAN_POINT ( 'NONE',  ( -84.54884574960647114, -279.0017253002762914, -330.6345996472991260 ) ) ;
#50929 = CARTESIAN_POINT ( 'NONE',  ( -95.61046795058176428, -279.0034279764616940, -226.3659374065110796 ) ) ;
#50930 = CARTESIAN_POINT ( 'NONE',  ( 20.25220980794826886, -276.8738665047488894, -222.8765063205398747 ) ) ;
#50931 = CARTESIAN_POINT ( 'NONE',  ( 39.60688391750915116, -293.5873380482357788, -273.1745524279834854 ) ) ;
#50932 = CARTESIAN_POINT ( 'NONE',  ( -83.58454293498222398, -287.7102132997681565, -328.9567346163393040 ) ) ;
#50933 = CARTESIAN_POINT ( 'NONE',  ( -1.201436748137719501, -294.1236286711109642, -203.2766802979610645 ) ) ;
#50934 = CARTESIAN_POINT ( 'NONE',  ( -73.46665075974691206, -294.4638878973798342, -334.1515092322806595 ) ) ;
#50935 = CARTESIAN_POINT ( 'NONE',  ( 35.64259782757726924, -293.1882805918654071, -268.0416916304655501 ) ) ;
#50936 = CARTESIAN_POINT ( 'NONE',  ( -110.1418420663086266, -291.9384873975006940, -246.0777937725686968 ) ) ;
#50937 = CARTESIAN_POINT ( 'NONE',  ( 32.33099770372923842, -282.4984913336941190, -292.6531239611390447 ) ) ;
#50938 = EDGE_CURVE ( 'NONE', #22426, #72058, #9067, .T. ) ;
#50939 = ADVANCED_FACE ( 'NONE', ( #66854 ), #10012, .F. ) ;
#50940 = CARTESIAN_POINT ( 'NONE',  ( -81.10637535350065264, -272.5325913237194868, -207.2294969941391685 ) ) ;
#50941 = CARTESIAN_POINT ( 'NONE',  ( -73.11907485539609297, -290.1651221641153597, -338.4441452574731670 ) ) ;
#50942 = CARTESIAN_POINT ( 'NONE',  ( -27.55550236442894629, -281.0688231859247708, -345.5437479406617740 ) ) ;
#50943 = CARTESIAN_POINT ( 'NONE',  ( -37.49728615799227072, -289.3872929793831190, -347.3528851897505660 ) ) ;
#50944 = CARTESIAN_POINT ( 'NONE',  ( -44.03053703779866623, -286.2985344710945697, -197.6469725391537793 ) ) ;
#50945 = CARTESIAN_POINT ( 'NONE',  ( 24.96937360126054273, -22.70870616253715824, -344.9910381550040483 ) ) ;
#50946 = CARTESIAN_POINT ( 'NONE',  ( 159.2431035810776905, 219.8277306504076307, -203.5701272057735878 ) ) ;
#50947 = CARTESIAN_POINT ( 'NONE',  ( -93.74409744368286113, -238.7666546281632804, -338.5088866427397534 ) ) ;
#50948 = CARTESIAN_POINT ( 'NONE',  ( -105.6614162580993650, -278.0997785501654675, -244.0464234553423069 ) ) ;
#50949 = CARTESIAN_POINT ( 'NONE',  ( -87.73316560708165923, -278.2487418301028015, -217.0469511595870244 ) ) ;
#50950 = CARTESIAN_POINT ( 'NONE',  ( -3.831473428062826425, -274.1488981792788309, -201.0443114855024476 ) ) ;
#50951 = CARTESIAN_POINT ( 'NONE',  ( -110.4560631405595643, -273.2888399267177419, -270.3704977824100979 ) ) ;
#50952 = CARTESIAN_POINT ( 'NONE',  ( -113.4552190830244456, -277.2189962577540996, -263.0520944849046714 ) ) ;
#50953 = CARTESIAN_POINT ( 'NONE',  ( -88.06460109016667559, -281.7856572128818584, -325.1952930489084110 ) ) ;
#50954 = CARTESIAN_POINT ( 'NONE',  ( -74.09630248089541737, -297.2933515904690012, -336.9262263504716657 ) ) ;
#50955 = CARTESIAN_POINT ( 'NONE',  ( -32.15917367351151768, -292.6116002623460872, -197.4709880223978473 ) ) ;
#50956 = CARTESIAN_POINT ( 'NONE',  ( -99.26624624139137154, -288.6931917087532611, -309.9413411553215951 ) ) ;
#50957 = CARTESIAN_POINT ( 'NONE',  ( -3.877972876050205908, -275.1334331069022028, -201.1115825374340886 ) ) ;
#50958 = CARTESIAN_POINT ( 'NONE',  ( -97.18216028420732755, -296.1358376802232897, -312.1716349946260038 ) ) ;
#50959 = ORIENTED_EDGE ( 'NONE', *, *, #50919, .T. ) ;
#50960 = FACE_OUTER_BOUND ( 'NONE', #28161, .T. ) ;
#50961 = CARTESIAN_POINT ( 'NONE',  ( 196.5168303497916895, 24.84897060197241814, 13.11473570156704405 ) ) ;
#50962 = CARTESIAN_POINT ( 'NONE',  ( -92.04838421226122591, -281.1990888989095083, -218.1663481207656616 ) ) ;
#50963 = CARTESIAN_POINT ( 'NONE',  ( -46.50868548182884155, -281.0128985697700159, -197.5760893315352575 ) ) ;
#50964 = CARTESIAN_POINT ( 'NONE',  ( -9.256757258909233954, -282.1744649884686851, -199.7550984223298940 ) ) ;
#50965 = CARTESIAN_POINT ( 'NONE',  ( -10.90197354023956677, -281.7576543484078115, -338.7109086237585416 ) ) ;
#50966 = CARTESIAN_POINT ( 'NONE',  ( -68.55882751477295756, -272.1142347183406400, -203.5925259070333766 ) ) ;
#50967 = CARTESIAN_POINT ( 'NONE',  ( 196.7510731661265595, -142.7221692137691775, 21.50000000000000000 ) ) ;
#50968 = LINE ( 'NONE', #79852, #35069 ) ;
#50969 = CARTESIAN_POINT ( 'NONE',  ( 36.42793918752401794, -276.0826956006137038, -248.6764523678102421 ) ) ;
#50970 = CARTESIAN_POINT ( 'NONE',  ( 164.8310050610337498, 214.8829733828359565, 22.91067844396894060 ) ) ;
#50971 = CARTESIAN_POINT ( 'NONE',  ( 20.21266117828161057, -278.2166602070761883, -318.4495380733854972 ) ) ;
#50972 = CARTESIAN_POINT ( 'NONE',  ( -12.07825596151696956, -275.3045789554300313, -342.5301652189041874 ) ) ;
#50973 = EDGE_LOOP ( 'NONE', ( #80144, #85090 ) ) ;
#50974 = CYLINDRICAL_SURFACE ( 'NONE', #88245, 0.5000000000000004441 ) ;
#50975 = CARTESIAN_POINT ( 'NONE',  ( -75.89425137132091947, -285.5437228061603037, -335.1680927717017084 ) ) ;
#50976 = CARTESIAN_POINT ( 'NONE',  ( 29.63378567290673971, -293.1445530632305463, -299.8040463046418154 ) ) ;
#50977 = CARTESIAN_POINT ( 'NONE',  ( -33.72381460238398176, -285.4451497863647091, -193.5482044125795937 ) ) ;
#50978 = CARTESIAN_POINT ( 'NONE',  ( -95.93217628199963087, -282.1638250617883159, -315.6049286642285097 ) ) ;
#50979 = CARTESIAN_POINT ( 'NONE',  ( -10.77989302364126800, -281.2737121324661302, -339.0434373999217428 ) ) ;
#50980 = CARTESIAN_POINT ( 'NONE',  ( 12.19592657620327891, -283.5492645987591800, -324.5197188179855061 ) ) ;
#50981 = CARTESIAN_POINT ( 'NONE',  ( -66.72791628044898005, -271.6670035016841780, -201.3578502986385388 ) ) ;
#50982 = CARTESIAN_POINT ( 'NONE',  ( -111.1057353475587917, -282.7097134914578191, -289.5259226527679743 ) ) ;
#50983 = CARTESIAN_POINT ( 'NONE',  ( -109.2893851079527252, -298.2790390368232352, -291.5849199021723734 ) ) ;
#50984 = CARTESIAN_POINT ( 'NONE',  ( -91.47880715477889169, -280.1983502611237782, -221.0399045835715697 ) ) ;
#50985 = CARTESIAN_POINT ( 'NONE',  ( -51.84510091347816285, -287.8672905728646469, -196.5538343999191113 ) ) ;
#50986 = DIRECTION ( 'NONE',  ( 0.000000000000000000, 0.000000000000000000, 1.000000000000000000 ) ) ;
#50987 = DIRECTION ( 'NONE',  ( -0.000000000000000000, 1.000000000000000000, 0.000000000000000000 ) ) ;
#50988 = CARTESIAN_POINT ( 'NONE',  ( 34.90286814260568349, -295.1890382577763035, -248.2243487094521015 ) ) ;
#50989 = CARTESIAN_POINT ( 'NONE',  ( -48.94163486376639582, -275.1996230818745630, -344.5114353270543575 ) ) ;
#50990 = CARTESIAN_POINT ( 'NONE',  ( -41.76150947437994176, -288.3036439178633259, -347.0856160532400736 ) ) ;
#50991 = CARTESIAN_POINT ( 'NONE',  ( 25.54008364571286549, -291.4241584403899878, -231.6334817727388895 ) ) ;
#50992 = CARTESIAN_POINT ( 'NONE',  ( -40.54390445751135275, -275.7780482727015396, -343.7970234432891061 ) ) ;
#50993 = CARTESIAN_POINT ( 'NONE',  ( -91.32142545007197043, -293.9692792276212003, -321.3964809502224966 ) ) ;
#50994 = CARTESIAN_POINT ( 'NONE',  ( -105.1645984978421069, -292.2460609290928915, -241.9214067118645914 ) ) ;
#50995 = CARTESIAN_POINT ( 'NONE',  ( -20.19161114001083490, -285.3376638359844719, -345.3538533559490702 ) ) ;
#50996 = CARTESIAN_POINT ( 'NONE',  ( 23.46465375207146309, -292.6518335754161058, -316.4620407769572239 ) ) ;
#50997 = CARTESIAN_POINT ( 'NONE',  ( -18.24707915307216410, -290.4022335897068956, -341.7012804433098268 ) ) ;
#50998 = CARTESIAN_POINT ( 'NONE',  ( -113.1751167339738089, -288.8531414278379543, -265.5375365763666196 ) ) ;
#50999 = ADVANCED_FACE ( 'NONE', ( #30881 ), #69477, .F. ) ;
#51000 = CARTESIAN_POINT ( 'NONE',  ( 31.03938911176018678, -289.3399650551003788, -297.6905788816848144 ) ) ;
#51001 = CARTESIAN_POINT ( 'NONE',  ( -101.7805382291104195, -290.8823059450201640, -305.1129508036477205 ) ) ;
#51002 = CARTESIAN_POINT ( 'NONE',  ( 195.1553079136006943, 21.00000000000003553, 15.11292322100999819 ) ) ;
#51003 = CARTESIAN_POINT ( 'NONE',  ( -72.97547648096811201, -290.7186951878180707, -338.1861407105386661 ) ) ;
#51004 = CARTESIAN_POINT ( 'NONE',  ( -95.53087620390357415, -277.2296967769691491, -222.4617682166225165 ) ) ;
#51005 = CARTESIAN_POINT ( 'NONE',  ( -22.57439544081095661, -280.5693661488294879, -194.7577481575451941 ) ) ;
#51006 = CARTESIAN_POINT ( 'NONE',  ( 39.16225703207692277, -281.1062278192027293, -261.3566547280000805 ) ) ;
#51007 = CARTESIAN_POINT ( 'NONE',  ( 29.45056055819301477, -285.0995438406746416, -236.1321022833115251 ) ) ;
#51008 = CARTESIAN_POINT ( 'NONE',  ( 194.7510731661265595, -164.3527196417747689, 22.50000000000000000 ) ) ;
#51009 = CARTESIAN_POINT ( 'NONE',  ( 31.47078313542831651, -280.0585113518169464, -298.2126462205336566 ) ) ;
#51010 = CARTESIAN_POINT ( 'NONE',  ( -75.07780795924897177, -283.5496724866497402, -205.4863033057050927 ) ) ;
#51011 = FACE_OUTER_BOUND ( 'NONE', #82042, .T. ) ;
#51012 = CARTESIAN_POINT ( 'NONE',  ( -94.70250776891384703, -276.3448881708775389, -320.6845270535447412 ) ) ;
#51013 = CARTESIAN_POINT ( 'NONE',  ( -110.8157998883666266, -283.1950498810738281, -292.3851274451994300 ) ) ;
#51014 = CARTESIAN_POINT ( 'NONE',  ( -110.0473752105498164, -273.4623154001432681, -262.2071902407515154 ) ) ;
#51015 = CARTESIAN_POINT ( 'NONE',  ( -69.38316837066221865, -293.2235294107999266, -203.8657005363225494 ) ) ;
#51016 = CARTESIAN_POINT ( 'NONE',  ( -111.2530440437265469, -274.2242566822889103, -250.7749510710396521 ) ) ;
#51017 = CARTESIAN_POINT ( 'NONE',  ( 35.71992156475009494, -275.2350692071352114, -271.5895561323770835 ) ) ;
#51018 = CARTESIAN_POINT ( 'NONE',  ( -91.84357065002804177, -297.8292329132049190, -321.9581749194084068 ) ) ;
#51019 = CARTESIAN_POINT ( 'NONE',  ( -80.53885857708523588, -289.7865310167421171, -334.1672384920702257 ) ) ;
#51020 = CARTESIAN_POINT ( 'NONE',  ( 25.10460180199353886, -279.0592042294516091, -227.7283495288590132 ) ) ;
#51021 = CARTESIAN_POINT ( 'NONE',  ( -3.319439481211793996, -292.3223121054058424, -201.2706379079105545 ) ) ;
#51022 = CARTESIAN_POINT ( 'NONE',  ( -44.31070046219010550, -291.0207325948613857, -197.4071773135576677 ) ) ;
#51023 = CARTESIAN_POINT ( 'NONE',  ( 21.58408446128172642, -292.1892730909928559, -316.7794793842076047 ) ) ;
#51024 = EDGE_LOOP ( 'NONE', ( #73318, #89134, #19978, #35223 ) ) ;
#51025 = DIRECTION ( 'NONE',  ( 0.000000000000000000, 0.000000000000000000, 1.000000000000000000 ) ) ;
#51026 = CARTESIAN_POINT ( 'NONE',  ( -110.1845341748307874, -289.9771885154749498, -276.6289519616127563 ) ) ;
#51027 = DIRECTION ( 'NONE',  ( 8.299690114939509805E-17, -0.7353190267777791611, 0.6777211291221335587 ) ) ;
#51028 = CARTESIAN_POINT ( 'NONE',  ( -37.99251322539671349, -286.9854318925292773, -193.5991700109078408 ) ) ;
#51029 = CARTESIAN_POINT ( 'NONE',  ( -92.05005921254146983, -286.4090924074130839, -314.0302885647153062 ) ) ;
#51030 = CARTESIAN_POINT ( 'NONE',  ( -11.14879584051634076, -293.7778559617395331, -342.5753377799391615 ) ) ;
#51031 = CARTESIAN_POINT ( 'NONE',  ( 38.78916494465794784, -282.9691339289838083, -278.4496375185593706 ) ) ;
#51032 = CARTESIAN_POINT ( 'NONE',  ( -96.57358185941994577, -284.9823984878326542, -227.6714896863678916 ) ) ;
#51033 = CARTESIAN_POINT ( 'NONE',  ( -1.112648095701359141, -278.0826014965762170, -334.5917887401917596 ) ) ;
#51034 = CARTESIAN_POINT ( 'NONE',  ( -50.79178153345812774, -293.2449305763212237, -343.7841532648337761 ) ) ;
#51035 = CARTESIAN_POINT ( 'NONE',  ( 22.15422249566766766, -295.9210824752074132, -314.3862154445993156 ) ) ;
#51036 = CARTESIAN_POINT ( 'NONE',  ( 34.55041386389184055, -274.5410830132706224, -285.1480869662650548 ) ) ;
#51037 = ORIENTED_EDGE ( 'NONE', *, *, #51565, .T. ) ;
#51038 = CARTESIAN_POINT ( 'NONE',  ( 0.000000000000000000, 3.000000000000000000, 9.000000000000001776 ) ) ;
#51039 = CARTESIAN_POINT ( 'NONE',  ( -24.91541006873382713, -294.5646587161193679, -346.3844490381481478 ) ) ;
#51040 = CARTESIAN_POINT ( 'NONE',  ( -28.98771047613502461, -290.8655955160263602, -344.3308756797667343 ) ) ;
#51041 = CARTESIAN_POINT ( 'NONE',  ( -81.68173343236078665, -296.7195798862911715, -332.9995598328504229 ) ) ;
#51042 = CARTESIAN_POINT ( 'NONE',  ( -38.63501986142806288, -286.6869602755991764, -197.2581271832783898 ) ) ;
#51043 = CARTESIAN_POINT ( 'NONE',  ( -95.04187543518484915, -276.9236646183248354, -320.9922347279758696 ) ) ;
#51044 = CARTESIAN_POINT ( 'NONE',  ( -61.55159473342654763, -296.0098837190847689, -343.4044083551847848 ) ) ;
#51045 = CARTESIAN_POINT ( 'NONE',  ( -29.13490488666295164, -287.0889298664189369, -345.7327989286015963 ) ) ;
#51046 = CARTESIAN_POINT ( 'NONE',  ( -111.1939019949068239, -296.6124288744349542, -292.1238771964989951 ) ) ;
#51047 = CARTESIAN_POINT ( 'NONE',  ( -65.33899087563729324, -292.0091314203624506, -202.9069649173861194 ) ) ;
#51048 = CARTESIAN_POINT ( 'NONE',  ( 196.2275967971934847, 72.70402042033215650, -11.63057524128066866 ) ) ;
#51049 = CARTESIAN_POINT ( 'NONE',  ( 156.4851178187871312, 1.000000000000000000, -7.000000000000000888 ) ) ;
#51050 = CARTESIAN_POINT ( 'NONE',  ( 202.8072765148675103, 291.9636416985566143, -68.23872395582101547 ) ) ;
#51051 = CARTESIAN_POINT ( 'NONE',  ( -40.80456282695320169, -287.5295882308791988, -194.0813409114329602 ) ) ;
#51052 = CARTESIAN_POINT ( 'NONE',  ( -55.56934967048407970, -283.3380690714490697, -190.3538533559490702 ) ) ;
#51053 = ORIENTED_EDGE ( 'NONE', *, *, #34764, .T. ) ;
#51054 = CARTESIAN_POINT ( 'NONE',  ( -104.7003003547445417, -278.3818676540418551, -233.2648680129257457 ) ) ;
#51055 = CARTESIAN_POINT ( 'NONE',  ( -88.15549523683108646, -285.7650690500026940, -325.3681939281526638 ) ) ;
#51056 = CARTESIAN_POINT ( 'NONE',  ( -108.7587668370613301, -282.7786464165852180, -297.6786500538951259 ) ) ;
#51057 = CARTESIAN_POINT ( 'NONE',  ( -56.45853184964177984, -287.3801278799319903, -342.3581729291028068 ) ) ;
#51058 = CARTESIAN_POINT ( 'NONE',  ( 11.91976159537290769, -278.2363651558653146, -327.9251159915700100 ) ) ;
#51059 = CARTESIAN_POINT ( 'NONE',  ( -35.15172674704856348, -298.5726437816636576, -197.2993898346907429 ) ) ;
#51060 = EDGE_CURVE ( 'NONE', #92061, #92001, #3796, .T. ) ;
#51061 = CARTESIAN_POINT ( 'NONE',  ( -63.76181381131007697, -294.0886479231024282, -338.9950778410869816 ) ) ;
#51062 = CARTESIAN_POINT ( 'NONE',  ( 6.119804185979267785, -281.2766240399240019, -206.9228769201384353 ) ) ;
#51064 = CARTESIAN_POINT ( 'NONE',  ( -108.3867763994746127, -278.1276044459845025, -253.1422386305939369 ) ) ;
#51063 = CARTESIAN_POINT ( 'NONE',  ( -36.46617441205170707, -277.0409132872975988, -343.3683347522843405 ) ) ;
#51065 = CARTESIAN_POINT ( 'NONE',  ( 36.98224627476096060, -276.3942870809443093, -251.4549416924350851 ) ) ;
#51066 = CARTESIAN_POINT ( 'NONE',  ( -11.98142676218160574, -275.6501241513911964, -342.7932557989564089 ) ) ;
#51067 = CARTESIAN_POINT ( 'NONE',  ( -71.48678950961217993, -195.9896530788094253, -360.3036401658151817 ) ) ;
#51068 = CARTESIAN_POINT ( 'NONE',  ( -77.13658905977014513, -275.5849227701816062, -333.9932805167524634 ) ) ;
#51069 = EDGE_CURVE ( 'NONE', #26346, #2466, #57404, .T. ) ;
#51070 = CARTESIAN_POINT ( 'NONE',  ( -112.6201739033270997, -297.8084888185636601, -283.7653447835110114 ) ) ;
#51071 = LINE ( 'NONE', #66686, #41273 ) ;
#51072 = DIRECTION ( 'NONE',  ( -0.000000000000000000, -0.000000000000000000, 1.000000000000000000 ) ) ;
#51073 = CARTESIAN_POINT ( 'NONE',  ( -42.71042936018697134, -287.0625339764642376, -197.2361771341240910 ) ) ;
#51074 = CARTESIAN_POINT ( 'NONE',  ( -15.72349531265234823, -288.0880960616462403, -197.4598595427160035 ) ) ;
#51075 = CARTESIAN_POINT ( 'NONE',  ( -49.43022779396378041, -285.2426830650466627, -198.2140551011335674 ) ) ;
#51076 = CARTESIAN_POINT ( 'NONE',  ( -83.92712333052770646, -277.8001142140955722, -213.0565520483397961 ) ) ;
#51077 = CARTESIAN_POINT ( 'NONE',  ( -108.5463921900058892, -286.6878300636243466, -249.1884143319376221 ) ) ;
#51078 = CARTESIAN_POINT ( 'NONE',  ( -109.5628939842647327, -277.2243763405871846, -255.6415385081728857 ) ) ;
#51079 = CARTESIAN_POINT ( 'NONE',  ( -21.53071167818425735, -278.1604891875282419, -342.1857161561738394 ) ) ;
#51080 = CARTESIAN_POINT ( 'NONE',  ( 31.17385357820676006, -275.7064907657397157, -244.9917005299174946 ) ) ;
#51081 = CARTESIAN_POINT ( 'NONE',  ( 36.39799149660461097, -286.6089816499899143, -291.1568765219308261 ) ) ;
#51082 = CARTESIAN_POINT ( 'NONE',  ( 39.54879918530137672, -282.3494671859059508, -269.9209668513495330 ) ) ;
#51083 = CARTESIAN_POINT ( 'NONE',  ( 38.60810804908933846, -282.1994100333202482, -282.7379071919000353 ) ) ;
#51084 = ORIENTED_EDGE ( 'NONE', *, *, #57774, .T. ) ;
#51085 = ORIENTED_EDGE ( 'NONE', *, *, #72094, .F. ) ;
#51086 = FACE_BOUND ( 'NONE', #20335, .T. ) ;
#51087 = CARTESIAN_POINT ( 'NONE',  ( 20.56060653380401604, -290.0815428073241833, -319.2244822390707668 ) ) ;
#51088 = CARTESIAN_POINT ( 'NONE',  ( -74.20449915820179854, -288.2163608899847986, -337.4166041082575589 ) ) ;
#51089 = CARTESIAN_POINT ( 'NONE',  ( -16.70375795726870294, -296.3901479883312504, -343.7677806324035714 ) ) ;
#51090 = CARTESIAN_POINT ( 'NONE',  ( 51.92734036832234779, -298.3949240948066972, -197.2122406934001617 ) ) ;
#51091 = CARTESIAN_POINT ( 'NONE',  ( -56.15580824353236267, -291.1646794034347181, -195.7452483575337112 ) ) ;
#51092 = CARTESIAN_POINT ( 'NONE',  ( 28.28430794893779776, -285.5795050992591655, -236.7234117582345334 ) ) ;
#51093 = CARTESIAN_POINT ( 'NONE',  ( -47.10627101322353383, -290.1662694622758067, -196.9947280787739601 ) ) ;
#51094 = TOROIDAL_SURFACE ( 'NONE', #43590, 2.103083949679977582, 3.000000000000000000 ) ;
#51095 = CARTESIAN_POINT ( 'NONE',  ( 14.37398244000208081, -289.5099409172001970, -322.4439239837490732 ) ) ;
#51096 = CARTESIAN_POINT ( 'NONE',  ( -69.91165696735023971, -300.1233781216987495, -202.8022627189028810 ) ) ;
#51097 = CARTESIAN_POINT ( 'NONE',  ( -18.20929502808394673, -290.8057285049814027, -342.8797481467224202 ) ) ;
#51098 = CARTESIAN_POINT ( 'NONE',  ( -5.142081507021530662, -286.6291991882284265, -338.2958874063808139 ) ) ;
#51099 = CARTESIAN_POINT ( 'NONE',  ( -98.31313142189650023, -291.9579171654473839, -314.0576789665474280 ) ) ;
#51100 = CARTESIAN_POINT ( 'NONE',  ( -107.6143234067178440, -285.2209477664488304, -291.0254421079523581 ) ) ;
#51101 = CARTESIAN_POINT ( 'NONE',  ( -55.76469888281305032, -293.8158264128625774, -197.4334616761163375 ) ) ;
#51102 = CARTESIAN_POINT ( 'NONE',  ( 196.2452211277167748, 71.67373103464963435, -13.59235650557799779 ) ) ;
#51103 = APPLICATION_CONTEXT ( 'automotive_design' ) ;
#51104 = DIRECTION ( 'NONE',  ( -1.110223024625156540E-15, 0.000000000000000000, 1.000000000000000000 ) ) ;
#51105 = CARTESIAN_POINT ( 'NONE',  ( -110.2338880845598936, -274.7787865676199885, -251.0526395367190844 ) ) ;
#51106 = CARTESIAN_POINT ( 'NONE',  ( 33.80478422507519554, -280.9744704911740882, -287.4666434848887775 ) ) ;
#51107 = CARTESIAN_POINT ( 'NONE',  ( -38.95290268266872147, -281.0721757505338019, -345.3566466280354916 ) ) ;
#51108 = CARTESIAN_POINT ( 'NONE',  ( -84.09507087535742187, -294.8732843839204065, -331.4059196420202511 ) ) ;
#51109 = CARTESIAN_POINT ( 'NONE',  ( 32.07639937149461673, -273.4543652466414869, -244.6881463194227422 ) ) ;
#51110 = CARTESIAN_POINT ( 'NONE',  ( -57.00361218945658237, -275.3874260833529775, -342.2110595009923486 ) ) ;
#51111 = CARTESIAN_POINT ( 'NONE',  ( -110.8773036433820920, -297.8525773782296255, -271.4872749191334833 ) ) ;
#51112 = DIRECTION ( 'NONE',  ( 0.000000000000000000, 0.000000000000000000, 1.000000000000000000 ) ) ;
#51113 = CARTESIAN_POINT ( 'NONE',  ( -99.19686102394565808, -294.1986119463037426, -314.5849452550909859 ) ) ;
#51114 = CARTESIAN_POINT ( 'NONE',  ( 1.899267874983875171, -295.9415172121264277, -332.6751630027971487 ) ) ;
#51115 = CARTESIAN_POINT ( 'NONE',  ( 186.6539576904058890, 293.9636489450775230, -9.103929867429224387 ) ) ;
#51116 = CARTESIAN_POINT ( 'NONE',  ( -28.86714660428147283, -295.7449464245688091, -343.0812458012580350 ) ) ;
#51117 = CARTESIAN_POINT ( 'NONE',  ( 201.6445761222582007, 62.92800856396192444, 6.999999999998341771 ) ) ;
#51119 = CARTESIAN_POINT ( 'NONE',  ( -92.74440614636914404, -297.2290146111806166, -222.8072700936497483 ) ) ;
#51118 = CARTESIAN_POINT ( 'NONE',  ( -109.1265359876504704, -282.2773268986495623, -293.3241030871791963 ) ) ;
#51120 = CARTESIAN_POINT ( 'NONE',  ( -102.9180786539602792, -284.0246746958243875, -310.7187514541928408 ) ) ;
#51121 = CARTESIAN_POINT ( 'NONE',  ( 24.76100957757790511, -284.0519538684512213, -313.4253478896217757 ) ) ;
#51122 = AXIS2_PLACEMENT_3D ( 'NONE', #88988, #65874, #88055 ) ;
#51123 = CARTESIAN_POINT ( 'NONE',  ( 22.38604925080206343, -287.8707831529797545, -318.9446070580681862 ) ) ;
#51124 = CARTESIAN_POINT ( 'NONE',  ( -2.767129051994785538, -290.5102143224892188, -203.9937505166963376 ) ) ;
#51125 = EDGE_CURVE ( 'NONE', #40555, #38261, #93665, .T. ) ;
#51126 = CARTESIAN_POINT ( 'NONE',  ( -111.5723750715653324, -277.9989432986553766, -250.4617769120534092 ) ) ;
#51127 = EDGE_CURVE ( 'NONE', #13434, #32648, #24111, .T. ) ;
#51128 = CARTESIAN_POINT ( 'NONE',  ( 35.78497577281001440, -278.8380690714489560, -253.7030783399848985 ) ) ;
#51129 = CARTESIAN_POINT ( 'NONE',  ( -48.18343439339133027, -262.5501068226379289, -494.5729214566428027 ) ) ;
#51130 = CARTESIAN_POINT ( 'NONE',  ( 34.96124105455808717, -286.1776501377624413, -257.4481184333653800 ) ) ;
#51132 = CARTESIAN_POINT ( 'NONE',  ( 175.2296996224750103, 160.0000000000000568, 0.000000000000000000 ) ) ;
#51131 = CARTESIAN_POINT ( 'NONE',  ( -104.8902311795035445, -289.0011005629708052, -306.6748682947091993 ) ) ;
#51133 = CARTESIAN_POINT ( 'NONE',  ( 208.4306832106270804, -198.2391364535880598, 7.500000000000012434 ) ) ;
#51134 = CARTESIAN_POINT ( 'NONE',  ( -97.54704456335279872, -298.7417860848294140, -227.6790735431856945 ) ) ;
#51135 = CARTESIAN_POINT ( 'NONE',  ( -112.4828521586852048, -279.8016968538092897, -284.3042359674442423 ) ) ;
#51137 = CARTESIAN_POINT ( 'NONE',  ( 32.75607713922430975, -280.9483591675636944, -249.9065559243356631 ) ) ;
#51136 = CARTESIAN_POINT ( 'NONE',  ( -96.04872799750523882, -295.2192699766738428, -223.1182170727707899 ) ) ;
#51138 = CARTESIAN_POINT ( 'NONE',  ( 6.615742610128464207, -294.6396333603258313, -333.6458882556190702 ) ) ;
#51139 = CARTESIAN_POINT ( 'NONE',  ( 22.73174121994457408, -285.0091164189876736, -224.5087289828665291 ) ) ;
#51140 = CARTESIAN_POINT ( 'NONE',  ( -111.3220646130688323, -280.3940606587116804, -282.6861462060236363 ) ) ;
#51141 = CARTESIAN_POINT ( 'NONE',  ( -75.32245294360193100, -296.5914191786604306, -207.6854697250635979 ) ) ;
#51142 = ORIENTED_EDGE ( 'NONE', *, *, #85122, .T. ) ;
#51143 = CARTESIAN_POINT ( 'NONE',  ( 18.85951277953860128, -284.2174640594336097, -319.4861673201651229 ) ) ;
#51144 = DIRECTION ( 'NONE',  ( -0.000000000000000000, -0.000000000000000000, -1.000000000000000000 ) ) ;
#51145 = CARTESIAN_POINT ( 'NONE',  ( 21.31550574532286291, -290.4094976428776249, -223.6242672951989618 ) ) ;
#51146 = CARTESIAN_POINT ( 'NONE',  ( 4.783199877688997681, -273.8022978453109317, -206.0356185755451293 ) ) ;
#51147 = CARTESIAN_POINT ( 'NONE',  ( -104.0485805477667043, -289.9848100426735868, -300.1371361625018608 ) ) ;
#51148 = CARTESIAN_POINT ( 'NONE',  ( 3.068151096329007732, -282.1253954055514441, -208.6739960586112090 ) ) ;
#51149 = CARTESIAN_POINT ( 'NONE',  ( -46.29582928246363593, -275.5367938077609438, -197.1063298430928228 ) ) ;
#51150 = CARTESIAN_POINT ( 'NONE',  ( 0.4890743226171061497, -284.1569440888880536, -336.5220397580550298 ) ) ;
#51151 = CARTESIAN_POINT ( 'NONE',  ( 19.99577512790231637, -279.7032604210278919, -224.5403318966637869 ) ) ;
#51152 = CARTESIAN_POINT ( 'NONE',  ( -108.1440564277788496, -280.2301735133773377, -295.2576465013926281 ) ) ;
#51153 = CARTESIAN_POINT ( 'NONE',  ( -97.81438414798213898, -273.3563534167021203, -222.6950452267130345 ) ) ;
#51154 = CARTESIAN_POINT ( 'NONE',  ( -41.19064645770409072, -273.8384209096070663, -193.4051156341953401 ) ) ;
#51155 = CARTESIAN_POINT ( 'NONE',  ( 28.44185374688795420, -295.9390054384124937, -305.3115145383727622 ) ) ;
#51156 = CYLINDRICAL_SURFACE ( 'NONE', #36031, 2.000000000000001776 ) ;
#51157 = CARTESIAN_POINT ( 'NONE',  ( -16.86387529450534828, -292.9301606725258580, -343.3603985373750334 ) ) ;
#51158 = CARTESIAN_POINT ( 'NONE',  ( -24.57952629240084264, -273.7269398815510044, -198.3712105745552492 ) ) ;
#51159 = CARTESIAN_POINT ( 'NONE',  ( 12.80811989866018230, -294.2574092503788847, -212.8484819595923909 ) ) ;
#51161 = CARTESIAN_POINT ( 'NONE',  ( -66.87660097890348254, -292.8786753979895252, -199.6808636619570052 ) ) ;
#51160 = CARTESIAN_POINT ( 'NONE',  ( 31.95455697924148097, -283.6233781216988064, -236.9535640164627637 ) ) ;
#51162 = CARTESIAN_POINT ( 'NONE',  ( -85.85465383972889697, -291.7255569108441478, -327.4077514720813156 ) ) ;
#51163 = CARTESIAN_POINT ( 'NONE',  ( -18.58133240007699882, -274.8097791813563049, -342.8047307183484236 ) ) ;
#51164 = CARTESIAN_POINT ( 'NONE',  ( -15.94400305952446395, -278.6935536367594750, -341.7135144517626486 ) ) ;
#51165 = CARTESIAN_POINT ( 'NONE',  ( -7.431721254557253964, -292.7367500436675414, -338.5417221535161616 ) ) ;
#51166 = CARTESIAN_POINT ( 'NONE',  ( 37.21439624702472315, -283.5848084734714121, -283.9126926997171836 ) ) ;
#51167 = EDGE_LOOP ( 'NONE', ( #42680, #68799, #3681, #63335 ) ) ;
#51168 = CARTESIAN_POINT ( 'NONE',  ( -90.75982214474217358, -283.5031429853315217, -320.1465749655091031 ) ) ;
#51169 = CARTESIAN_POINT ( 'NONE',  ( 20.82264648940808627, -281.9542099770382606, -220.3571436467458682 ) ) ;
#51170 = CARTESIAN_POINT ( 'NONE',  ( 21.29611585587976919, -281.0142438009466446, -319.6522455459171965 ) ) ;
#51171 = CARTESIAN_POINT ( 'NONE',  ( -6.657707155575216973, -277.6003056939377416, -340.7408971148583419 ) ) ;
#51172 = CARTESIAN_POINT ( 'NONE',  ( 0.000000000000000000, 0.000000000000000000, 0.000000000000000000 ) ) ;
#51173 = CARTESIAN_POINT ( 'NONE',  ( 35.40752252100414665, -277.3643215082681195, -293.3884573108048244 ) ) ;
#51174 = CARTESIAN_POINT ( 'NONE',  ( -37.30987171927208124, -291.5519495502701375, -340.3611179825599606 ) ) ;
#51175 = ORIENTED_EDGE ( 'NONE', *, *, #50389, .F. ) ;
#51176 = CARTESIAN_POINT ( 'NONE',  ( -97.72529541505058148, -299.1593410108936268, -225.8554737236963206 ) ) ;
#51177 = CARTESIAN_POINT ( 'NONE',  ( -46.12613884528399666, -275.1840826853351132, -344.5389969121603144 ) ) ;
#51178 = CARTESIAN_POINT ( 'NONE',  ( -112.1779767200939233, -292.4792220396324751, -257.1889609516422297 ) ) ;
#51179 = CARTESIAN_POINT ( 'NONE',  ( 35.39763592381030577, -292.7984871376878004, -262.5993243562664361 ) ) ;
#51180 = CARTESIAN_POINT ( 'NONE',  ( -4.365129471991358479, -288.1367683650125286, -339.8886968637668815 ) ) ;
#51181 = CARTESIAN_POINT ( 'NONE',  ( -23.68628624284178130, -44.55766379199612004, -21.49999999999998579 ) ) ;
#51183 = CARTESIAN_POINT ( 'NONE',  ( -78.84315096917276833, -282.0217828831396218, -331.3862766615405917 ) ) ;
#51182 = CARTESIAN_POINT ( 'NONE',  ( 10.81279845429053843, -292.9762589657690910, -329.7567760583565359 ) ) ;
#51184 = CARTESIAN_POINT ( 'NONE',  ( -45.47463465081332856, -291.0167197691744150, -344.1494697427020242 ) ) ;
#51185 = CARTESIAN_POINT ( 'NONE',  ( -90.14627724528926933, -283.7690935259753360, -218.8837821325069797 ) ) ;
#51186 = CARTESIAN_POINT ( 'NONE',  ( -66.74157205310883967, -284.7607549507834506, -337.7312264360124345 ) ) ;
#51187 = CARTESIAN_POINT ( 'NONE',  ( -26.16693419948606092, -289.8544500578014436, -346.3081048805617002 ) ) ;
#51188 = CARTESIAN_POINT ( 'NONE',  ( 25.18570854657578550, -281.5235480821974647, -232.4700798614151722 ) ) ;
#51189 = CARTESIAN_POINT ( 'NONE',  ( -22.19116521235297057, -293.6571598072058578, -345.4508643481782997 ) ) ;
#51190 = CARTESIAN_POINT ( 'NONE',  ( -31.82813607470581019, -289.7872086811860299, -347.0540191270774244 ) ) ;
#51191 = CARTESIAN_POINT ( 'NONE',  ( 39.29276794509681281, -287.9518246092063691, -262.9569427667189530 ) ) ;
#51192 = CARTESIAN_POINT ( 'NONE',  ( -87.69603675152850997, -285.4913477055930002, -217.5081068317804238 ) ) ;
#51193 = EDGE_LOOP ( 'NONE', ( #64260, #27095, #50331, #48732 ) ) ;
#51194 = CARTESIAN_POINT ( 'NONE',  ( 196.0068564634292159, 26.11245708493671103, 13.37100780525461374 ) ) ;
#51195 = CARTESIAN_POINT ( 'NONE',  ( 25.50067708387251031, -295.9792269590741398, -312.6829930222918961 ) ) ;
#51196 = CARTESIAN_POINT ( 'NONE',  ( -109.8834738408593239, -294.9288911563629085, -294.6713902756424659 ) ) ;
#51197 = CARTESIAN_POINT ( 'NONE',  ( -96.28950371176620138, -277.0035426759324082, -313.8397643539821615 ) ) ;
#51198 = CARTESIAN_POINT ( 'NONE',  ( 53.44637165907408871, -298.5094331931565534, -193.4727354929377441 ) ) ;
#51199 = CARTESIAN_POINT ( 'NONE',  ( -71.26705041534634688, -293.9883632973611043, -335.7952516704156665 ) ) ;
#51200 = CARTESIAN_POINT ( 'NONE',  ( -13.76355686666970080, -276.1225486433998526, -200.2038291762643212 ) ) ;
#51201 = CARTESIAN_POINT ( 'NONE',  ( -106.7483883185292370, -295.1318010299526122, -244.5096044230448058 ) ) ;
#51202 = CARTESIAN_POINT ( 'NONE',  ( 23.26952443796387371, -295.3311244716243777, -311.8433769586935114 ) ) ;
#51203 = CARTESIAN_POINT ( 'NONE',  ( 34.78483564400909955, -294.4586391219061738, -257.1769313256421583 ) ) ;
#51204 = CARTESIAN_POINT ( 'NONE',  ( -43.26782269566163563, -275.6797743861646381, -431.4331960659528704 ) ) ;
#51205 = CARTESIAN_POINT ( 'NONE',  ( -109.4636967734172259, -294.2793639751031378, -291.5831153897665331 ) ) ;
#51206 = CARTESIAN_POINT ( 'NONE',  ( -97.91123680697840825, -275.1561204526838651, -226.0443558784494655 ) ) ;
#51207 = CARTESIAN_POINT ( 'NONE',  ( -34.55708599290608163, -289.9577002517169149, -343.5931953528137797 ) ) ;
#51208 = CARTESIAN_POINT ( 'NONE',  ( -70.93675025342905371, -295.8414667259179396, -335.2092027438978334 ) ) ;
#51209 = CARTESIAN_POINT ( 'NONE',  ( -100.5261445489632024, -281.0841476157992247, -229.2041049313961594 ) ) ;
#51210 = CARTESIAN_POINT ( 'NONE',  ( -50.83609103335521695, -278.5680249251117289, -195.0537499125560430 ) ) ;
#51211 = CARTESIAN_POINT ( 'NONE',  ( 24.28099457999335087, -275.5134893412964061, -316.3606428042467655 ) ) ;
#51212 = CARTESIAN_POINT ( 'NONE',  ( -69.65595943882617291, -281.5607536458534241, -337.4356376623857727 ) ) ;
#51213 = CARTESIAN_POINT ( 'NONE',  ( -38.14086047152152759, -278.4421721935345317, -194.1653060168162028 ) ) ;
#51214 = CARTESIAN_POINT ( 'NONE',  ( -72.87592414889944337, -277.5824163051257187, -204.1094712698206592 ) ) ;
#51215 = CARTESIAN_POINT ( 'NONE',  ( 9.338798127652633951, -297.3333334804277115, -196.8786743985532439 ) ) ;
#51216 = CARTESIAN_POINT ( 'NONE',  ( -25.29944381291146982, -276.2056926635384571, -196.2821725839788769 ) ) ;
#51217 = CIRCLE ( 'NONE', #21027, 4.003189038634634045 ) ;
#51218 = CARTESIAN_POINT ( 'NONE',  ( 153.4656128104947470, 19.61038002238656475, 12.30465931838429228 ) ) ;
#51219 = CARTESIAN_POINT ( 'NONE',  ( -95.14593035939897447, -287.9073109253796474, -318.7244731886689237 ) ) ;
#51220 = CARTESIAN_POINT ( 'NONE',  ( -113.3600532252344095, -290.3988737420636994, -282.6171366018573963 ) ) ;
#51221 = CARTESIAN_POINT ( 'NONE',  ( 32.99699653898910867, -277.2087980014251229, -243.8564735617798078 ) ) ;
#51222 = CARTESIAN_POINT ( 'NONE',  ( -78.49956315542313234, -295.4969896288704376, -207.8003928352211176 ) ) ;
#51223 = ADVANCED_FACE ( 'NONE', ( #73506 ), #46914, .T. ) ;
#51224 = CARTESIAN_POINT ( 'NONE',  ( -78.42747205029628788, -284.7112635484882617, -205.4294757285993853 ) ) ;
#51225 = EDGE_CURVE ( 'NONE', #37664, #14615, #33234, .T. ) ;
#51226 = DIRECTION ( 'NONE',  ( -0.000000000000000000, -1.000000000000000000, -0.000000000000000000 ) ) ;
#51227 = CARTESIAN_POINT ( 'NONE',  ( -65.70949196615140409, -283.6811203973288116, -200.8785762500826877 ) ) ;
#51228 = DIRECTION ( 'NONE',  ( 0.000000000000000000, 0.000000000000000000, 1.000000000000000000 ) ) ;
#51229 = CARTESIAN_POINT ( 'NONE',  ( 35.93213221121447987, -292.2807214703314571, -265.3041903316326398 ) ) ;
#51230 = CARTESIAN_POINT ( 'NONE',  ( -88.52937113728961549, -283.4645782699816436, -216.5960008964246981 ) ) ;
#51231 = FACE_OUTER_BOUND ( 'NONE', #29676, .T. ) ;
#51232 = DIRECTION ( 'NONE',  ( -0.000000000000000000, -1.000000000000000000, 0.000000000000000000 ) ) ;
#51233 = CARTESIAN_POINT ( 'NONE',  ( 36.28297239206418823, -291.7355669292099378, -284.6582592317561762 ) ) ;
#51234 = CARTESIAN_POINT ( 'NONE',  ( -78.79941748305679994, -282.0798711219177903, -334.4233176276492259 ) ) ;
#51235 = CARTESIAN_POINT ( 'NONE',  ( -110.0710376239063066, -279.9878725310821892, -282.9610248752762232 ) ) ;
#51236 = CARTESIAN_POINT ( 'NONE',  ( -113.9437735332358415, -285.7617775967707985, -269.9990855383693429 ) ) ;
#51237 = CARTESIAN_POINT ( 'NONE',  ( -73.55563123900545008, -285.5572424245465868, -206.9624662142850298 ) ) ;
#51238 = CARTESIAN_POINT ( 'NONE',  ( -91.38836361919092610, -279.2651496445404291, -320.3785164674092698 ) ) ;
#51239 = CARTESIAN_POINT ( 'NONE',  ( -110.3204390218664770, -279.4230098878219906, -265.1933915910096289 ) ) ;
#51240 = CARTESIAN_POINT ( 'NONE',  ( -111.5135156720319429, -286.6994352803285437, -258.9029224791194110 ) ) ;
#51241 = ORIENTED_EDGE ( 'NONE', *, *, #56813, .F. ) ;
#51242 = DIRECTION ( 'NONE',  ( 0.9849620900324523864, 0.000000000000000000, -0.1727706028203384037 ) ) ;
#51243 = CARTESIAN_POINT ( 'NONE',  ( -113.9434354656293777, -296.2876553284954184, -278.1825083814383106 ) ) ;
#51244 = CARTESIAN_POINT ( 'NONE',  ( 6.837977664251367216, -290.4280544449424610, -330.5920098815333859 ) ) ;
#51245 = DIRECTION ( 'NONE',  ( -0.000000000000000000, -1.000000000000000000, -0.000000000000000000 ) ) ;
#51246 = CARTESIAN_POINT ( 'NONE',  ( -72.08107566293803359, -282.1233781216987495, -198.2974183793908196 ) ) ;
#51247 = CARTESIAN_POINT ( 'NONE',  ( -61.93543364288468922, -278.6602465554441324, -197.6646250129299744 ) ) ;
#51248 = CARTESIAN_POINT ( 'NONE',  ( 31.47236698863065740, -291.5267467177152980, -237.5113012651123654 ) ) ;
#51249 = CARTESIAN_POINT ( 'NONE',  ( 13.60503044792356775, -288.3012470983588287, -217.0447169430276517 ) ) ;
#51250 = CARTESIAN_POINT ( 'NONE',  ( -111.2916997068601574, -280.2724700465123533, -273.4224205519616930 ) ) ;
#51251 = CARTESIAN_POINT ( 'NONE',  ( 35.82646053970353250, -289.2564825129219912, -292.4299170415991398 ) ) ;
#51252 = CARTESIAN_POINT ( 'NONE',  ( -104.8007342804427253, -286.1190163130639803, -303.2565073990449491 ) ) ;
#51253 = CARTESIAN_POINT ( 'NONE',  ( -112.7932035111290219, -278.5258611049355295, -285.7908604842945692 ) ) ;
#51254 = CARTESIAN_POINT ( 'NONE',  ( -37.11996792456957195, -296.0750594714473891, -195.7134715578960709 ) ) ;
#51255 = CARTESIAN_POINT ( 'NONE',  ( 38.27064004391357344, -291.6316672520829343, -270.3353211111757446 ) ) ;
#51256 = CARTESIAN_POINT ( 'NONE',  ( -77.49070475511013001, -279.3628606267507166, -204.5950748890428770 ) ) ;
#51257 = CARTESIAN_POINT ( 'NONE',  ( -31.26177024751022770, -275.9901474282495997, -196.3624454328090678 ) ) ;
#51258 = CARTESIAN_POINT ( 'NONE',  ( 154.6019620322140327, 19.02489598988758601, 11.88315578648355597 ) ) ;
#51259 = CARTESIAN_POINT ( 'NONE',  ( 31.98288692825981272, -296.4805209788415823, -303.7098442033569654 ) ) ;
#51260 = CARTESIAN_POINT ( 'NONE',  ( 15.34083055876097212, -273.0241809487641262, -215.6023289834772640 ) ) ;
#51261 = PLANE ( 'NONE',  #69673 ) ;
#51262 = CARTESIAN_POINT ( 'NONE',  ( -103.4228329088073082, -278.4819740116267894, -239.0769838463497479 ) ) ;
#51263 = CARTESIAN_POINT ( 'NONE',  ( -20.19995125228745536, -278.0418551492644497, -345.0759160607198055 ) ) ;
#51264 = CARTESIAN_POINT ( 'NONE',  ( 9.380405744046012018, -300.0735365612985106, -196.7602862293037731 ) ) ;
#51265 = CARTESIAN_POINT ( 'NONE',  ( -92.27375911077636772, -282.8731231115476135, -323.9828403407423707 ) ) ;
#51266 = CARTESIAN_POINT ( 'NONE',  ( 21.17220360774945220, -289.9420375074424783, -315.7037947314042299 ) ) ;
#51267 = CARTESIAN_POINT ( 'NONE',  ( -33.39872607132846838, -299.6207851031292648, -194.0534482888731702 ) ) ;
#51268 = CARTESIAN_POINT ( 'NONE',  ( -111.2431119366072352, -298.0133092692187802, -250.0008861325090379 ) ) ;
#51269 = CARTESIAN_POINT ( 'NONE',  ( -5.973799624531089592, -296.6390399610475583, -338.3028816361386362 ) ) ;
#51270 = CARTESIAN_POINT ( 'NONE',  ( -12.95540827744081191, -280.7345018623467467, -341.1644693185671713 ) ) ;
#51271 = CARTESIAN_POINT ( 'NONE',  ( 10.55947360335228602, -272.7372355019858787, -213.0454916812439876 ) ) ;
#51272 = CARTESIAN_POINT ( 'NONE',  ( -73.25418718593287792, -287.1845969734122832, -203.0960214877770795 ) ) ;
#51273 = CARTESIAN_POINT ( 'NONE',  ( -13.19899063299152608, -287.6513335046544739, -339.5807369613722813 ) ) ;
#51274 = CARTESIAN_POINT ( 'NONE',  ( -46.75580690834000563, -155.7037500639930556, -364.9887862212212326 ) ) ;
#51275 = ORIENTED_EDGE ( 'NONE', *, *, #66162, .T. ) ;
#51276 = CARTESIAN_POINT ( 'NONE',  ( -72.91576878434101161, -288.0887723416465178, -338.0004029801337992 ) ) ;
#51277 = CARTESIAN_POINT ( 'NONE',  ( -18.47213173214542792, -288.4691351571925679, -340.9546770565488032 ) ) ;
#51278 = ORIENTED_EDGE ( 'NONE', *, *, #13868, .T. ) ;
#51279 = CARTESIAN_POINT ( 'NONE',  ( -108.7457342867439252, -285.9895661006634668, -242.2352704080417141 ) ) ;
#51280 = CARTESIAN_POINT ( 'NONE',  ( -8.726480681712610377, -277.0004240130094217, -337.5554410759777966 ) ) ;
#51281 = CARTESIAN_POINT ( 'NONE',  ( 27.83593559519302474, -293.0043085922339401, -310.8758121720233021 ) ) ;
#51282 = CARTESIAN_POINT ( 'NONE',  ( 38.15303266288361073, -282.0204279340560447, -255.7372297268021271 ) ) ;
#51283 = CARTESIAN_POINT ( 'NONE',  ( 38.18778090552909532, -283.2093621946389703, -281.2241400026125575 ) ) ;
#51284 = CARTESIAN_POINT ( 'NONE',  ( 0.8615533933342958139, -282.8903013607180128, -337.2063973570359963 ) ) ;
#51286 = CARTESIAN_POINT ( 'NONE',  ( -34.31670010331186660, -280.4244747725265370, -197.3901109744372206 ) ) ;
#51285 = AXIS2_PLACEMENT_3D ( 'NONE', #12600, #34376, #76528 ) ;
#51287 = CARTESIAN_POINT ( 'NONE',  ( -77.71228223721278994, -208.7304540725825746, -357.2837420577297962 ) ) ;
#51288 = CARTESIAN_POINT ( 'NONE',  ( -110.2672532426750394, -280.3355224829630288, -287.2074681069486246 ) ) ;
#51289 = CARTESIAN_POINT ( 'NONE',  ( 152.7083132524945199, 207.2806415074720690, -216.8349236652551895 ) ) ;
#51290 = CARTESIAN_POINT ( 'NONE',  ( -23.05802698232256276, -108.1619730152996510, -359.3355512241282099 ) ) ;
#51291 = CARTESIAN_POINT ( 'NONE',  ( -29.96343797951733734, -273.3450898377187173, -197.5726369257234296 ) ) ;
#51292 = CARTESIAN_POINT ( 'NONE',  ( 38.29559869269915851, -293.2370527439210264, -284.5221967548640123 ) ) ;
#51293 = CARTESIAN_POINT ( 'NONE',  ( -54.63958497508173906, -170.0083358554137760, -360.9089503003181107 ) ) ;
#51295 = CARTESIAN_POINT ( 'NONE',  ( -56.29044453690115546, -287.7001020515376126, -341.7401652616800334 ) ) ;
#51294 = CARTESIAN_POINT ( 'NONE',  ( 4.606858296998139757, -273.2900389422306375, -206.3168755091394075 ) ) ;
#51296 = CARTESIAN_POINT ( 'NONE',  ( -85.25760938254116184, -297.5822589470674870, -327.1289543838508393 ) ) ;
#51297 = CARTESIAN_POINT ( 'NONE',  ( -31.81768368539835024, -290.2963063946691022, -343.6973392395946689 ) ) ;
#51298 = ORIENTED_EDGE ( 'NONE', *, *, #40194, .T. ) ;
#51299 = CARTESIAN_POINT ( 'NONE',  ( -66.82295980787920087, -296.3703552800276384, -341.2531668934860249 ) ) ;
#51300 = CARTESIAN_POINT ( 'NONE',  ( -19.80715333753590812, -286.7760857790582349, -199.4349020232345993 ) ) ;
#51301 = CARTESIAN_POINT ( 'NONE',  ( -64.77660902420062428, -272.6224856830560270, -198.7312219740244643 ) ) ;
#51302 = CARTESIAN_POINT ( 'NONE',  ( 34.30854149943613862, -294.0009565589429030, -242.4580193273854434 ) ) ;
#51303 = CARTESIAN_POINT ( 'NONE',  ( 37.40172060872340865, -294.2735517855292073, -288.6631250977949321 ) ) ;
#51304 = CARTESIAN_POINT ( 'NONE',  ( -81.73072800137975946, -291.5953493553906810, -212.3435988334819911 ) ) ;
#51305 = VERTEX_POINT ( 'NONE', #3378 ) ;
#51306 = EDGE_CURVE ( 'NONE', #13595, #35945, #10514, .T. ) ;
#51307 = CARTESIAN_POINT ( 'NONE',  ( -106.7643302014827924, -274.8610345231431324, -240.3989706573248384 ) ) ;
#51308 = CARTESIAN_POINT ( 'NONE',  ( 39.30990417282686877, -274.3574070850378348, -271.1827802559762972 ) ) ;
#51309 = ORIENTED_EDGE ( 'NONE', *, *, #28273, .T. ) ;
#51310 = CARTESIAN_POINT ( 'NONE',  ( -97.64475288401712305, -278.6997196782659785, -222.5796494837631201 ) ) ;
#51311 = CARTESIAN_POINT ( 'NONE',  ( -19.05388863936206434, -272.6911939619357099, -198.8098863554541254 ) ) ;
#51312 = CARTESIAN_POINT ( 'NONE',  ( -72.06623429421867399, -274.6615927930545240, -205.7411494700859578 ) ) ;
#51313 = CARTESIAN_POINT ( 'NONE',  ( -19.22497150002561028, -275.2321654090210927, -199.3494330304375239 ) ) ;
#51314 = CARTESIAN_POINT ( 'NONE',  ( 18.63627104344689300, -300.3420462640792721, -194.1461562402953689 ) ) ;
#51315 = CARTESIAN_POINT ( 'NONE',  ( 21.34383611093550925, -274.2198598528069056, -317.6511144384777481 ) ) ;
#51316 = CARTESIAN_POINT ( 'NONE',  ( -82.41615070157540401, -296.3374367231871815, -327.9772502772240159 ) ) ;
#51317 = CARTESIAN_POINT ( 'NONE',  ( -9.020755267232376085, -293.2490940668136545, -338.2961025804175961 ) ) ;
#51318 = DIRECTION ( 'NONE',  ( -0.000000000000000000, -0.000000000000000000, -1.000000000000000000 ) ) ;
#51319 = CARTESIAN_POINT ( 'NONE',  ( -11.88062928749293157, -277.2218893912382782, -343.0204507072509728 ) ) ;
#51320 = CARTESIAN_POINT ( 'NONE',  ( -27.29227955308186537, -274.3499687997675665, -198.0052463807687957 ) ) ;
#51321 = CARTESIAN_POINT ( 'NONE',  ( -113.8621955474651060, -283.2060724927833348, -272.8165877493603375 ) ) ;
#51322 = CARTESIAN_POINT ( 'NONE',  ( -67.46745545333388350, -297.4465505707994453, -339.2266920765391092 ) ) ;
#51323 = DIRECTION ( 'NONE',  ( 0.000000000000000000, 1.000000000000000000, 0.000000000000000000 ) ) ;
#51324 = CARTESIAN_POINT ( 'NONE',  ( -2.099643807327661538, -285.7282144306698228, -206.1903179535610207 ) ) ;
#51325 = EDGE_CURVE ( 'NONE', #89945, #14641, #91415, .T. ) ;
#51326 = CARTESIAN_POINT ( 'NONE',  ( -111.3638953955564546, -276.8246514181016096, -267.8518529840685005 ) ) ;
#51327 = CARTESIAN_POINT ( 'NONE',  ( -109.6254634277432700, -276.9454204025141735, -284.2275108900748251 ) ) ;
#51328 = CARTESIAN_POINT ( 'NONE',  ( -109.5792553573367343, -286.2923252711419764, -290.5759471552039486 ) ) ;
#51329 = CARTESIAN_POINT ( 'NONE',  ( -8.830680336366494743, -275.6385956928988890, -202.6737006584762071 ) ) ;
#51330 = DIRECTION ( 'NONE',  ( 1.000000000000000000, 0.000000000000000000, 0.000000000000000000 ) ) ;
#51331 = CARTESIAN_POINT ( 'NONE',  ( 34.97723848205466624, -273.6447393864390847, -246.1860825442317662 ) ) ;
#51332 = CARTESIAN_POINT ( 'NONE',  ( -61.48350515421354601, -281.7395822199710551, -199.1219377857263737 ) ) ;
#51333 = ADVANCED_FACE ( 'NONE', ( #11886 ), #6023, .T. ) ;
#51334 = LINE ( 'NONE', #23405, #52833 ) ;
#51335 = CARTESIAN_POINT ( 'NONE',  ( 22.70197244248242896, -288.8488033283720142, -224.4697524299036502 ) ) ;
#51336 = CARTESIAN_POINT ( 'NONE',  ( 27.32275329823826837, -292.0609984471067264, -308.4552361473316182 ) ) ;
#51337 = CARTESIAN_POINT ( 'NONE',  ( 160.5350683151633291, 250.0000000000000568, 20.22542485937379908 ) ) ;
#51338 = CARTESIAN_POINT ( 'NONE',  ( -58.00193527136787708, -296.5741332006574567, -199.9318258683461806 ) ) ;
#51339 = CARTESIAN_POINT ( 'NONE',  ( -63.20931109326946284, -289.8511557346079712, -200.7785613824553650 ) ) ;
#51340 = CARTESIAN_POINT ( 'NONE',  ( 168.1488725781630649, 234.1813984995739588, -193.4213935641190858 ) ) ;
#51341 = LINE ( 'NONE', #1624, #64117 ) ;
#51342 = CARTESIAN_POINT ( 'NONE',  ( -74.11037536823270955, -288.0114460422887532, -337.2398715936250824 ) ) ;
#51343 = CARTESIAN_POINT ( 'NONE',  ( 12.47151682149915786, -283.9442536367162120, -324.8137013068803185 ) ) ;
#51344 = CARTESIAN_POINT ( 'NONE',  ( -32.35029913124321865, -284.3541113851138107, -194.5255695087189167 ) ) ;
#51345 = EDGE_CURVE ( 'NONE', #30942, #56563, #16200, .T. ) ;
#51346 = CARTESIAN_POINT ( 'NONE',  ( 1.427036243123854575, -283.9487498538712771, -332.9694892035441853 ) ) ;
#51347 = CARTESIAN_POINT ( 'NONE',  ( -110.4710336452073989, -285.3835324466729730, -268.1926379186728582 ) ) ;
#51348 = CARTESIAN_POINT ( 'NONE',  ( -99.31326752228548571, -291.9534794869913412, -313.2322229163359566 ) ) ;
#51349 = AXIS2_PLACEMENT_3D ( 'NONE', #70832, #4547, #11651 ) ;
#51350 = CARTESIAN_POINT ( 'NONE',  ( -76.42564679772937097, -273.8780621880021613, -203.9806774624228183 ) ) ;
#51351 = CARTESIAN_POINT ( 'NONE',  ( -64.94420504085373125, -287.4896187115740531, -340.7542856627702577 ) ) ;
#51352 = CARTESIAN_POINT ( 'NONE',  ( 39.62341770031462573, -275.5982112438683771, -274.0439643318902654 ) ) ;
#51354 = CARTESIAN_POINT ( 'NONE',  ( -8.574200426926870122, -296.6537085379361542, -339.2537505169716496 ) ) ;
#51353 = AXIS2_PLACEMENT_3D ( 'NONE', #50417, #79322, #20138 ) ;
#51355 = CARTESIAN_POINT ( 'NONE',  ( -39.58036566374939724, -229.5268262511776527, 21.50000000000000000 ) ) ;
#51356 = CARTESIAN_POINT ( 'NONE',  ( 21.31550574532285580, -296.6948066931273615, -317.0979686699210447 ) ) ;
#51357 = CARTESIAN_POINT ( 'NONE',  ( -38.91229977634652215, -281.7570514290203505, -343.8500613152575056 ) ) ;
#51358 = CARTESIAN_POINT ( 'NONE',  ( -97.35543649558452728, -275.9343644715334563, -315.6412824194929385 ) ) ;
#51359 = CARTESIAN_POINT ( 'NONE',  ( -78.45158725841787373, -271.9893862814429895, -206.0751558145414322 ) ) ;
#51360 = CARTESIAN_POINT ( 'NONE',  ( 22.36887989861714843, -274.3126577192658146, -228.1667141005777353 ) ) ;
#51361 = CARTESIAN_POINT ( 'NONE',  ( -7.002322054124368478, -293.9778007656896079, -203.2028728277592506 ) ) ;
#51362 = CARTESIAN_POINT ( 'NONE',  ( 33.34695230240954800, -294.7460569882038612, -289.5536156726855666 ) ) ;
#51363 = CARTESIAN_POINT ( 'NONE',  ( -75.25822012815351059, -287.2993804090584149, -206.7976731066611933 ) ) ;
#51364 = CARTESIAN_POINT ( 'NONE',  ( 36.84547423152254453, -294.7467286616699766, -252.0616793162862450 ) ) ;
#51365 = CARTESIAN_POINT ( 'NONE',  ( 32.97001352374171290, -295.2554385341416037, -300.6539121235078937 ) ) ;
#51366 = CARTESIAN_POINT ( 'NONE',  ( -90.40869541044028779, -295.6627419143641191, -320.5626925475636426 ) ) ;
#51367 = CARTESIAN_POINT ( 'NONE',  ( -64.52259417479709214, -291.4069716192421993, -340.3181356888530900 ) ) ;
#51368 = CARTESIAN_POINT ( 'NONE',  ( -63.91002463949956081, -283.5559343855917973, -342.6323026771391937 ) ) ;
#51369 = CARTESIAN_POINT ( 'NONE',  ( -98.55485888375768866, -271.2949951125382313, -225.6282772434913682 ) ) ;
#51370 = CARTESIAN_POINT ( 'NONE',  ( 7.545653922764927302, -286.4788797298362510, -207.7324745035944318 ) ) ;
#51371 = CARTESIAN_POINT ( 'NONE',  ( -108.6812842002432404, -280.2454704615338414, -292.5001271597886330 ) ) ;
#51372 = CARTESIAN_POINT ( 'NONE',  ( -72.55108138684782659, -284.3699796257046728, -205.9462821791904048 ) ) ;
#51373 = CARTESIAN_POINT ( 'NONE',  ( 19.05180765752198369, -286.2390077329460496, -319.8251025343561764 ) ) ;
#51374 = CARTESIAN_POINT ( 'NONE',  ( -14.57596635432840237, -278.4835867449974671, -198.0425159834175588 ) ) ;
#51375 = CARTESIAN_POINT ( 'NONE',  ( -114.4693872376281121, -273.8646567567205921, -270.3778293100139649 ) ) ;
#51376 = CARTESIAN_POINT ( 'NONE',  ( -71.20117712068562810, -285.1000708925562890, -205.6191357793204304 ) ) ;
#51377 = CARTESIAN_POINT ( 'NONE',  ( 36.10240885156724744, -283.0338500426178143, -292.3146140444306411 ) ) ;
#51378 = CARTESIAN_POINT ( 'NONE',  ( -93.42910324097664443, -288.8933169988201257, -322.8497945501792401 ) ) ;
#51379 = CARTESIAN_POINT ( 'NONE',  ( 0.6658735846956594928, -278.1547510787144688, -336.4653906778946180 ) ) ;
#51380 = CARTESIAN_POINT ( 'NONE',  ( -38.52045723407346145, -278.3818106649574702, -346.8588879259321516 ) ) ;
#51381 = CARTESIAN_POINT ( 'NONE',  ( -32.96089309463820882, -279.9421988014126441, -197.4926849388189680 ) ) ;
#51382 = CARTESIAN_POINT ( 'NONE',  ( -62.60966605852549804, -275.7015885356250351, -200.1231175860255860 ) ) ;
#51383 = CARTESIAN_POINT ( 'NONE',  ( 39.22612934283546338, -293.4441570845385741, -261.7259186998205678 ) ) ;
#51384 = CARTESIAN_POINT ( 'NONE',  ( -59.19420209856912152, -287.3563384424054448, -341.7895882359574102 ) ) ;
#51385 = CARTESIAN_POINT ( 'NONE',  ( -4.962778673954555408, -294.0715167717559666, -201.3825280875441308 ) ) ;
#51386 = CARTESIAN_POINT ( 'NONE',  ( 33.74243774670213725, -292.7080384216546918, -288.2851637620581187 ) ) ;
#51387 = CARTESIAN_POINT ( 'NONE',  ( -34.30456222466462890, -294.6796352118220170, -343.3190735473191921 ) ) ;
#51388 = CARTESIAN_POINT ( 'NONE',  ( -114.0806652775742265, -291.6207988044860144, -271.2389971882222994 ) ) ;
#51389 = CARTESIAN_POINT ( 'NONE',  ( 30.11236519062958905, -281.8261398450110846, -242.1859207362689119 ) ) ;
#51390 = CARTESIAN_POINT ( 'NONE',  ( -83.42922628208066271, -272.4967088667843882, -208.9043682662539254 ) ) ;
#51391 = CARTESIAN_POINT ( 'NONE',  ( -9.592366059720150773, -289.3503335277848123, -342.0778332262464119 ) ) ;
#51392 = CARTESIAN_POINT ( 'NONE',  ( -16.50465898389557751, -280.9254217157837843, -343.2586523003407137 ) ) ;
#51393 = B_SPLINE_CURVE_WITH_KNOTS ( 'NONE', 3,
 ( #41137, #55394, #84246, #62987, #10874, #34084 ),
 .UNSPECIFIED., .F., .F.,
 ( 4, 2, 4 ),
 ( 0.000000000000000000, 0.001526582415388715898, 0.003053164830777431796 ),
 .UNSPECIFIED. ) ;
#51394 = CARTESIAN_POINT ( 'NONE',  ( -23.31162333636806494, -289.2108809321733247, -346.1047236308979791 ) ) ;
#51395 = CARTESIAN_POINT ( 'NONE',  ( -54.76549701512190182, -286.1553782475880325, -199.3968956021237204 ) ) ;
#51396 = DIRECTION ( 'NONE',  ( 0.000000000000000000, 0.000000000000000000, 1.000000000000000000 ) ) ;
#51397 = CARTESIAN_POINT ( 'NONE',  ( -23.56101253494735204, -107.7048510163219390, -360.7984423213250693 ) ) ;
#51398 = CARTESIAN_POINT ( 'NONE',  ( 84.33524000671648935, 81.64880898236285134, -298.7293534775860735 ) ) ;
#51399 = CARTESIAN_POINT ( 'NONE',  ( -67.36322160390778890, -278.8452327614540422, -203.6293444107159587 ) ) ;
#51400 = CARTESIAN_POINT ( 'NONE',  ( -81.01450109818662781, -276.5816164338935437, -329.2416115957188367 ) ) ;
#51401 = CARTESIAN_POINT ( 'NONE',  ( -52.53729328442921798, -273.5294786642951408, -194.8425405212830412 ) ) ;
#51402 = CARTESIAN_POINT ( 'NONE',  ( 180.9896740030162334, 251.1209438834910941, -164.8178949726211044 ) ) ;
#51403 = CARTESIAN_POINT ( 'NONE',  ( -101.3873539498802785, -277.6795321963437004, -228.5909497609535777 ) ) ;
#51404 = CARTESIAN_POINT ( 'NONE',  ( -67.24105069211334751, -281.4662213769327082, -338.7699945286641992 ) ) ;
#51405 = CARTESIAN_POINT ( 'NONE',  ( -22.27624258869237295, -296.6218995080958507, -344.8393429914403896 ) ) ;
#51406 = CARTESIAN_POINT ( 'NONE',  ( -66.59446684659742743, -292.1506748908980740, -203.4114049053566191 ) ) ;
#51407 = CARTESIAN_POINT ( 'NONE',  ( -71.41618139399894005, -288.1968084978206548, -335.4919496959481080 ) ) ;
#51408 = CARTESIAN_POINT ( 'NONE',  ( -64.87134762020566825, -274.3532910164384475, -198.5456182762580397 ) ) ;
#51409 = CARTESIAN_POINT ( 'NONE',  ( -77.51374711841455678, -297.6634811330434331, -209.3478787528440535 ) ) ;
#51410 = VERTEX_POINT ( 'NONE', #25617 ) ;
#51411 = DIRECTION ( 'NONE',  ( 1.000000000000000000, 0.000000000000000000, 0.000000000000000000 ) ) ;
#51412 = CARTESIAN_POINT ( 'NONE',  ( -45.14935909155659743, -281.8742948270440820, -195.1535817487443580 ) ) ;
#51413 = CIRCLE ( 'NONE', #8, 4.025000000000000355 ) ;
#51414 = CARTESIAN_POINT ( 'NONE',  ( -22.14369121652733696, -281.3309695277396827, -198.5926110428148093 ) ) ;
#51415 = CARTESIAN_POINT ( 'NONE',  ( -92.58171691235297374, -279.5895982078021689, -322.6143171171322592 ) ) ;
#51416 = AXIS2_PLACEMENT_3D ( 'NONE', #58208, #7073, #35490 ) ;
#51417 = CARTESIAN_POINT ( 'NONE',  ( 35.75544495413252832, -280.5517729176612534, -265.8649164330307713 ) ) ;
#51418 = CARTESIAN_POINT ( 'NONE',  ( -59.66743547012691806, -272.2376801242465376, -200.0775824269973384 ) ) ;
#51419 = DIRECTION ( 'NONE',  ( 0.000000000000000000, 0.000000000000000000, -1.000000000000000000 ) ) ;
#51420 = PLANE ( 'NONE',  #66828 ) ;
#51421 = CARTESIAN_POINT ( 'NONE',  ( 37.75005991015741813, -276.5599169703956477, -286.7133135149941268 ) ) ;
#51422 = CARTESIAN_POINT ( 'NONE',  ( 36.93973550371305237, -277.4193302799413345, -260.0040445923528978 ) ) ;
#51423 = CARTESIAN_POINT ( 'NONE',  ( -112.2198929560257739, -276.9341662533229282, -285.6528870379738123 ) ) ;
#51424 = VERTEX_POINT ( 'NONE', #90008 ) ;
#51425 = CARTESIAN_POINT ( 'NONE',  ( 200.7568414405312751, 39.78480925505072463, 10.49999999999999822 ) ) ;
#51426 = CARTESIAN_POINT ( 'NONE',  ( 29.62718709690886598, -283.9870730079629197, -304.9092719664535025 ) ) ;
#51427 = CARTESIAN_POINT ( 'NONE',  ( -67.85924666746414857, -290.8382078271920932, -203.8546398804367641 ) ) ;
#51428 = CARTESIAN_POINT ( 'NONE',  ( 39.25393064353939820, -286.8082484606679827, -262.9753143014479519 ) ) ;
#51429 = EDGE_CURVE ( 'NONE', #18590, #93421, #4511, .T. ) ;
#51430 = CARTESIAN_POINT ( 'NONE',  ( -18.49899670153819287, -281.0460798014408965, -341.9888668150459239 ) ) ;
#51431 = CARTESIAN_POINT ( 'NONE',  ( -95.59390966811150747, -282.4986398064423270, -315.3489596925234082 ) ) ;
#51432 = CARTESIAN_POINT ( 'NONE',  ( 30.38200422305712323, -282.3797132356800148, -242.0657054077556154 ) ) ;
#51433 = CARTESIAN_POINT ( 'NONE',  ( -84.52961589271976095, -271.4021107443734877, -212.0661675029861613 ) ) ;
#51434 = CARTESIAN_POINT ( 'NONE',  ( -93.82004815023677224, -282.2497098719531436, -321.5335470610789343 ) ) ;
#51435 = CARTESIAN_POINT ( 'NONE',  ( -93.14597332543328889, -297.8540675974251144, -320.4889635898066444 ) ) ;
#51436 = CARTESIAN_POINT ( 'NONE',  ( -106.4823877096816886, -279.1714356761793283, -294.6596929520679282 ) ) ;
#51437 = CARTESIAN_POINT ( 'NONE',  ( -100.9801976548508833, -287.0888725472586316, -230.3589923139726068 ) ) ;
#51438 = CARTESIAN_POINT ( 'NONE',  ( 194.7453183674696504, 19.99999999999992895, 15.62500000000045475 ) ) ;
#51439 = CARTESIAN_POINT ( 'NONE',  ( 208.4306832106271088, -74.55766379199613425, 0.000000000000000000 ) ) ;
#51440 = CARTESIAN_POINT ( 'NONE',  ( 35.71074242522526276, -295.7185769415397658, -289.6653879129536904 ) ) ;
#51441 = CARTESIAN_POINT ( 'NONE',  ( 33.13256286020257591, -273.8865216935262197, -296.1707854824464334 ) ) ;
#51442 = CARTESIAN_POINT ( 'NONE',  ( 0.6305773313442843975, -287.7568422106557477, -337.2214274436521464 ) ) ;
#51443 = CARTESIAN_POINT ( 'NONE',  ( 2.691392010305296623, -290.9983933267406542, -208.3022497218942419 ) ) ;
#51444 = CARTESIAN_POINT ( 'NONE',  ( -67.01704250314124067, -276.1343115458083162, -337.5966557142100442 ) ) ;
#51445 = CARTESIAN_POINT ( 'NONE',  ( -110.1000124254166366, -294.4997796230364315, -285.1586130065427369 ) ) ;
#51446 = CARTESIAN_POINT ( 'NONE',  ( -77.53879578183138221, -292.8153249138662204, -208.8352130454967437 ) ) ;
#51447 = CARTESIAN_POINT ( 'NONE',  ( -37.30987171927208124, -279.5519495502701943, -345.3611179825600175 ) ) ;
#51448 = CARTESIAN_POINT ( 'NONE',  ( -16.71309073743227458, -293.2703998742069871, -343.8812709142250696 ) ) ;
#51449 = CARTESIAN_POINT ( 'NONE',  ( 34.48425296021367359, -288.9303289733669544, -253.3515399664831307 ) ) ;
#51450 = CARTESIAN_POINT ( 'NONE',  ( -102.9351757981450532, -288.2849323774306640, -308.8249880105770444 ) ) ;
#51451 = EDGE_CURVE ( 'NONE', #27414, #79261, #77227, .T. ) ;
#51452 = CARTESIAN_POINT ( 'NONE',  ( -20.98082687442135708, -290.2633378636901398, -342.1085690995844288 ) ) ;
#51453 = DIRECTION ( 'NONE',  ( 8.659560562354932858E-17, 0.7071067811865474617, -0.7071067811865474617 ) ) ;
#51454 = CARTESIAN_POINT ( 'NONE',  ( -68.81820771131771153, -290.2797560707646198, -336.4052789502438827 ) ) ;
#51455 = DIRECTION ( 'NONE',  ( -0.000000000000000000, 1.000000000000000000, 0.000000000000000000 ) ) ;
#51456 = CARTESIAN_POINT ( 'NONE',  ( 20.28437933050187425, -289.4437260866753263, -320.8511097140428774 ) ) ;
#51457 = CARTESIAN_POINT ( 'NONE',  ( -109.7496430750738483, -276.8396252520901726, -249.4925626328013948 ) ) ;
#51458 = CARTESIAN_POINT ( 'NONE',  ( -38.17393650028858332, -280.3752688410053793, -193.3867607311133554 ) ) ;
#51459 = EDGE_CURVE ( 'NONE', #69103, #68845, #22625, .T. ) ;
#51460 = CARTESIAN_POINT ( 'NONE',  ( -71.22146339282159033, -279.2837893561733722, -201.2387197835106463 ) ) ;
#51461 = CARTESIAN_POINT ( 'NONE',  ( 32.33400821136631720, -285.9150837605819220, -298.2552784806180739 ) ) ;
#51462 = CARTESIAN_POINT ( 'NONE',  ( 196.8702642586142986, 40.96915988761478644, 12.42857142857142350 ) ) ;
#51463 = CARTESIAN_POINT ( 'NONE',  ( -95.74823965925392599, -277.3272824979381994, -224.5199116817613572 ) ) ;
#51464 = CARTESIAN_POINT ( 'NONE',  ( -82.69459577496682812, -281.6714023057865575, -330.1600784574403065 ) ) ;
#51465 = DIRECTION ( 'NONE',  ( 0.9951408606192332362, 1.205805641958552022E-17, 0.09846150276129254919 ) ) ;
#51466 = CARTESIAN_POINT ( 'NONE',  ( -88.45257126145590121, -277.8307061036803702, -213.7008443938491666 ) ) ;
#51467 = CARTESIAN_POINT ( 'NONE',  ( -107.6372678634031956, -283.8664351519456091, -239.5685517524192676 ) ) ;
#51468 = CARTESIAN_POINT ( 'NONE',  ( -89.36415982661537782, -274.0989427967181769, -218.9192535745787325 ) ) ;
#51469 = CARTESIAN_POINT ( 'NONE',  ( -9.351672897702075105, -299.7108510549784341, -193.8481552504320859 ) ) ;
#51470 = CARTESIAN_POINT ( 'NONE',  ( 28.04754862254848291, -275.6608127046996515, -302.9763796356857029 ) ) ;
#51471 = CARTESIAN_POINT ( 'NONE',  ( 15.74957097491475722, -296.3011702534035408, -323.4088545178870504 ) ) ;
#51472 = CARTESIAN_POINT ( 'NONE',  ( 0.7211415310280909763, -288.7261983510460936, -337.3558177322461802 ) ) ;
#51473 = CARTESIAN_POINT ( 'NONE',  ( 34.80811009731442596, -279.3446851516665106, -247.9174310598610305 ) ) ;
#51474 = CARTESIAN_POINT ( 'NONE',  ( -2.053946846237938217, -292.3396013615513880, -201.9082332835468776 ) ) ;
#51476 = CARTESIAN_POINT ( 'NONE',  ( -29.15869370762009183, -288.0046506885831263, -343.1378096759977439 ) ) ;
#51475 = AXIS2_PLACEMENT_3D ( 'NONE', #81649, #3996, #75491 ) ;
#51477 = CARTESIAN_POINT ( 'NONE',  ( 37.50432874118308035, -291.6233253216327626, -275.9170354931635529 ) ) ;
#51478 = ORIENTED_EDGE ( 'NONE', *, *, #63587, .T. ) ;
#51479 = CARTESIAN_POINT ( 'NONE',  ( 198.6670339576480160, 69.03724764704809047, 9.597602971383192738 ) ) ;
#51480 = CARTESIAN_POINT ( 'NONE',  ( -109.4808660694708919, -289.9062295050376861, -282.0126272586754794 ) ) ;
#51481 = DIRECTION ( 'NONE',  ( -0.000000000000000000, -0.000000000000000000, -1.000000000000000000 ) ) ;
#51482 = CARTESIAN_POINT ( 'NONE',  ( 22.80004149195270458, -287.8528267523544741, -222.6349184610621990 ) ) ;
#51483 = CARTESIAN_POINT ( 'NONE',  ( -82.13390479932378696, -287.9090924074130839, -214.2458315076590907 ) ) ;
#51484 = CARTESIAN_POINT ( 'NONE',  ( -22.15585142638321869, -293.9209410872509807, -345.6087771587921225 ) ) ;
#51485 = CARTESIAN_POINT ( 'NONE',  ( -8.211044061489817025, -283.9938639573693422, -341.1612280169849782 ) ) ;
#51486 = CARTESIAN_POINT ( 'NONE',  ( -57.39234806562222246, -285.6195142118892250, -200.1161158421914763 ) ) ;
#51487 = CARTESIAN_POINT ( 'NONE',  ( 33.32962563312794657, -276.6002865124329446, -250.0099622126104464 ) ) ;
#51488 = CARTESIAN_POINT ( 'NONE',  ( 4.722953411414295033, -292.5011172347317370, -332.0248165667503599 ) ) ;
#51489 = CARTESIAN_POINT ( 'NONE',  ( 7.586010280570228304, -273.4760008703399308, -212.3212063608265794 ) ) ;
#51490 = ORIENTED_EDGE ( 'NONE', *, *, #14384, .T. ) ;
#51491 = CARTESIAN_POINT ( 'NONE',  ( -96.12512592106646991, -239.9971452530988358, -342.0757611934672582 ) ) ;
#51492 = CARTESIAN_POINT ( 'NONE',  ( -32.01821008745215380, -294.6534699819620755, -347.1689308397690183 ) ) ;
#51493 = CARTESIAN_POINT ( 'NONE',  ( -11.54545232377714470, -288.3109337429892776, -200.5337036185871682 ) ) ;
#51494 = CARTESIAN_POINT ( 'NONE',  ( -110.9149370818568059, -297.3586985871093589, -292.0516070652091685 ) ) ;
#51495 = CARTESIAN_POINT ( 'NONE',  ( 35.09599560119829675, -288.0691792901280905, -260.1594505518147571 ) ) ;
#51496 = CARTESIAN_POINT ( 'NONE',  ( -98.62285123107045592, -276.9931017054823315, -316.6151600833169937 ) ) ;
#51497 = CARTESIAN_POINT ( 'NONE',  ( 33.32617774255534471, -294.5917845606924743, -300.8166419520252930 ) ) ;
#51498 = CARTESIAN_POINT ( 'NONE',  ( 13.75294810023830472, -286.4850339426432129, -326.3753983022115790 ) ) ;
#51499 = CARTESIAN_POINT ( 'NONE',  ( 0.5337987675556906675, -294.8949596031568490, -337.3926416029415805 ) ) ;
#51500 = CARTESIAN_POINT ( 'NONE',  ( -17.43090634539850825, -292.6493979765727431, -200.0543458388402485 ) ) ;
#51501 = DIRECTION ( 'NONE',  ( -0.000000000000000000, -1.000000000000000000, -0.000000000000000000 ) ) ;
#51502 = FACE_OUTER_BOUND ( 'NONE', #19115, .T. ) ;
#51503 = CARTESIAN_POINT ( 'NONE',  ( -93.16763214118681447, -239.2410508537433884, -338.7284373407006797 ) ) ;
#51504 = CARTESIAN_POINT ( 'NONE',  ( 21.54268577276647179, -288.4142508919589432, -221.8293051974474110 ) ) ;
#51505 = CARTESIAN_POINT ( 'NONE',  ( -99.90806341382575795, -281.4094976428775112, -320.2154176792147382 ) ) ;
#51506 = ORIENTED_EDGE ( 'NONE', *, *, #34702, .F. ) ;
#51507 = CARTESIAN_POINT ( 'NONE',  ( -22.57761245057275801, -279.5848302304230515, -194.8394933818699428 ) ) ;
#51508 = CARTESIAN_POINT ( 'NONE',  ( 28.04878311192764428, -283.0669582122817474, -233.9727527325047447 ) ) ;
#51509 = CARTESIAN_POINT ( 'NONE',  ( 181.7656723149513880, 252.4586733329624053, -166.1422410563588130 ) ) ;
#51510 = CARTESIAN_POINT ( 'NONE',  ( -68.24568264764472758, -284.2289048048329505, -200.4644511332673744 ) ) ;
#51511 = CARTESIAN_POINT ( 'NONE',  ( 17.04668346832513848, -286.3495989613521147, -321.2618796214046597 ) ) ;
#51512 = CARTESIAN_POINT ( 'NONE',  ( -46.75145511815055244, -275.7943065919627088, -195.1829164207212557 ) ) ;
#51513 = CARTESIAN_POINT ( 'NONE',  ( -84.11903992990953327, -297.8813703588620569, -214.1713655441783999 ) ) ;
#51514 = CARTESIAN_POINT ( 'NONE',  ( 8.522949523767147539, -293.0939367030430276, -327.8519173053024929 ) ) ;
#51515 = CARTESIAN_POINT ( 'NONE',  ( -67.66077212544553277, -278.0910863022785975, -341.0298285978793729 ) ) ;
#51517 = CARTESIAN_POINT ( 'NONE',  ( -102.2425666139509559, -278.3589462117289486, -236.6091812185341325 ) ) ;
#51516 = CARTESIAN_POINT ( 'NONE',  ( 29.15426609100027378, -275.9581228753388018, -300.4823144493466884 ) ) ;
#51518 = CARTESIAN_POINT ( 'NONE',  ( 21.60441516583463084, -275.9692775008721242, -221.3014807778387478 ) ) ;
#51519 = CARTESIAN_POINT ( 'NONE',  ( -5.426000899097470409, -275.5623375294906054, -340.0954757530493566 ) ) ;
#51520 = CARTESIAN_POINT ( 'NONE',  ( -108.1563228279122768, -262.1275830946152041, -317.5270657317772702 ) ) ;
#51521 = CARTESIAN_POINT ( 'NONE',  ( -46.06852554266539101, -275.1625392261226466, -344.9032639548833004 ) ) ;
#51522 = EDGE_CURVE ( 'NONE', #70988, #60279, #51413, .T. ) ;
#51523 = CARTESIAN_POINT ( 'NONE',  ( -105.9919509934429698, -298.4115808985222316, -236.8089295680381952 ) ) ;
#51524 = CARTESIAN_POINT ( 'NONE',  ( 31.95455697924148097, -277.6233781216988064, -236.9535640164627637 ) ) ;
#51525 = CARTESIAN_POINT ( 'NONE',  ( -87.71122462277782006, -229.8683413793775117, -344.1918058839762011 ) ) ;
#51526 = CARTESIAN_POINT ( 'NONE',  ( -6.900640255930542644, -287.5409829054607940, -203.6572456730689282 ) ) ;
#51527 = CARTESIAN_POINT ( 'NONE',  ( -103.5232766187397999, -285.8201101801178652, -307.8035823936453994 ) ) ;
#51528 = CARTESIAN_POINT ( 'NONE',  ( 6.995324597041635784, -286.0223298788998250, -212.1755509813080778 ) ) ;
#51529 = CARTESIAN_POINT ( 'NONE',  ( -98.32121526661819644, -276.3799919904208764, -311.9296054340202886 ) ) ;
#51530 = CARTESIAN_POINT ( 'NONE',  ( -76.76332396977754513, -285.4459938954857421, -333.3250083207291254 ) ) ;
#51531 = CARTESIAN_POINT ( 'NONE',  ( -14.07176115676825034, -278.8392872868009817, -200.3842248877257646 ) ) ;
#51532 = CARTESIAN_POINT ( 'NONE',  ( -39.15167158012825865, -278.1550714810845193, -343.6478840308668055 ) ) ;
#51533 = CARTESIAN_POINT ( 'NONE',  ( 196.8803347170859865, 20.19615242270661426, 12.49999999999999289 ) ) ;
#51534 = CARTESIAN_POINT ( 'NONE',  ( -99.33600732362529584, -273.5776517489460957, -231.6998412713061555 ) ) ;
#51535 = CARTESIAN_POINT ( 'NONE',  ( -17.04450508939578768, -281.1105946589420910, -196.2518561215067905 ) ) ;
#51536 = CARTESIAN_POINT ( 'NONE',  ( 13.64470276825844230, -282.8529038051732982, -328.0507303541347710 ) ) ;
#51537 = ORIENTED_EDGE ( 'NONE', *, *, #77868, .F. ) ;
#51538 = ORIENTED_EDGE ( 'NONE', *, *, #73794, .T. ) ;
#51539 = CARTESIAN_POINT ( 'NONE',  ( 198.3325868694534222, 18.45344983985875231, -10.88803913700318127 ) ) ;
#51540 = CARTESIAN_POINT ( 'NONE',  ( 38.12206254256724236, -289.3196729603439508, -263.0524668228799783 ) ) ;
#51541 = CARTESIAN_POINT ( 'NONE',  ( -70.44097758174139301, -288.1641391424131484, -339.3518567632083887 ) ) ;
#51542 = CARTESIAN_POINT ( 'NONE',  ( -106.1425256547889262, -295.4168378874039718, -295.3908183492602575 ) ) ;
#51543 = CARTESIAN_POINT ( 'NONE',  ( -47.72141014014221838, -291.2722034441277970, -194.1130751415974203 ) ) ;
#51544 = ADVANCED_FACE ( 'NONE', ( #5278 ), #39296, .F. ) ;
#51545 = CARTESIAN_POINT ( 'NONE',  ( 28.84203366586359607, -286.4669256282139145, -302.7713190245626151 ) ) ;
#51546 = CARTESIAN_POINT ( 'NONE',  ( 28.00470673309790826, -288.3042642937858204, -236.8278898279071427 ) ) ;
#51547 = CARTESIAN_POINT ( 'NONE',  ( -114.2704648735229114, -299.0519495502701943, -270.3937649182068981 ) ) ;
#51548 = CARTESIAN_POINT ( 'NONE',  ( 34.86597864598481777, -289.8137000892604647, -290.6826865948855811 ) ) ;
#51549 = CARTESIAN_POINT ( 'NONE',  ( -95.87879206254001474, -287.9043026808990362, -317.5347622934455103 ) ) ;
#51550 = TOROIDAL_SURFACE ( 'NONE', #28931, 8.222204860432942297, 1.000000000000000000 ) ;
#51551 = CARTESIAN_POINT ( 'NONE',  ( -99.22345584756880044, -284.9527490412704651, -309.6230683398875385 ) ) ;
#51552 = CARTESIAN_POINT ( 'NONE',  ( -97.74686961344146141, -293.1617239508714761, -225.6042820436836109 ) ) ;
#51553 = DIRECTION ( 'NONE',  ( 0.000000000000000000, -1.000000000000000000, -0.000000000000000000 ) ) ;
#51554 = PLANE ( 'NONE',  #45780 ) ;
#51555 = CARTESIAN_POINT ( 'NONE',  ( -101.3358179605779981, -275.0639070193280986, -230.5721787613621530 ) ) ;
#51556 = CARTESIAN_POINT ( 'NONE',  ( 34.64249328587163035, -280.9223010025953045, -283.5032802121699547 ) ) ;
#51557 = CARTESIAN_POINT ( 'NONE',  ( -33.41634072821867818, -281.0025978053354834, -345.2712460209173173 ) ) ;
#51558 = CARTESIAN_POINT ( 'NONE',  ( 39.44514265855386270, -292.7846346989077801, -273.1788466563999123 ) ) ;
#51559 = CARTESIAN_POINT ( 'NONE',  ( -37.12704547263024324, -296.4547617808264590, -196.5582917753991694 ) ) ;
#51560 = CARTESIAN_POINT ( 'NONE',  ( 36.26922387774162360, -273.4875589136615304, -259.1960850271480012 ) ) ;
#51561 = CARTESIAN_POINT ( 'NONE',  ( -73.10138559252372659, -298.8826822098195066, -206.1545110475628917 ) ) ;
#51562 = DIRECTION ( 'NONE',  ( -0.000000000000000000, 1.000000000000000000, 0.000000000000000000 ) ) ;
#51563 = CARTESIAN_POINT ( 'NONE',  ( -57.94515094746591188, -272.3659471441075652, -196.7255249332656604 ) ) ;
#51564 = CARTESIAN_POINT ( 'NONE',  ( -65.25243010132754762, -293.6518021448031277, -341.0502221943905283 ) ) ;
#51565 = EDGE_CURVE ( 'NONE', #7087, #70758, #43572, .T. ) ;
#51566 = CARTESIAN_POINT ( 'NONE',  ( 34.35357825303041324, -295.1951546965901798, -287.0046998196123695 ) ) ;
#51567 = CARTESIAN_POINT ( 'NONE',  ( 194.3144103428324172, 250.0000000000000568, 16.91223866672520515 ) ) ;
#51568 = CARTESIAN_POINT ( 'NONE',  ( -35.63662330301218617, -295.8330851369480570, -343.5152470036020986 ) ) ;
#51569 = CARTESIAN_POINT ( 'NONE',  ( 151.3711209067282368, 130.9666726753620196, 11.50000000000000178 ) ) ;
#51571 = CARTESIAN_POINT ( 'NONE',  ( -107.8356591662239055, -296.8031960251138912, -251.3497813343888936 ) ) ;
#51570 = CARTESIAN_POINT ( 'NONE',  ( -111.5224520475220658, -282.3992386006758011, -283.9004205813481008 ) ) ;
#51572 = CARTESIAN_POINT ( 'NONE',  ( -87.74994165089476894, -285.3708314892757016, -212.0839224961861760 ) ) ;
#51573 = CARTESIAN_POINT ( 'NONE',  ( 23.95374330326716716, -284.0695214465138179, -314.5666032461355144 ) ) ;
#51574 = CARTESIAN_POINT ( 'NONE',  ( 9.801154225267605824, -286.3481616322209220, -209.5064092505764961 ) ) ;
#51575 = CARTESIAN_POINT ( 'NONE',  ( -47.21167348868880964, -289.9262888767061099, -196.1815247602738452 ) ) ;
#51576 = CARTESIAN_POINT ( 'NONE',  ( -111.3446827290143801, -277.6384391010379886, -291.2625857043049677 ) ) ;
#51577 = CARTESIAN_POINT ( 'NONE',  ( -20.19161114001082069, -277.7666405000204009, -195.3683826091709363 ) ) ;
#51578 = CARTESIAN_POINT ( 'NONE',  ( -48.18343439339133027, -257.0657538259594617, -487.6787901984638438 ) ) ;
#51579 = CARTESIAN_POINT ( 'NONE',  ( 35.39175343796056694, -286.2129898035755105, -260.1417195151675514 ) ) ;
#51580 = CARTESIAN_POINT ( 'NONE',  ( -48.83629899556947862, -288.1154695846664708, -346.2394255820412923 ) ) ;
#51581 = CARTESIAN_POINT ( 'NONE',  ( 133.0872704186301405, -299.5541904835127980, -195.3611179825600175 ) ) ;
#51582 = CARTESIAN_POINT ( 'NONE',  ( -106.8904003388547466, -280.3864918002959712, -238.5858381513849622 ) ) ;
#51584 = CARTESIAN_POINT ( 'NONE',  ( 33.47712789946047707, -280.9834423564890926, -252.5119597210160407 ) ) ;
#51583 = CARTESIAN_POINT ( 'NONE',  ( -37.70686698473414822, -293.0767806102421673, -345.7282360733721589 ) ) ;
#51585 = CARTESIAN_POINT ( 'NONE',  ( 37.09711093659996095, -293.9653863938079326, -290.0553661733474655 ) ) ;
#51586 = CARTESIAN_POINT ( 'NONE',  ( -18.51669669479845126, -284.3725038957269931, -197.1296308933189607 ) ) ;
#51587 = EDGE_CURVE ( 'NONE', #78927, #20997, #34147, .T. ) ;
#51588 = CARTESIAN_POINT ( 'NONE',  ( -108.7542917987817077, -280.2545261917697985, -293.4463161030702167 ) ) ;
#51589 = CARTESIAN_POINT ( 'NONE',  ( -34.30339225811070492, -294.0717626604970292, -343.5333609022540600 ) ) ;
#51590 = ORIENTED_EDGE ( 'NONE', *, *, #50231, .F. ) ;
#51591 = LINE ( 'NONE', #45408, #54387 ) ;
#51592 = CARTESIAN_POINT ( 'NONE',  ( 20.94490568316089707, -282.8877125334589095, -223.7293864005971216 ) ) ;
#51593 = CARTESIAN_POINT ( 'NONE',  ( -106.9298080458953564, -295.7629108594917966, -292.7844062299135430 ) ) ;
#51594 = DIRECTION ( 'NONE',  ( -0.000000000000000000, -1.000000000000000000, -0.000000000000000000 ) ) ;
#51595 = CARTESIAN_POINT ( 'NONE',  ( -95.99890600148557951, -281.4094976428775681, -317.0979686699210447 ) ) ;
#51596 = CARTESIAN_POINT ( 'NONE',  ( 2.343374020077495068, -273.7668932137033835, -204.5640533806881365 ) ) ;
#51597 = CARTESIAN_POINT ( 'NONE',  ( -110.3063956430286510, -290.3386970636212254, -273.9068405058119993 ) ) ;
#51598 = CARTESIAN_POINT ( 'NONE',  ( -107.1073257192191335, -280.3866126434344892, -246.4668656059827470 ) ) ;
#51599 = CARTESIAN_POINT ( 'NONE',  ( -57.09513368708623204, -275.3933308992231446, -199.2005607208959077 ) ) ;
#51600 = CARTESIAN_POINT ( 'NONE',  ( -47.13317081521313412, -284.7746942242131354, -345.9294150123008080 ) ) ;
#51601 = CARTESIAN_POINT ( 'NONE',  ( 34.72704160853412247, -280.1638233896074439, -256.3942250783815666 ) ) ;
#51602 = CARTESIAN_POINT ( 'NONE',  ( -29.47910173162345515, -278.9528598568939515, -345.0001490536233177 ) ) ;
#51603 = VERTEX_POINT ( 'NONE', #41692 ) ;
#51604 = CARTESIAN_POINT ( 'NONE',  ( -64.89809936468039098, -273.5353297490814839, -198.4466900184550013 ) ) ;
#51605 = CARTESIAN_POINT ( 'NONE',  ( -73.34443220093123728, -293.4913029372727351, -205.1486192212192066 ) ) ;
#51606 = CARTESIAN_POINT ( 'NONE',  ( 198.6884013828325521, 64.61450673763175701, -9.555809373750795643 ) ) ;
#51607 = DIRECTION ( 'NONE',  ( -0.000000000000000000, -1.000000000000000000, -0.000000000000000000 ) ) ;
#51608 = CARTESIAN_POINT ( 'NONE',  ( -11.50112392889963253, -292.8588402021799766, -341.6387504825224255 ) ) ;
#51609 = CARTESIAN_POINT ( 'NONE',  ( 2.969114865619621568, -274.1168070937578705, -209.3660418895248370 ) ) ;
#51610 = DIRECTION ( 'NONE',  ( 0.000000000000000000, -0.000000000000000000, 1.000000000000000000 ) ) ;
#51611 = CIRCLE ( 'NONE', #63767, 0.4999999999999941158 ) ;
#51612 = CARTESIAN_POINT ( 'NONE',  ( 27.45329504610856119, -294.5391058367924870, -229.9585084527130618 ) ) ;
#51614 = CARTESIAN_POINT ( 'NONE',  ( 22.78679633143006100, -294.1188887239611631, -222.8788878413000134 ) ) ;
#51613 = CARTESIAN_POINT ( 'NONE',  ( -20.19161114001083490, -285.3376638359844719, -345.3538533559490702 ) ) ;
#51615 = CARTESIAN_POINT ( 'NONE',  ( 36.77972346564443029, -289.6860340952448496, -280.7523597154669233 ) ) ;
#51616 = CARTESIAN_POINT ( 'NONE',  ( 14.99578389997540206, -274.3122857512170185, -323.9198584516471442 ) ) ;
#51617 = B_SPLINE_CURVE_WITH_KNOTS ( 'NONE', 3,
 ( #21163, #28742, #50970, #71371, #52711, #79854 ),
 .UNSPECIFIED., .F., .F.,
 ( 4, 2, 4 ),
 ( 0.000000000000000000, 0.0004262108901887123489, 0.0008524217803774246979 ),
 .UNSPECIFIED. ) ;
#51618 = CARTESIAN_POINT ( 'NONE',  ( 6.259644447126521349, -278.3756213712943577, -330.7591618347854592 ) ) ;
#51619 = CARTESIAN_POINT ( 'NONE',  ( 37.08057606013549901, -291.6735687044987344, -273.5750589786385376 ) ) ;
#51620 = CARTESIAN_POINT ( 'NONE',  ( -92.19609144501890796, -281.1393604072019912, -218.0242795429592775 ) ) ;
#51621 = ORIENTED_EDGE ( 'NONE', *, *, #56217, .F. ) ;
#51622 = CARTESIAN_POINT ( 'NONE',  ( -8.489791802609559568, -282.3304788351815660, -337.4405848320453174 ) ) ;
#51623 = CARTESIAN_POINT ( 'NONE',  ( -84.38819405829782738, -280.5017872345344472, -209.7288997785005051 ) ) ;
#51624 = CARTESIAN_POINT ( 'NONE',  ( 32.02627016541798355, -280.7667768477475079, -302.9836265505269353 ) ) ;
#51625 = CARTESIAN_POINT ( 'NONE',  ( -68.90763339293847878, -278.3983720020250416, -340.3498446071059220 ) ) ;
#51626 =( NAMED_UNIT ( * ) PLANE_ANGLE_UNIT ( ) SI_UNIT ( $, .RADIAN. ) );
#51627 = CARTESIAN_POINT ( 'NONE',  ( 25.56195184069837723, -276.4967306381847152, -227.1426158259065176 ) ) ;
#51628 = CARTESIAN_POINT ( 'NONE',  ( -92.08974858914540107, -287.6948066931273047, -226.7417163044926838 ) ) ;
#51629 = ORIENTED_EDGE ( 'NONE', *, *, #73478, .T. ) ;
#51630 = CARTESIAN_POINT ( 'NONE',  ( -99.37691940767398080, -275.1208352733501101, -228.4157905965967927 ) ) ;
#51631 = CARTESIAN_POINT ( 'NONE',  ( -57.75414217784511806, -292.8620947905608887, -199.8980839639592091 ) ) ;
#51632 = CARTESIAN_POINT ( 'NONE',  ( -43.36438112073825835, -275.1487065485370636, -344.7625569244016788 ) ) ;
#51633 = CARTESIAN_POINT ( 'NONE',  ( -110.9349403241829464, -292.0717447851199609, -289.3342355719657917 ) ) ;
#51634 = CARTESIAN_POINT ( 'NONE',  ( -38.89143457441620200, -291.3807856368616171, -197.2756133208389713 ) ) ;
#51635 = CARTESIAN_POINT ( 'NONE',  ( 23.23512552972464107, -287.6945525438034679, -317.8162318287989478 ) ) ;
#51636 = CARTESIAN_POINT ( 'NONE',  ( 222.4306832106270804, -141.7221692137691775, -22.50000000000000000 ) ) ;
#51638 = CARTESIAN_POINT ( 'NONE',  ( -61.81907311342790479, -281.7753799530041761, -340.0374878636112612 ) ) ;
#51637 = CARTESIAN_POINT ( 'NONE',  ( 38.27154246693870476, -291.9836314069960395, -258.9944522024007938 ) ) ;
#51639 = CARTESIAN_POINT ( 'NONE',  ( -111.0124639627065903, -292.2940468195929498, -279.4980778574630449 ) ) ;
#51640 = CARTESIAN_POINT ( 'NONE',  ( -110.9191896322689104, -283.0968601607828532, -265.3994165696995537 ) ) ;
#51641 = CARTESIAN_POINT ( 'NONE',  ( 33.92974531635276492, -282.6316308831800939, -252.3761424678914125 ) ) ;
#51642 = CARTESIAN_POINT ( 'NONE',  ( -112.3329090950867197, -291.2875975136693683, -286.7665680445915086 ) ) ;
#51643 = CARTESIAN_POINT ( 'NONE',  ( 35.09294997241880054, -281.9136679203530775, -260.4348292019039377 ) ) ;
#51644 = CARTESIAN_POINT ( 'NONE',  ( -25.06985353031387120, -291.0002499313933413, -194.7475576992289064 ) ) ;
#51645 = CARTESIAN_POINT ( 'NONE',  ( 1.431349676844140939, -287.3592656706775301, -204.0072160270258905 ) ) ;
#51646 = CARTESIAN_POINT ( 'NONE',  ( 38.49513895880458136, -287.8811516476849874, -257.3105717182550052 ) ) ;
#51647 = CARTESIAN_POINT ( 'NONE',  ( -33.24077978194360128, -286.2717666972439474, -197.4265775622738772 ) ) ;
#51648 = ORIENTED_EDGE ( 'NONE', *, *, #8814, .F. ) ;
#51649 = DIRECTION ( 'NONE',  ( -0.6056179655966479336, 0.7957555401921982963, 0.000000000000000000 ) ) ;
#51650 = CARTESIAN_POINT ( 'NONE',  ( -30.67564585599519589, -296.8291322073731635, -345.8321004901878268 ) ) ;
#51651 = CARTESIAN_POINT ( 'NONE',  ( -32.06336046332013012, -293.6717356359525866, -346.6988407170836695 ) ) ;
#51652 = CARTESIAN_POINT ( 'NONE',  ( -71.77538176415235682, -276.5777251577628135, -335.0106260483595406 ) ) ;
#51653 = CARTESIAN_POINT ( 'NONE',  ( -75.72182459495267892, -296.9028726064447596, -203.6645925338374354 ) ) ;
#51654 = CARTESIAN_POINT ( 'NONE',  ( 36.33429432913775514, -292.0735364145804738, -273.5379849549560163 ) ) ;
#51655 = CARTESIAN_POINT ( 'NONE',  ( -105.6895157450809961, -295.1676507923224335, -241.9612920727463461 ) ) ;
#51656 = CARTESIAN_POINT ( 'NONE',  ( 17.02200831704047701, -294.0537411095587572, -220.9741447264666476 ) ) ;
#51657 = CARTESIAN_POINT ( 'NONE',  ( 29.01248043674391042, -294.2111676511165683, -239.0748898811623917 ) ) ;
#51658 = CARTESIAN_POINT ( 'NONE',  ( 140.6539576904058606, 0.000000000000000000, 12.50000000000000000 ) ) ;
#51659 = CARTESIAN_POINT ( 'NONE',  ( -4.063910376749810816, -292.6142979405661890, -337.7743125028446229 ) ) ;
#51660 = CARTESIAN_POINT ( 'NONE',  ( -99.18376716040198460, -297.9771256121612737, -312.8166145294829334 ) ) ;
#51661 = CARTESIAN_POINT ( 'NONE',  ( -109.8542345570249950, -291.3572682127912117, -280.7145499118705629 ) ) ;
#51662 = CARTESIAN_POINT ( 'NONE',  ( -9.218816181171575863, -295.0073634883732439, -337.7630868465290064 ) ) ;
#51663 = CARTESIAN_POINT ( 'NONE',  ( -81.56029844326707234, -279.6305310699261213, -331.3785119213960684 ) ) ;
#51664 = CARTESIAN_POINT ( 'NONE',  ( -33.92045886808352151, -278.7791807461813960, -193.9308008180744025 ) ) ;
#51665 = VERTEX_POINT ( 'NONE', #64472 ) ;
#51666 = CARTESIAN_POINT ( 'NONE',  ( -73.88909482989376443, -272.9287860919027366, -202.6439581546898125 ) ) ;
#51667 = CARTESIAN_POINT ( 'NONE',  ( 18.67261079882158725, -280.3180480034368998, -319.3887751887700119 ) ) ;
#51668 = CARTESIAN_POINT ( 'NONE',  ( -113.5847819481960101, -276.9366823302664216, -271.5751011180207115 ) ) ;
#51669 = CARTESIAN_POINT ( 'NONE',  ( -83.42243452349075028, -277.4224509311123938, -210.9101312106916453 ) ) ;
#51670 = CARTESIAN_POINT ( 'NONE',  ( -65.74796355123966407, -296.3574412365002786, -202.5796479696884944 ) ) ;
#51671 = CARTESIAN_POINT ( 'NONE',  ( -112.3417001281054297, -274.5519904173220311, -270.3865538441530134 ) ) ;
#51672 = DIRECTION ( 'NONE',  ( -1.000000000000000000, 0.000000000000000000, -0.000000000000000000 ) ) ;
#51673 = AXIS2_PLACEMENT_3D ( 'NONE', #28740, #85086, #92649 ) ;
#51674 = CARTESIAN_POINT ( 'NONE',  ( -112.7228054487562758, -288.5976714566861574, -268.3724124827416517 ) ) ;
#51675 = AXIS2_PLACEMENT_3D ( 'NONE', #25600, #69173, #38867 ) ;
#51676 = CARTESIAN_POINT ( 'NONE',  ( -114.1124757261751483, -290.4697041760436491, -276.9535925488979160 ) ) ;
#51677 = CARTESIAN_POINT ( 'NONE',  ( 3.836990852237445626, -276.6048393859001635, -207.4158012753741787 ) ) ;
#51678 = CARTESIAN_POINT ( 'NONE',  ( -100.9639638295098507, -271.0855457997349163, -230.6470372420505441 ) ) ;
#51679 = CARTESIAN_POINT ( 'NONE',  ( -37.97084460644526160, -285.2416296256656096, -193.5251693742420400 ) ) ;
#51680 = CARTESIAN_POINT ( 'NONE',  ( 175.2296996224750103, 134.0000000000000284, 24.00000000000001066 ) ) ;
#51681 = CONICAL_SURFACE ( 'NONE', #75964, 6.500000000000024869, 0.7853981633974488341 ) ;
#51682 = CARTESIAN_POINT ( 'NONE',  ( -35.20354040728916800, -281.0251771647569967, -345.3432887154716013 ) ) ;
#51683 = CARTESIAN_POINT ( 'NONE',  ( 198.5293976730290524, 24.71549707027390141, 10.72178272431895962 ) ) ;
#51684 = CARTESIAN_POINT ( 'NONE',  ( 13.18757191924456151, -291.5727708067083199, -217.1265129731111756 ) ) ;
#51685 = CARTESIAN_POINT ( 'NONE',  ( -86.52711838184109183, -283.5003021195386737, -214.6897341499047513 ) ) ;
#51686 = CARTESIAN_POINT ( 'NONE',  ( -113.5000000000000568, -218.8335761803644743, -490.8867980474134356 ) ) ;
#51687 = DIRECTION ( 'NONE',  ( 0.000000000000000000, 0.000000000000000000, -1.000000000000000000 ) ) ;
#51688 = CARTESIAN_POINT ( 'NONE',  ( 35.25024326259225660, -291.3097428884024680, -251.5087863881390149 ) ) ;
#51689 = CARTESIAN_POINT ( 'NONE',  ( -81.27951722050408989, -279.2609849072333645, -329.6562159443857354 ) ) ;
#51690 = CARTESIAN_POINT ( 'NONE',  ( -3.056718355146273325, -283.8144285654549890, -338.8778774335357866 ) ) ;
#51692 = CARTESIAN_POINT ( 'NONE',  ( -105.5649326430529271, -284.8989327378303642, -244.3882370255285252 ) ) ;
#51691 = CARTESIAN_POINT ( 'NONE',  ( -0.7215142817322897084, -272.6144445692577847, -204.2534669931673079 ) ) ;
#51693 = CARTESIAN_POINT ( 'NONE',  ( 27.14418845292203741, -276.4957481868808600, -234.8015397374245481 ) ) ;
#51694 = CARTESIAN_POINT ( 'NONE',  ( 19.31311742701443279, -277.0091579537096891, -316.6716112503846716 ) ) ;
#51695 = ADVANCED_FACE ( 'NONE', ( #5737 ), #64931, .F. ) ;
#51696 = CARTESIAN_POINT ( 'NONE',  ( -110.2682972287494891, -286.3267434943717262, -287.9286054130099046 ) ) ;
#51697 = VERTEX_POINT ( 'NONE', #27506 ) ;
#51698 = DIRECTION ( 'NONE',  ( 0.7957555401921962979, 0.6056179655966504871, -8.673617379884085762E-16 ) ) ;
#51699 = CARTESIAN_POINT ( 'NONE',  ( -112.6056091699295791, -296.1821361037062843, -286.6197772223017068 ) ) ;
#51700 = CARTESIAN_POINT ( 'NONE',  ( 12.20745792215177516, -288.7250639320607775, -214.4640308664372981 ) ) ;
#51701 = CARTESIAN_POINT ( 'NONE',  ( 188.2019740231993410, 44.81720372851549428, 12.00000000000000000 ) ) ;
#51702 = CARTESIAN_POINT ( 'NONE',  ( -115.3430155898818299, -293.8380690714490129, -288.1317622949166548 ) ) ;
#51703 = CARTESIAN_POINT ( 'NONE',  ( -56.46622564396024302, -278.7317438173255368, -196.0382793546128255 ) ) ;
#51704 = CARTESIAN_POINT ( 'NONE',  ( -1.165508133930641899, -290.9238889895950138, -203.2960484647188082 ) ) ;
#51705 = CARTESIAN_POINT ( 'NONE',  ( -65.37473102826832871, -287.1991883730297559, -202.1536045630575131 ) ) ;
#51706 = CARTESIAN_POINT ( 'NONE',  ( -108.7927429910693320, -280.0607702022878129, -289.6671400754698311 ) ) ;
#51707 = CARTESIAN_POINT ( 'NONE',  ( 28.40605071646576008, -289.4885580561158918, -309.2949021636125622 ) ) ;
#51708 = CARTESIAN_POINT ( 'NONE',  ( 20.04056526586238718, -284.2201907275607482, -318.6747089409196292 ) ) ;
#51709 = CARTESIAN_POINT ( 'NONE',  ( -111.3378347064482483, -278.9858507896692004, -249.0638864259610159 ) ) ;
#51710 = CARTESIAN_POINT ( 'NONE',  ( -80.66259005203754384, -295.4813998916320656, -209.5733947463996856 ) ) ;
#51711 = CARTESIAN_POINT ( 'NONE',  ( -114.3777617634478361, -278.4058452298719430, -268.7321277066191669 ) ) ;
#51712 = CARTESIAN_POINT ( 'NONE',  ( -36.74962053950157781, -275.9200846893302810, -196.1156507256139037 ) ) ;
#51713 = CARTESIAN_POINT ( 'NONE',  ( 197.8598376457711367, 297.6481317602094236, -7.112773483223372217 ) ) ;
#51714 = CARTESIAN_POINT ( 'NONE',  ( -54.49178911615187815, -288.3376638359845856, -195.3683826091709363 ) ) ;
#51715 = CARTESIAN_POINT ( 'NONE',  ( -100.3555003455923895, -271.3600266310947973, -227.8029686674794618 ) ) ;
#51716 = CYLINDRICAL_SURFACE ( 'NONE', #50071, 4.000000000000003553 ) ;
#51717 = CARTESIAN_POINT ( 'NONE',  ( -64.83346329196058377, -279.1907823994736191, -202.6692322067896441 ) ) ;
#51718 = CARTESIAN_POINT ( 'NONE',  ( 39.31022670569921473, -276.7671707211511034, -271.1521465307259859 ) ) ;
#51719 = CARTESIAN_POINT ( 'NONE',  ( -24.58452265463143860, -281.9520499287045823, -346.1123236937039565 ) ) ;
#51720 = CARTESIAN_POINT ( 'NONE',  ( -31.77304763926113651, -290.7412018032209176, -344.2159951128452349 ) ) ;
#51721 = CARTESIAN_POINT ( 'NONE',  ( -30.58069267507421429, -299.6554609107259921, -194.0527348764640863 ) ) ;
#51722 = CARTESIAN_POINT ( 'NONE',  ( -97.04656720098439848, -298.4037222275503041, -222.3680188080467701 ) ) ;
#51723 = CARTESIAN_POINT ( 'NONE',  ( 15.63163035019207747, -296.3011702540286478, -323.2909306849135191 ) ) ;
#51724 = CARTESIAN_POINT ( 'NONE',  ( 20.26327926962336434, -278.8910007609364357, -222.5741322981677399 ) ) ;
#51725 = CARTESIAN_POINT ( 'NONE',  ( -27.03875510055579667, -272.2037422874089430, -196.3787248729832982 ) ) ;
#51726 = CARTESIAN_POINT ( 'NONE',  ( -80.50203437437069454, -287.0782939394681534, -207.4991215171385477 ) ) ;
#51727 = CARTESIAN_POINT ( 'NONE',  ( -86.94862462529601999, -288.6821678992318425, -324.4057227234073935 ) ) ;
#51728 = CARTESIAN_POINT ( 'NONE',  ( 175.5833602167774075, 242.2213184666997847, -179.4617043395230382 ) ) ;
#51729 = ORIENTED_EDGE ( 'NONE', *, *, #11367, .T. ) ;
#51730 = CARTESIAN_POINT ( 'NONE',  ( 0.4122403315564826531, -287.1345029591557818, -336.8531712378951397 ) ) ;
#51731 = CARTESIAN_POINT ( 'NONE',  ( 31.41788371323971063, -287.5460617981311202, -294.9417428059152826 ) ) ;
#51732 = ORIENTED_EDGE ( 'NONE', *, *, #46714, .F. ) ;
#51733 = CARTESIAN_POINT ( 'NONE',  ( -112.0616838708246803, -285.8487346899426598, -253.0863809110456373 ) ) ;
#51734 = CARTESIAN_POINT ( 'NONE',  ( -76.36353307757454445, -277.9226512050869928, -332.1407914791986968 ) ) ;
#51735 = CARTESIAN_POINT ( 'NONE',  ( 31.94483059854229268, -292.8969094194542890, -303.3614406634127363 ) ) ;
#51736 = CARTESIAN_POINT ( 'NONE',  ( 24.17855000973035473, -282.8184109370029091, -316.4975635533658078 ) ) ;
#51737 = CARTESIAN_POINT ( 'NONE',  ( 35.92850781740990840, -282.8020480421558887, -249.0027144860982276 ) ) ;
#51738 = CARTESIAN_POINT ( 'NONE',  ( -88.30436075307106591, -284.0761832059829430, -328.1258884340070949 ) ) ;
#51739 = CARTESIAN_POINT ( 'NONE',  ( -24.87695345809282799, -280.5488422214895650, -198.4117081368473805 ) ) ;
#51740 = CARTESIAN_POINT ( 'NONE',  ( -95.95921662488163406, -270.6952119285918457, -223.5744983911110353 ) ) ;
#51741 = CARTESIAN_POINT ( 'NONE',  ( -112.2661335305100607, -271.5905929391889231, -296.4060789002301703 ) ) ;
#51742 = ORIENTED_EDGE ( 'NONE', *, *, #18555, .F. ) ;
#51743 = AXIS2_PLACEMENT_3D ( 'NONE', #62772, #6866, #64187 ) ;
#51744 = CARTESIAN_POINT ( 'NONE',  ( -71.26159565677255614, -279.5012423282600480, -337.0654590507153330 ) ) ;
#51745 = CARTESIAN_POINT ( 'NONE',  ( 202.2090562182569329, 295.8239156117442690, -54.00000000003540634 ) ) ;
#51746 = CARTESIAN_POINT ( 'NONE',  ( -48.83192253240383707, -154.4817910994489125, -361.7742097625079509 ) ) ;
#51747 = AXIS2_PLACEMENT_3D ( 'NONE', #7917, #23536, #36342 ) ;
#51748 = CARTESIAN_POINT ( 'NONE',  ( -107.9319282003822025, -296.1518881054044527, -251.3152091021987928 ) ) ;
#51749 = CARTESIAN_POINT ( 'NONE',  ( 17.51326807713136091, -293.8017528632220206, -324.3855614581157170 ) ) ;
#51750 = CARTESIAN_POINT ( 'NONE',  ( -38.24214191940907881, -140.5200643640481530, -361.2081418523172260 ) ) ;
#51751 = ADVANCED_FACE ( 'NONE', ( #13780 ), #72470, .F. ) ;
#51752 = CIRCLE ( 'NONE', #10920, 1.499999999999999556 ) ;
#51754 = CARTESIAN_POINT ( 'NONE',  ( -101.0042690261450389, -288.4438275629378268, -307.7916663922778753 ) ) ;
#51753 = CARTESIAN_POINT ( 'NONE',  ( 18.86779562414340461, -297.3175958210166527, -193.9636422523521446 ) ) ;
#51755 = CARTESIAN_POINT ( 'NONE',  ( -67.78037544935655490, -297.3163264815419780, -338.0829004485497649 ) ) ;
#51756 = EDGE_CURVE ( 'NONE', #15284, #3498, #31760, .T. ) ;
#51757 = CARTESIAN_POINT ( 'NONE',  ( -29.10131066803382538, -290.2607129870415861, -343.3908342571914432 ) ) ;
#51758 = ORIENTED_EDGE ( 'NONE', *, *, #77632, .F. ) ;
#51759 = CARTESIAN_POINT ( 'NONE',  ( -24.93399507428794237, -295.8389866957581376, -346.1703434077252837 ) ) ;
#51760 = CARTESIAN_POINT ( 'NONE',  ( -9.475717188045660322, -286.9187402820135162, -202.8089034423035457 ) ) ;
#51761 = CARTESIAN_POINT ( 'NONE',  ( -40.40891024762056105, -296.8094625049994875, -193.7677614475972803 ) ) ;
#51762 = CARTESIAN_POINT ( 'NONE',  ( -81.84519527958066476, -292.2655190776030167, -207.7224898098984340 ) ) ;
#51763 = CARTESIAN_POINT ( 'NONE',  ( 1.663490251089023708, -293.0510353660948226, -203.9818970056705041 ) ) ;
#51764 = CARTESIAN_POINT ( 'NONE',  ( -98.30070881451759135, -291.2769263791527123, -230.1071322280571394 ) ) ;
#51765 = ORIENTED_EDGE ( 'NONE', *, *, #6503, .T. ) ;
#51766 = CARTESIAN_POINT ( 'NONE',  ( 154.1407330040854333, 250.0000000000000568, -13.42592592592592915 ) ) ;
#51767 = CARTESIAN_POINT ( 'NONE',  ( -63.08981177487974179, -275.6395554477534802, -199.3234593506664964 ) ) ;
#51768 = CARTESIAN_POINT ( 'NONE',  ( 39.23433943456829098, -274.3215646882962915, -268.3316149920015619 ) ) ;
#51769 = ORIENTED_EDGE ( 'NONE', *, *, #29467, .F. ) ;
#51770 = CARTESIAN_POINT ( 'NONE',  ( -6.605048963356055403, -276.1669382116546103, -340.9075191628697326 ) ) ;
#51771 = CARTESIAN_POINT ( 'NONE',  ( 96.00430790048001484, -298.2308315540366266, -196.7031297424393586 ) ) ;
#51772 = CARTESIAN_POINT ( 'NONE',  ( 26.42467482652973487, -274.2056338440190757, -308.3705234474269332 ) ) ;
#51773 = B_SPLINE_CURVE_WITH_KNOTS ( 'NONE', 3,
 ( #82430, #75332, #10448, #46890, #39314, #18038, #75791, #55434 ),
 .UNSPECIFIED., .F., .F.,
 ( 4, 2, 2, 4 ),
 ( 2.845565583954360595E-21, 0.001369958260980388021, 0.002054937391470581815, 0.002739916521960775609 ),
 .UNSPECIFIED. ) ;
#51774 = CARTESIAN_POINT ( 'NONE',  ( -34.04045928965716428, -275.1743224558018710, -197.1263729284439989 ) ) ;
#51775 = CARTESIAN_POINT ( 'NONE',  ( -24.56713583653360899, -275.1603083401777781, -198.1968209710419444 ) ) ;
#51776 = CARTESIAN_POINT ( 'NONE',  ( -35.86813203185662502, -299.6704306543792882, -194.1607190958659714 ) ) ;
#51777 = CARTESIAN_POINT ( 'NONE',  ( 24.80271614868557606, -272.9972813898556865, -227.7180730713507160 ) ) ;
#51778 = CARTESIAN_POINT ( 'NONE',  ( -92.26178022449579430, -296.5157983408155928, -318.6071278755809431 ) ) ;
#51779 = CARTESIAN_POINT ( 'NONE',  ( 20.97916625190972795, -292.7536754211492962, -315.2599282628933679 ) ) ;
#51780 = LINE ( 'NONE', #73584, #4856 ) ;
#51781 = CARTESIAN_POINT ( 'NONE',  ( 20.77788441106363848, -276.7264826566882334, -320.7957481113962785 ) ) ;
#51782 = CARTESIAN_POINT ( 'NONE',  ( -51.56353771953207854, -274.0319735407738335, -198.7080757365475279 ) ) ;
#51783 = CARTESIAN_POINT ( 'NONE',  ( -111.0210956306622450, -282.9771035354178252, -290.9680331296258942 ) ) ;
#51784 = CARTESIAN_POINT ( 'NONE',  ( -112.1167892953612153, -298.4541466750958989, -278.0236544501690332 ) ) ;
#51785 = DIRECTION ( 'NONE',  ( -0.000000000000000000, -0.000000000000000000, 1.000000000000000000 ) ) ;
#51786 = CARTESIAN_POINT ( 'NONE',  ( -70.04545606454857420, -284.8071136175269658, -204.9020058818749419 ) ) ;
#51787 = CARTESIAN_POINT ( 'NONE',  ( -111.4060476780554438, -276.7886409042052946, -270.6195273407540185 ) ) ;
#51788 = CARTESIAN_POINT ( 'NONE',  ( -81.18486162104123594, -276.2360711649095606, -329.4640122081586924 ) ) ;
#51789 = CARTESIAN_POINT ( 'NONE',  ( 18.55066038899585834, -284.2488858665664111, -320.3906144081263392 ) ) ;
#51790 = CARTESIAN_POINT ( 'NONE',  ( 35.98277186567027286, -276.7013367957666219, -266.1007085542030381 ) ) ;
#51791 = DIRECTION ( 'NONE',  ( 0.000000000000000000, 0.000000000000000000, -1.000000000000000000 ) ) ;
#51792 = CARTESIAN_POINT ( 'NONE',  ( 38.58166099535635141, -274.0340083866285568, -276.8483091883569500 ) ) ;
#51793 = CARTESIAN_POINT ( 'NONE',  ( -3.245082127908186731, -282.5014870486801328, -203.3583181042076831 ) ) ;
#51794 = CARTESIAN_POINT ( 'NONE',  ( 195.4781563537916043, 27.42197070042634621, 15.00000000000000000 ) ) ;
#51795 = CARTESIAN_POINT ( 'NONE',  ( -18.56397944953064183, -288.2121940331755354, -197.1174924024900577 ) ) ;
#51796 = CARTESIAN_POINT ( 'NONE',  ( 175.2296996224750103, 20.99999999999998934, 0.000000000000000000 ) ) ;
#51797 = CARTESIAN_POINT ( 'NONE',  ( -89.73759162597615102, -289.3133199411504961, -216.6269217376771508 ) ) ;
#51798 = CARTESIAN_POINT ( 'NONE',  ( 82.12584444479689694, -301.3619252513798301, -196.2136339012648421 ) ) ;
#51799 = CARTESIAN_POINT ( 'NONE',  ( -77.71767044612955999, -296.2919463044487429, -209.0064025358645665 ) ) ;
#51800 = CARTESIAN_POINT ( 'NONE',  ( -105.8337094111578267, -289.0709820956251974, -241.5968699754999420 ) ) ;
#51801 = CARTESIAN_POINT ( 'NONE',  ( 26.40820234725076787, -24.66803830325296687, -341.1985388896944755 ) ) ;
#51802 = CARTESIAN_POINT ( 'NONE',  ( 164.2231345125756263, 293.9636489450775230, 0.000000000000000000 ) ) ;
#51803 = CARTESIAN_POINT ( 'NONE',  ( 11.95305454682809554, -286.8611114333259025, -328.6083060046808555 ) ) ;
#51804 = CARTESIAN_POINT ( 'NONE',  ( -26.60648544987661523, -284.5135909336848385, -343.4280182904995513 ) ) ;
#51805 = CARTESIAN_POINT ( 'NONE',  ( -113.1392416281361903, -282.8687443791885698, -264.3063662864773278 ) ) ;
#51806 = CARTESIAN_POINT ( 'NONE',  ( -109.1789178478847333, -290.3809580755313391, -283.3385657392481676 ) ) ;
#51807 = CARTESIAN_POINT ( 'NONE',  ( 35.72708396225598904, -283.0972007792462364, -279.5136551379666798 ) ) ;
#51808 = CARTESIAN_POINT ( 'NONE',  ( -18.68461158030488178, -283.6086411758013242, -341.1562353184132235 ) ) ;
#51809 = CARTESIAN_POINT ( 'NONE',  ( -107.2626943707492728, -292.1676624055533011, -298.4584730987802459 ) ) ;
#51810 = AXIS2_PLACEMENT_3D ( 'NONE', #21531, #13055, #63252 ) ;
#51811 = CARTESIAN_POINT ( 'NONE',  ( 4.848023476581549751, -274.9382285887120361, -205.9102099542536735 ) ) ;
#51812 = VECTOR ( 'NONE', #55046, 1000.000000000000000 ) ;
#51813 = CARTESIAN_POINT ( 'NONE',  ( 32.69816433407451228, -286.0003991606355385, -298.8505309983199254 ) ) ;
#51814 = CARTESIAN_POINT ( 'NONE',  ( 2.418001196179785595, -274.5695963131491339, -204.4204920331079052 ) ) ;
#51815 = CARTESIAN_POINT ( 'NONE',  ( -4.802211893568830270, -296.6013840662571397, -337.5543205120396237 ) ) ;
#51816 = CARTESIAN_POINT ( 'NONE',  ( -39.58036566374939724, -229.5268262511776527, 22.50000000000000000 ) ) ;
#51817 = CARTESIAN_POINT ( 'NONE',  ( -85.33152481854864391, -299.9090924074131408, -210.2361428286349110 ) ) ;
#51818 = CARTESIAN_POINT ( 'NONE',  ( -8.314775077069059606, -281.3487446853740153, -337.8791237368803309 ) ) ;
#51819 = CIRCLE ( 'NONE', #60895, 25.00000000000000355 ) ;
#51820 = CARTESIAN_POINT ( 'NONE',  ( -108.0217867114887866, -276.2192798760343067, -296.0938644756075746 ) ) ;
#51821 = CARTESIAN_POINT ( 'NONE',  ( -65.94916478938755233, -272.1644697477332784, -199.6058535279562705 ) ) ;
#51822 = CARTESIAN_POINT ( 'NONE',  ( 33.93500357570439974, -274.6862255737179339, -254.0716954391058948 ) ) ;
#51823 = CARTESIAN_POINT ( 'NONE',  ( -22.62087217350328316, -293.7641427854604217, -198.1530507401843124 ) ) ;
#51824 = CARTESIAN_POINT ( 'NONE',  ( 24.63274801200521935, -295.0318049131648763, -309.4766047352536020 ) ) ;
#51825 = CARTESIAN_POINT ( 'NONE',  ( -111.4042624983455170, -286.3047787658018137, -270.9392790060217635 ) ) ;
#51826 = CARTESIAN_POINT ( 'NONE',  ( 36.50838846416730377, -294.7293692528860447, -250.6951106122827753 ) ) ;
#51827 = CARTESIAN_POINT ( 'NONE',  ( 37.83751610972370116, -294.6886994617340179, -256.1701448061610336 ) ) ;
#51828 = CARTESIAN_POINT ( 'NONE',  ( -68.51926662613033159, -295.3068697202317594, -336.3821168181235635 ) ) ;
#51829 = CARTESIAN_POINT ( 'NONE',  ( -110.6112468135569742, -292.3459322671900509, -286.4386582921183617 ) ) ;
#51830 = CARTESIAN_POINT ( 'NONE',  ( -101.4179626534740635, -284.1557502113835767, -313.1561121816219497 ) ) ;
#51831 = CARTESIAN_POINT ( 'NONE',  ( -35.49079075278447704, -296.1550023229804083, -194.8017099911895684 ) ) ;
#51832 = CARTESIAN_POINT ( 'NONE',  ( -112.5255515072295935, -284.1775553355857937, -286.9860539624092439 ) ) ;
#51833 = CARTESIAN_POINT ( 'NONE',  ( -105.7693302352541735, -280.1383373422133900, -300.3151256840215524 ) ) ;
#51834 = CARTESIAN_POINT ( 'NONE',  ( -109.8107469201079169, -283.5007667540454008, -258.6468452431744254 ) ) ;
#51835 = CARTESIAN_POINT ( 'NONE',  ( 33.95594074649907412, -285.2494619234425954, -246.9215409384524378 ) ) ;
#51836 = CARTESIAN_POINT ( 'NONE',  ( -110.5315628778188994, -276.9415308877714210, -250.7266713465869259 ) ) ;
#51837 = CARTESIAN_POINT ( 'NONE',  ( -112.8392349625790274, -266.9846182459017427, -270.2902299390011081 ) ) ;
#51838 = CARTESIAN_POINT ( 'NONE',  ( -94.16595011483481414, -284.7089361065579283, -224.4175175083425415 ) ) ;
#51839 = CARTESIAN_POINT ( 'NONE',  ( 33.94922476129675459, -282.3984064311338784, -242.1876307228529868 ) ) ;
#51840 = CARTESIAN_POINT ( 'NONE',  ( -62.69728083778057481, -288.4328759412251770, -342.8736287742139552 ) ) ;
#51841 = CARTESIAN_POINT ( 'NONE',  ( -96.42107494180385174, -279.4994528838173551, -318.5070877323978493 ) ) ;
#51842 = CARTESIAN_POINT ( 'NONE',  ( 10.23258619427804206, -277.7270409929954553, -330.3452673534020505 ) ) ;
#51843 = CARTESIAN_POINT ( 'NONE',  ( -76.82007195183167880, -279.3409834169878536, -208.8968036737456373 ) ) ;
#51844 = CARTESIAN_POINT ( 'NONE',  ( 8.317561934251690658, -276.6604562315231419, -211.3096269979002386 ) ) ;
#51845 = CARTESIAN_POINT ( 'NONE',  ( 38.06190843432031556, -293.3562701668817567, -254.6985520459939494 ) ) ;
#51846 = CARTESIAN_POINT ( 'NONE',  ( 20.95915198056814077, -284.9047667132333572, -223.4255745101119714 ) ) ;
#51847 =( BOUNDED_SURFACE ( )  B_SPLINE_SURFACE ( 3, 2, ( 
 ( #85146, #56284, #77113 ),
 ( #93188, #78065, #6090 ),
 ( #63410, #78528, #20761 ),
 ( #91772, #20300, #49633 ),
 ( #28340, #13666, #70958 ),
 ( #41089, #55811, #49172 ),
 ( #92712, #26924, #13208 ),
 ( #42518, #35442, #86072 ) ),
 .UNSPECIFIED., .F., .F., .F. ) 
 B_SPLINE_SURFACE_WITH_KNOTS ( ( 4, 2, 2, 4 ),
 ( 3, 3 ),
 ( 0.000000000000000000, 0.004223792520792201549, 0.006335688781188302324, 0.008447585041584403098 ),
 ( 0.000000000000000000, 1.000000000000000000 ),
 .UNSPECIFIED. ) 
 GEOMETRIC_REPRESENTATION_ITEM ( )  RATIONAL_B_SPLINE_SURFACE ( (
 ( 1.000000000000000000, 0.7071067811865475727, 1.000000000000000000),
 ( 1.000000000000000000, 0.7191403781184984023, 1.000000000000000000),
 ( 1.000000000000000000, 0.7377564866452918091, 1.000000000000000000),
 ( 1.000000000000000000, 0.7710512730019563055, 1.000000000000000000),
 ( 1.000000000000000000, 0.7830816923593915124, 1.000000000000000000),
 ( 1.000000000000000000, 0.8079768302257757107, 1.000000000000000000),
 ( 1.000000000000000000, 0.8207366415442810537, 1.000000000000000000),
 ( 1.000000000000000000, 0.8333723006565931790, 1.000000000000000000) ) ) 
 REPRESENTATION_ITEM ( '' )  SURFACE ( )  );
#51848 = CARTESIAN_POINT ( 'NONE',  ( -36.40884667172176847, -293.6637864842886643, -194.1539289451806667 ) ) ;
#51849 = VECTOR ( 'NONE', #83854, 1000.000000000000000 ) ;
#51850 = CARTESIAN_POINT ( 'NONE',  ( 1.722969254557689123, -293.4369771981951658, -332.4549142219471491 ) ) ;
#51851 = CARTESIAN_POINT ( 'NONE',  ( 19.70762346661165410, -293.8627343345103782, -315.9602349079602277 ) ) ;
#51852 =( BOUNDED_CURVE ( )  B_SPLINE_CURVE ( 3, ( #77939, #63749, #13083, #41921 ),
 .UNSPECIFIED., .F., .F. ) 
 B_SPLINE_CURVE_WITH_KNOTS ( ( 4, 4 ),
 ( 4.278565243615663150, 4.712388980384691450 ),
 .UNSPECIFIED. ) 
 CURVE ( )  GEOMETRIC_REPRESENTATION_ITEM ( )  RATIONAL_B_SPLINE_CURVE ( ( 1.000000000000000000, 0.9843778111405747655, 0.9843778111405747655, 1.000000000000000000 ) ) 
 REPRESENTATION_ITEM ( '' )  );
#51853 = CARTESIAN_POINT ( 'NONE',  ( -112.5621054832894998, -291.4433097802354951, -285.3736299110723280 ) ) ;
#51854 = CARTESIAN_POINT ( 'NONE',  ( -1.923946207189996205, -281.1859637584270786, -206.4121119265851121 ) ) ;
#51855 = CARTESIAN_POINT ( 'NONE',  ( -76.30293345726610710, -272.6037346133413735, -204.1571100663524589 ) ) ;
#51856 = CARTESIAN_POINT ( 'NONE',  ( 23.21233099692946666, -288.8381278299563064, -317.7798135117720335 ) ) ;
#51857 = CARTESIAN_POINT ( 'NONE',  ( 22.41386763608326405, -280.3244136636627672, -316.9608001777151003 ) ) ;
#51858 = CARTESIAN_POINT ( 'NONE',  ( -3.066332952619674312, -288.9450693959109344, -339.3028311170559732 ) ) ;
#51859 = CARTESIAN_POINT ( 'NONE',  ( -30.53353787668844177, -286.4737532708497270, -197.6072347239738178 ) ) ;
#51860 = CARTESIAN_POINT ( 'NONE',  ( 84.21812867672285563, 83.45443861182893386, -302.1763853415790209 ) ) ;
#51861 = CARTESIAN_POINT ( 'NONE',  ( -84.98320358907332661, -218.2615186942531409, -350.7060260155240030 ) ) ;
#51862 = CARTESIAN_POINT ( 'NONE',  ( 173.1604602154851875, 240.6435161624839338, -177.0232263525105907 ) ) ;
#51863 = CARTESIAN_POINT ( 'NONE',  ( -72.19765763824351268, -278.7756547176378490, -206.0364418984405006 ) ) ;
#51864 = CARTESIAN_POINT ( 'NONE',  ( -108.1222861304432854, -277.2214165994359405, -289.4486720284914441 ) ) ;
#51865 = CARTESIAN_POINT ( 'NONE',  ( -114.3203984661416399, -272.2547862396379514, -267.4902059702777706 ) ) ;
#51866 = CARTESIAN_POINT ( 'NONE',  ( 26.98300397726301725, -24.65525921013767885, -342.2912574563407020 ) ) ;
#51867 = ADVANCED_FACE ( 'NONE', ( #93300 ), #28450, .T. ) ;
#51868 = CARTESIAN_POINT ( 'NONE',  ( -19.87315442162139334, -278.8470366021491600, -195.9195587694034941 ) ) ;
#51869 = CARTESIAN_POINT ( 'NONE',  ( -14.07078513763565297, -296.5144743677850556, -342.6967145281109310 ) ) ;
#51870 = CARTESIAN_POINT ( 'NONE',  ( -79.57138049760347087, -291.9569396937159240, -210.6782799074938737 ) ) ;
#51871 = CARTESIAN_POINT ( 'NONE',  ( -76.32360360301103697, -274.4859349289054649, -204.1692798212957314 ) ) ;
#51872 = CARTESIAN_POINT ( 'NONE',  ( -10.55989518150903983, -287.3802701280101815, -338.8552912570969511 ) ) ;
#51873 = CARTESIAN_POINT ( 'NONE',  ( -102.6368702000801676, -273.7356421530424200, -229.7427286533957442 ) ) ;
#51874 = CARTESIAN_POINT ( 'NONE',  ( -109.2762201800415340, -296.8827627635618001, -257.9343392603321945 ) ) ;
#51875 = EDGE_LOOP ( 'NONE', ( #78527, #2418, #92945 ) ) ;
#51876 = CARTESIAN_POINT ( 'NONE',  ( 175.2296996224750103, 275.5000000000000568, 0.000000000000000000 ) ) ;
#51877 = AXIS2_PLACEMENT_3D ( 'NONE', #35860, #86490, #65702 ) ;
#51878 = CARTESIAN_POINT ( 'NONE',  ( -94.82649853260295458, -281.1464848322396506, -221.3023529691275542 ) ) ;
#51879 = CIRCLE ( 'NONE', #89645, 0.5000000000000004441 ) ;
#51880 = VECTOR ( 'NONE', #84152, 1000.000000000000000 ) ;
#51881 = CARTESIAN_POINT ( 'NONE',  ( -110.2751131314128799, -279.7356011958916042, -262.4613132416062626 ) ) ;
#51882 = CARTESIAN_POINT ( 'NONE',  ( -113.3706383089800056, -280.2964112198901034, -271.6143522394123693 ) ) ;
#51883 = CARTESIAN_POINT ( 'NONE',  ( -67.32201083455039736, -272.1315862647464883, -203.0279926872035219 ) ) ;
#51884 = CARTESIAN_POINT ( 'NONE',  ( 210.3152560301384142, 38.32590481451375553, 10.00000000000000000 ) ) ;
#51885 = CARTESIAN_POINT ( 'NONE',  ( 154.1779308144228651, 20.65864417925001817, 13.49368544356955901 ) ) ;
#51886 = CARTESIAN_POINT ( 'NONE',  ( -68.52521708756100338, -279.7972491266701809, -204.3566615074421691 ) ) ;
#51887 = CIRCLE ( 'NONE', #62463, 12.68950434577434372 ) ;
#51888 = CARTESIAN_POINT ( 'NONE',  ( 35.05228750150188688, -276.6824700767942886, -296.2720261306258749 ) ) ;
#51889 = CARTESIAN_POINT ( 'NONE',  ( 28.79185429016951048, -278.0229503667779909, -305.8453205207046040 ) ) ;
#51890 = CARTESIAN_POINT ( 'NONE',  ( -37.14683262218385806, -275.6244569760258400, -346.7846013406943371 ) ) ;
#51891 = ORIENTED_EDGE ( 'NONE', *, *, #88395, .F. ) ;
#51892 = CARTESIAN_POINT ( 'NONE',  ( 199.5287591261953253, 41.61473866538664623, 9.179409580634077415 ) ) ;
#51893 = CARTESIAN_POINT ( 'NONE',  ( 32.06111909379272618, -283.9153081272322083, -299.8484504907859218 ) ) ;
#51894 = CARTESIAN_POINT ( 'NONE',  ( -102.5488586488664993, -290.2002487404811859, -237.0732866943937154 ) ) ;
#51895 = CARTESIAN_POINT ( 'NONE',  ( -46.48513868308838681, -285.2875884870334176, -194.0085782880030933 ) ) ;
#51896 = CARTESIAN_POINT ( 'NONE',  ( -101.2877509435486587, -282.2875545616817021, -307.6287526927116005 ) ) ;
#51898 = CARTESIAN_POINT ( 'NONE',  ( 28.95146729627809634, -285.1795373793448789, -236.3869425068192527 ) ) ;
#51897 = CARTESIAN_POINT ( 'NONE',  ( -38.91573687095960565, -281.6469709578629477, -343.9461045972946067 ) ) ;
#51899 = CARTESIAN_POINT ( 'NONE',  ( -27.52035372606641772, -281.3846391851541853, -197.5726463987835189 ) ) ;
#51900 = CARTESIAN_POINT ( 'NONE',  ( 180.5981353652897496, 255.9489591101111046, -166.9704198444101451 ) ) ;
#51901 = CARTESIAN_POINT ( 'NONE',  ( 10.96949821822724935, -280.7966828342952113, -329.3570384045843298 ) ) ;
#51902 = CARTESIAN_POINT ( 'NONE',  ( 35.47391973830447398, -295.3215238129108116, -252.3920847284757940 ) ) ;
#51903 = CIRCLE ( 'NONE', #48877, 0.4999999999999892308 ) ;
#51904 = CARTESIAN_POINT ( 'NONE',  ( -109.5915464334587881, -279.0569643513442202, -281.4900162715477450 ) ) ;
#51905 = CARTESIAN_POINT ( 'NONE',  ( -54.56975096601541964, -287.8314300844096465, -197.1953972673855162 ) ) ;
#51906 = CARTESIAN_POINT ( 'NONE',  ( 197.8941236165608473, 24.69666864892464986, 9.707778735729039710 ) ) ;
#51907 = CARTESIAN_POINT ( 'NONE',  ( -96.35454364961768192, -293.1163991317904447, -223.1721520866158812 ) ) ;
#51908 = AXIS2_PLACEMENT_3D ( 'NONE', #1883, #16102, #45411 ) ;
#51909 = CARTESIAN_POINT ( 'NONE',  ( -21.24802395708481839, -274.8456881303112596, -343.6674775021141386 ) ) ;
#51910 = CARTESIAN_POINT ( 'NONE',  ( 30.21583466696752751, -287.2251493141621381, -307.0802679876832713 ) ) ;
#51911 = CARTESIAN_POINT ( 'NONE',  ( 35.62584744216544408, -292.1005805504409523, -281.7463104529301177 ) ) ;
#51912 = CARTESIAN_POINT ( 'NONE',  ( -68.26003287896597271, -276.1517906428187530, -337.0480445774149985 ) ) ;
#51913 = CARTESIAN_POINT ( 'NONE',  ( -109.8026360077661110, -294.4824546312578377, -286.4942595045956182 ) ) ;
#51914 = CARTESIAN_POINT ( 'NONE',  ( -70.17783218354340136, -290.8093332610928883, -336.1248361181010864 ) ) ;
#51915 =( NAMED_UNIT ( * ) PLANE_ANGLE_UNIT ( ) SI_UNIT ( $, .RADIAN. ) );
#51916 = CARTESIAN_POINT ( 'NONE',  ( 196.0143093133018510, 20.19615242270630517, -11.99999999999943867 ) ) ;
#51917 = CARTESIAN_POINT ( 'NONE',  ( 20.79489701036722238, -291.3594542414228385, -220.9160160474684744 ) ) ;
#51918 = CARTESIAN_POINT ( 'NONE',  ( -7.954914001910267096, -288.0438491317030980, -202.6643143814241341 ) ) ;
#51919 = CARTESIAN_POINT ( 'NONE',  ( -110.6491946599201839, -289.0464139752578490, -250.3121678261010459 ) ) ;
#51920 = CARTESIAN_POINT ( 'NONE',  ( -3.075960133487551929, -290.0157804865847879, -335.5423201903118411 ) ) ;
#51921 = CARTESIAN_POINT ( 'NONE',  ( 139.6539576904058606, 132.0000000000000568, 10.50000000000000000 ) ) ;
#51922 = CARTESIAN_POINT ( 'NONE',  ( -31.84905003557559411, -289.7840476326607018, -343.3668567379307319 ) ) ;
#51923 = CARTESIAN_POINT ( 'NONE',  ( -78.55583616408829073, -297.5840318635425206, -333.4467882404397301 ) ) ;
#51924 = CARTESIAN_POINT ( 'NONE',  ( 41.08708295871279859, -293.9068999365417199, -507.6442049081570076 ) ) ;
#51925 = CARTESIAN_POINT ( 'NONE',  ( 33.67998897336980946, -289.1251258290616875, -299.2066293557593326 ) ) ;
#51926 = CARTESIAN_POINT ( 'NONE',  ( -108.9780180173413981, -276.8747278547912174, -246.8152435183763771 ) ) ;
#51927 = CARTESIAN_POINT ( 'NONE',  ( -45.27541442975697095, -280.2876777570410809, -193.7392158406236717 ) ) ;
#51928 = CARTESIAN_POINT ( 'NONE',  ( -67.35030184351538196, -279.3359297978559539, -199.4722746103293787 ) ) ;
#51929 = CARTESIAN_POINT ( 'NONE',  ( -65.82993802584303467, -283.6794743266306682, -200.9270235732126650 ) ) ;
#51930 = DIRECTION ( 'NONE',  ( 0.000000000000000000, 0.000000000000000000, -1.000000000000000000 ) ) ;
#51931 = CARTESIAN_POINT ( 'NONE',  ( -39.71742228385635798, -278.1616160560209323, -196.1512067622547306 ) ) ;
#51932 = CARTESIAN_POINT ( 'NONE',  ( -98.18143222490674304, -281.9539909847155172, -314.3059858516032818 ) ) ;
#51933 = DIRECTION ( 'NONE',  ( 0.000000000000000000, 1.000000000000000000, 0.000000000000000000 ) ) ;
#51934 = CARTESIAN_POINT ( 'NONE',  ( -111.4082183218339424, -277.2643426227267014, -251.9538567227673695 ) ) ;
#51935 = CARTESIAN_POINT ( 'NONE',  ( 9.462241287838949688, -300.1685837963163408, -196.6554053896869618 ) ) ;
#51936 = CARTESIAN_POINT ( 'NONE',  ( -90.23494134184763027, -282.6992769371827308, -325.9658973063937424 ) ) ;
#51937 = CARTESIAN_POINT ( 'NONE',  ( -64.63850758792814588, -274.4892669104845027, -202.4691422519154003 ) ) ;
#51938 = CARTESIAN_POINT ( 'NONE',  ( -103.7266816256837814, -274.4738267847678230, -232.4178644756300969 ) ) ;
#51939 = CARTESIAN_POINT ( 'NONE',  ( 35.60834090647416161, -275.1632275029686525, -266.1419785265910036 ) ) ;
#51940 = CARTESIAN_POINT ( 'NONE',  ( -35.57874820471536026, -297.0302193861775208, -345.3532376387585714 ) ) ;
#51941 = CARTESIAN_POINT ( 'NONE',  ( -98.15830030560384500, -290.0881284591212648, -317.5876057556349110 ) ) ;
#51942 = CARTESIAN_POINT ( 'NONE',  ( -56.17367249863987411, -277.8913964011774169, -197.1315337419543994 ) ) ;
#51943 = CARTESIAN_POINT ( 'NONE',  ( -108.3663174189062346, -290.7637549701123589, -240.6205103361294562 ) ) ;
#51944 = CARTESIAN_POINT ( 'NONE',  ( -88.83499678121414433, -288.8561930924760759, -322.4365329848433817 ) ) ;
#51945 = CARTESIAN_POINT ( 'NONE',  ( 35.15657629717884447, -291.7988961774175323, -289.5705054500083975 ) ) ;
#51946 = ORIENTED_EDGE ( 'NONE', *, *, #30285, .T. ) ;
#51947 = CARTESIAN_POINT ( 'NONE',  ( 153.8109486292483439, 20.54314272855871337, 10.84972530314838579 ) ) ;
#51948 = CIRCLE ( 'NONE', #53515, 0.5000000000000004441 ) ;
#51949 = CARTESIAN_POINT ( 'NONE',  ( -99.76093133645639455, -290.5823294157507348, -232.3897074618980128 ) ) ;
#51950 = FACE_OUTER_BOUND ( 'NONE', #80554, .T. ) ;
#51951 = CARTESIAN_POINT ( 'NONE',  ( 16.12668598135667608, -287.7298505218980154, -215.2797971977761620 ) ) ;
#51952 = CARTESIAN_POINT ( 'NONE',  ( 27.36219212280431989, -296.4805209788416391, -301.4846348637938149 ) ) ;
#51953 = CARTESIAN_POINT ( 'NONE',  ( -32.04076049171884932, -294.0455973034375461, -346.9557935645869406 ) ) ;
#51954 = CARTESIAN_POINT ( 'NONE',  ( -1.847961186025400826, -283.9070645179809844, -338.1364288995113156 ) ) ;
#51955 = CARTESIAN_POINT ( 'NONE',  ( -73.55378684275576973, -285.3905892891570488, -206.9614126473610156 ) ) ;
#51956 = AXIS2_PLACEMENT_3D ( 'NONE', #49813, #573, #29457 ) ;
#51957 = CARTESIAN_POINT ( 'NONE',  ( 35.32677200703673748, -276.7223648358997821, -259.2976522769824328 ) ) ;
#51958 = CARTESIAN_POINT ( 'NONE',  ( 15.46238967421055044, -292.3217590176546992, -323.1933628464565231 ) ) ;
#51959 = CARTESIAN_POINT ( 'NONE',  ( 13.78418317186730668, -273.5835759955461981, -217.6992289062438886 ) ) ;
#51960 = ORIENTED_EDGE ( 'NONE', *, *, #71269, .T. ) ;
#51961 = CARTESIAN_POINT ( 'NONE',  ( 196.4772017995496469, 40.96554989718337225, 12.83327475779042359 ) ) ;
#51962 = CARTESIAN_POINT ( 'NONE',  ( -11.06841617541174472, -294.3857287583105631, -342.7741411782204750 ) ) ;
#51963 = CARTESIAN_POINT ( 'NONE',  ( 24.72137977662807273, -288.9119320753017064, -229.1644530640811581 ) ) ;
#51964 = CARTESIAN_POINT ( 'NONE',  ( -109.1432659898178059, -297.2879090788925396, -297.4557723210269842 ) ) ;
#51965 = AXIS2_PLACEMENT_3D ( 'NONE', #55726, #93099, #84578 ) ;
#51966 = CARTESIAN_POINT ( 'NONE',  ( 22.06958145142643701, -287.6080311963875147, -227.6824515807841465 ) ) ;
#51967 = ADVANCED_FACE ( 'NONE', ( #57799 ), #86185, .F. ) ;
#51968 = CARTESIAN_POINT ( 'NONE',  ( -100.2794831484175404, -277.0281520501196724, -314.3117230024359969 ) ) ;
#51969 = CARTESIAN_POINT ( 'NONE',  ( 39.60961157373269970, -294.2028207387753014, -270.3017462191357367 ) ) ;
#51970 = CARTESIAN_POINT ( 'NONE',  ( 29.26531416745986647, -286.1677361792641250, -306.5791032641260472 ) ) ;
#51971 = CARTESIAN_POINT ( 'NONE',  ( 36.26551863187449243, -293.6024214982456897, -247.8284386489340818 ) ) ;
#51972 = CARTESIAN_POINT ( 'NONE',  ( -79.54638421528115089, -291.7978992803895721, -210.7101114339929779 ) ) ;
#51973 = CARTESIAN_POINT ( 'NONE',  ( 164.6329196456214277, 214.9910457053126720, 23.09031830825856346 ) ) ;
#51974 = AXIS2_PLACEMENT_3D ( 'NONE', #93624, #58141, #86987 ) ;
#51975 = CARTESIAN_POINT ( 'NONE',  ( -112.3417001281054723, -270.5523139186827279, -270.3356821209761165 ) ) ;
#51976 = CARTESIAN_POINT ( 'NONE',  ( 139.1551670580431619, 178.0905500625548257, -238.3682463250823389 ) ) ;
#51977 = CARTESIAN_POINT ( 'NONE',  ( 38.94646215847269133, -289.0510653369147462, -268.6806282160406454 ) ) ;
#51978 = CARTESIAN_POINT ( 'NONE',  ( 13.84574458161073807, -290.1952119285918457, -206.2264541496106460 ) ) ;
#51979 = VERTEX_POINT ( 'NONE', #71072 ) ;
#51980 = CARTESIAN_POINT ( 'NONE',  ( -10.87695737206971103, -281.6192572698207641, -338.7804342335923593 ) ) ;
#51981 = CARTESIAN_POINT ( 'NONE',  ( -97.91489887575750117, -277.5836653927943871, -317.8651376559970458 ) ) ;
#51982 = CARTESIAN_POINT ( 'NONE',  ( 1.325988064423260893, -282.5696769496167917, -206.2321321975770729 ) ) ;
#51983 = CARTESIAN_POINT ( 'NONE',  ( -111.0079197358586214, -274.0791632895269458, -270.3805604919635925 ) ) ;
#51984 = CARTESIAN_POINT ( 'NONE',  ( -52.04200835963407457, -284.4424090379778249, -195.3237669500531979 ) ) ;
#51985 = CARTESIAN_POINT ( 'NONE',  ( 31.48800536491854629, -285.1916654029594724, -241.3425825247887531 ) ) ;
#51986 = CARTESIAN_POINT ( 'NONE',  ( -3.136734348080123524, -276.3594654734198457, -202.7424681462508715 ) ) ;
#51987 = AXIS2_PLACEMENT_3D ( 'NONE', #64364, #93190, #35902 ) ;
#51988 = CARTESIAN_POINT ( 'NONE',  ( -90.09463718365785212, -297.7740240719996905, -219.7405530229252406 ) ) ;
#51989 = ORIENTED_EDGE ( 'NONE', *, *, #62141, .T. ) ;
#51990 = CARTESIAN_POINT ( 'NONE',  ( 18.33514920658155489, -292.9158128532565115, -318.3525001728627899 ) ) ;
#51991 = CARTESIAN_POINT ( 'NONE',  ( -112.3831137694602091, -278.9932285075610707, -287.1569218002958905 ) ) ;
#51992 = CARTESIAN_POINT ( 'NONE',  ( -61.78982515148061339, -277.3787944179788383, -339.1992259225982593 ) ) ;
#51993 = CARTESIAN_POINT ( 'NONE',  ( -9.229482989995716480, -299.3372925595347169, -193.5920387966222620 ) ) ;
#51994 = CARTESIAN_POINT ( 'NONE',  ( -100.2199783508677911, -276.8897549883956799, -314.2680039770266376 ) ) ;
#51995 = CARTESIAN_POINT ( 'NONE',  ( 189.2871950347156940, 271.4890288425742142, -139.5295763810835865 ) ) ;
#51996 = CARTESIAN_POINT ( 'NONE',  ( 34.98873975703526185, -273.8075871038321338, -290.2410010562821299 ) ) ;
#51997 = EDGE_CURVE ( 'NONE', #70265, #70200, #92235, .T. ) ;
#51998 = CARTESIAN_POINT ( 'NONE',  ( -92.26079611022613847, -297.2439526662178650, -323.4883161862781549 ) ) ;
#51999 = CARTESIAN_POINT ( 'NONE',  ( -85.33152481854864391, -275.9090924074130839, -210.2361428286349110 ) ) ;
#52000 = CARTESIAN_POINT ( 'NONE',  ( -30.04969936926732288, -125.9919632799748683, -361.3284013991797110 ) ) ;
#52001 = CARTESIAN_POINT ( 'NONE',  ( -109.7285362384405119, -285.7851450106398943, -258.6896161597846913 ) ) ;
#52002 = CARTESIAN_POINT ( 'NONE',  ( -89.72315216868167909, -285.5386321713770599, -325.4801096333073929 ) ) ;
#52003 = CARTESIAN_POINT ( 'NONE',  ( -57.41442229614335702, -285.1348590589498144, -200.0163390994463271 ) ) ;
#52004 = CARTESIAN_POINT ( 'NONE',  ( -89.66725952945785139, -276.2046951007795315, -322.4767296067391271 ) ) ;
#52005 = CARTESIAN_POINT ( 'NONE',  ( -102.0799160549964881, -286.9026059667446020, -233.9262625125008981 ) ) ;
#52006 = CARTESIAN_POINT ( 'NONE',  ( -59.92789630099822773, -278.2341207688878058, -200.1605263892135724 ) ) ;
#52007 = CARTESIAN_POINT ( 'NONE',  ( 27.04479631321792610, -277.1095257163754013, -305.5187383069378484 ) ) ;
#52008 = CARTESIAN_POINT ( 'NONE',  ( 139.6925840978351516, -0.9999999999999991118, 21.50000000000000000 ) ) ;
#52009 = CARTESIAN_POINT ( 'NONE',  ( -97.89770967483167396, -273.6132652578792204, -229.3934956482949588 ) ) ;
#52010 = CARTESIAN_POINT ( 'NONE',  ( 34.17038043787031398, -281.9962280459111525, -242.1057839266462395 ) ) ;
#52011 = CARTESIAN_POINT ( 'NONE',  ( -30.21434691575735343, -283.4566042545496884, -346.9687399230846836 ) ) ;
#52012 = ORIENTED_EDGE ( 'NONE', *, *, #36276, .T. ) ;
#52013 = ORIENTED_EDGE ( 'NONE', *, *, #37424, .F. ) ;
#52014 = EDGE_CURVE ( 'NONE', #37280, #610, #77705, .T. ) ;
#52015 = DIRECTION ( 'NONE',  ( 0.000000000000000000, 1.000000000000000000, 0.000000000000000000 ) ) ;
#52016 = CARTESIAN_POINT ( 'NONE',  ( -21.26946536258823528, -288.1166067479214234, -196.3206645302480524 ) ) ;
#52017 = CARTESIAN_POINT ( 'NONE',  ( -110.3165667304556479, -288.9444064529691332, -293.5118513105415445 ) ) ;
#52018 = CARTESIAN_POINT ( 'NONE',  ( -110.5355835966617519, -295.7709277141003099, -268.7190931944208501 ) ) ;
#52019 = CARTESIAN_POINT ( 'NONE',  ( 13.21770259551357007, -292.0862236448231783, -212.4209800596536297 ) ) ;
#52020 = CARTESIAN_POINT ( 'NONE',  ( 1.662291437309062703, -287.0001007713279932, -332.8862840670425385 ) ) ;
#52022 = CARTESIAN_POINT ( 'NONE',  ( -36.16788276254150247, -290.3068895503973295, -196.3444405872138248 ) ) ;
#52021 = CARTESIAN_POINT ( 'NONE',  ( 14.48559661566718049, -286.8800168204973033, -322.6038804362329984 ) ) ;
#52023 = CARTESIAN_POINT ( 'NONE',  ( -68.95981749745881473, -286.8319300749523109, -204.1096102392688749 ) ) ;
#52024 = CARTESIAN_POINT ( 'NONE',  ( -109.4082310404863279, -276.8193602355277108, -249.5905673760453851 ) ) ;
#52025 = CARTESIAN_POINT ( 'NONE',  ( 28.20510820910030958, -286.4636447299458837, -309.2205612473138672 ) ) ;
#52026 = CIRCLE ( 'NONE', #5211, 35.00000000000000000 ) ;
#52027 = CARTESIAN_POINT ( 'NONE',  ( -20.90913801687735685, -290.8415605589049164, -343.5920408286086172 ) ) ;
#52028 = CARTESIAN_POINT ( 'NONE',  ( -90.32477883102639282, -287.7990660290804499, -323.7524817515514428 ) ) ;
#52029 = CARTESIAN_POINT ( 'NONE',  ( -7.145544870866885390, -283.5872817200231566, -337.0951936600899330 ) ) ;
#52030 = CARTESIAN_POINT ( 'NONE',  ( -78.60968204390852065, -293.4984325607915139, -207.4738745102226858 ) ) ;
#52031 = DIRECTION ( 'NONE',  ( 0.9693563597868444237, 0.2456588035076248677, 0.000000000000000000 ) ) ;
#52032 = LINE ( 'NONE', #16518, #12558 ) ;
#52033 = CIRCLE ( 'NONE', #23309, 0.5000000000000004441 ) ;
#52034 = CARTESIAN_POINT ( 'NONE',  ( -57.03836387379394068, -299.7203185958575773, -197.3592459473535996 ) ) ;
#52035 = CARTESIAN_POINT ( 'NONE',  ( 30.17443138965062133, -280.3721281583601126, -242.1800301505892890 ) ) ;
#52036 = CARTESIAN_POINT ( 'NONE',  ( 22.11668210822592329, -278.9256080486096039, -224.6269826264428104 ) ) ;
#52037 = CARTESIAN_POINT ( 'NONE',  ( 36.21212761405281810, -293.0309283784445711, -292.7672370760836884 ) ) ;
#52038 = CARTESIAN_POINT ( 'NONE',  ( -100.1284166468338981, -271.3255263694940140, -231.1718051364767632 ) ) ;
#52039 = CARTESIAN_POINT ( 'NONE',  ( 23.63154270290049652, -274.2170828571468633, -313.1529453722600920 ) ) ;
#52040 = CARTESIAN_POINT ( 'NONE',  ( -53.23984682951795833, -296.5753475943707826, -342.1664472209325822 ) ) ;
#52041 =( NAMED_UNIT ( * ) PLANE_ANGLE_UNIT ( ) SI_UNIT ( $, .RADIAN. ) );
#52043 = CARTESIAN_POINT ( 'NONE',  ( -109.8398071270582079, -294.5017166221026628, -293.1642916526852218 ) ) ;
#52042 = CIRCLE ( 'NONE', #59568, 24.00000000000001066 ) ;
#52044 = AXIS2_PLACEMENT_3D ( 'NONE', #92878, #34656, #64036 ) ;
#52045 = CARTESIAN_POINT ( 'NONE',  ( 23.42976964351907299, -295.5512854999624324, -311.9496961033782441 ) ) ;
#52046 = DIRECTION ( 'NONE',  ( -0.01818181818181330636, 0.000000000000000000, 0.9998346970812744816 ) ) ;
#52047 = CARTESIAN_POINT ( 'NONE',  ( -75.73410897391093499, -296.3813508877580034, -332.6987820336518098 ) ) ;
#52048 = DIRECTION ( 'NONE',  ( 0.000000000000000000, 0.000000000000000000, 1.000000000000000000 ) ) ;
#52050 = CARTESIAN_POINT ( 'NONE',  ( -98.44757094535637520, -297.1067407774778530, -230.3312834648069440 ) ) ;
#52049 = CARTESIAN_POINT ( 'NONE',  ( -92.69403831484001444, -283.2843834615023866, -219.1522432961410516 ) ) ;
#52051 = AXIS2_PLACEMENT_3D ( 'NONE', #40810, #77779, #34681 ) ;
#52052 = CARTESIAN_POINT ( 'NONE',  ( -70.47011812078504533, -283.4768185056325933, -339.8846287775337487 ) ) ;
#52053 = CARTESIAN_POINT ( 'NONE',  ( 18.73162842497693958, -284.1737779572890759, -321.0844736798899248 ) ) ;
#52054 = CARTESIAN_POINT ( 'NONE',  ( -68.48831159718943695, -285.3207193823188277, -199.9504898604309062 ) ) ;
#52055 = CARTESIAN_POINT ( 'NONE',  ( -87.13026657072720127, -289.3570090150861347, -214.4243442208789361 ) ) ;
#52056 = CARTESIAN_POINT ( 'NONE',  ( 35.78497577281001440, -272.8380690714490129, -253.7030783399848985 ) ) ;
#52057 = CARTESIAN_POINT ( 'NONE',  ( -43.43851610984211220, -259.1436342284649186, -498.2277075480836288 ) ) ;
#52058 = AXIS2_PLACEMENT_3D ( 'NONE', #70156, #77718, #40751 ) ;
#52059 = CARTESIAN_POINT ( 'NONE',  ( 30.42293856315230371, -285.8562765816720912, -241.7828628820301446 ) ) ;
#52060 = CARTESIAN_POINT ( 'NONE',  ( -100.4341511263454265, -288.8944097929862096, -313.9596860432638437 ) ) ;
#52061 = DIRECTION ( 'NONE',  ( -0.5831039236546632365, 0.7661730729848328370, -0.2701270746362063324 ) ) ;
#52062 = CARTESIAN_POINT ( 'NONE',  ( -105.5088612183088799, -298.5273794335520279, -242.0825295758795335 ) ) ;
#52063 = CARTESIAN_POINT ( 'NONE',  ( -96.37389219554266617, -280.6343093657642385, -221.8247215083474089 ) ) ;
#52065 = CARTESIAN_POINT ( 'NONE',  ( 21.82657927533756492, -281.8175891192346398, -313.1750736549134899 ) ) ;
#52064 = CARTESIAN_POINT ( 'NONE',  ( 26.69459508139615522, -292.1042328646184387, -310.1801234095037785 ) ) ;
#52066 = CARTESIAN_POINT ( 'NONE',  ( -22.09547090729973107, -295.0286947913670588, -345.8366272490243318 ) ) ;
#52067 = CARTESIAN_POINT ( 'NONE',  ( -103.1746369036387705, -282.1404074073567472, -307.5527081642565008 ) ) ;
#52068 = CARTESIAN_POINT ( 'NONE',  ( -112.0540594091986293, -280.6438772246250437, -263.2300970651955936 ) ) ;
#52069 = CARTESIAN_POINT ( 'NONE',  ( -6.677270644135938404, -293.6981034536681818, -336.8675177743754148 ) ) ;
#52070 = CARTESIAN_POINT ( 'NONE',  ( -103.9717408117783322, -271.0130733286139275, -235.4569417527998496 ) ) ;
#52071 = EDGE_LOOP ( 'NONE', ( #41034, #30918, #83467 ) ) ;
#52072 = CARTESIAN_POINT ( 'NONE',  ( 138.6539576904058606, 130.0000000000000568, -10.49999999999999822 ) ) ;
#52073 = CARTESIAN_POINT ( 'NONE',  ( 12.38316218089645027, -282.7286526451247823, -214.6898967956778108 ) ) ;
#52074 = CARTESIAN_POINT ( 'NONE',  ( -107.5167301283792369, -296.3285219301502025, -250.0275593611395095 ) ) ;
#52075 = DIRECTION ( 'NONE',  ( 1.124465274301078034E-16, 1.000000000000000000, 0.000000000000000000 ) ) ;
#52076 = CARTESIAN_POINT ( 'NONE',  ( 21.31550574532286291, -272.4094976428775681, -223.6242672951989618 ) ) ;
#52077 = CARTESIAN_POINT ( 'NONE',  ( -76.34192880043993057, -272.7421316953116275, -204.0943482722793760 ) ) ;
#52078 = CARTESIAN_POINT ( 'NONE',  ( -92.55510678622148646, -291.0659355605029646, -222.6067492847590188 ) ) ;
#52079 = CARTESIAN_POINT ( 'NONE',  ( -94.49035528878833645, -280.7246287572394294, -223.8343625843774873 ) ) ;
#52080 = CARTESIAN_POINT ( 'NONE',  ( -27.20018825017380237, -275.7831862839449855, -197.2097985232132658 ) ) ;
#52081 = CARTESIAN_POINT ( 'NONE',  ( 21.91415590932306046, -283.8015893952864985, -318.2897904512860805 ) ) ;
#52082 = CARTESIAN_POINT ( 'NONE',  ( -74.69471913953061915, -278.3383767729300189, -207.1213605377907072 ) ) ;
#52083 = CARTESIAN_POINT ( 'NONE',  ( -74.99594713437370785, -279.5539075098164403, -335.2237291813885349 ) ) ;
#52084 = ORIENTED_EDGE ( 'NONE', *, *, #37335, .T. ) ;
#52085 = CARTESIAN_POINT ( 'NONE',  ( -96.02631077693312989, -273.0576806687402041, -220.4898750584278844 ) ) ;
#52086 = CARTESIAN_POINT ( 'NONE',  ( 5.309071489689258350, -294.5539435640115471, -209.2878970248545443 ) ) ;
#52087 = DIRECTION ( 'NONE',  ( 0.000000000000000000, 1.000000000000000000, 0.000000000000000000 ) ) ;
#52088 = CARTESIAN_POINT ( 'NONE',  ( 113.5000000000000568, -212.3147208684173108, -422.1836331355066818 ) ) ;
#52089 = ADVANCED_FACE ( 'NONE', ( #63522 ), #20413, .F. ) ;
#52090 = CARTESIAN_POINT ( 'NONE',  ( -53.05655803448743058, -293.3909756074681354, -344.5319182710871928 ) ) ;
#52091 = CARTESIAN_POINT ( 'NONE',  ( -109.9462226093743311, -272.1673443876977672, -262.2019662576451537 ) ) ;
#52092 = LINE ( 'NONE', #81889, #88880 ) ;
#52093 = CARTESIAN_POINT ( 'NONE',  ( 32.68042373087087782, -294.6823127120879349, -240.0360471453423088 ) ) ;
#52094 = CARTESIAN_POINT ( 'NONE',  ( -54.49178911615187815, -276.3376638359844151, -195.3683826091709363 ) ) ;
#52095 = CARTESIAN_POINT ( 'NONE',  ( 37.28218010577872121, -289.6327263608534395, -276.6096840821182923 ) ) ;
#52096 = CARTESIAN_POINT ( 'NONE',  ( -29.54717560293130774, -274.9531837356862525, -344.8395990932402242 ) ) ;
#52097 = CARTESIAN_POINT ( 'NONE',  ( 35.58003269586576778, -277.6658072258828156, -285.3188946530946737 ) ) ;
#52098 = CARTESIAN_POINT ( 'NONE',  ( 20.80352015777070207, -292.2761184254233058, -316.8620439614169300 ) ) ;
#52099 = CARTESIAN_POINT ( 'NONE',  ( -111.2029559986527261, -280.6270680120944121, -253.4844960936010239 ) ) ;
#52100 = VERTEX_POINT ( 'NONE', #14259 ) ;
#52101 = CARTESIAN_POINT ( 'NONE',  ( -38.88978253256773598, -282.7387854184567573, -343.3783446526049943 ) ) ;
#52102 = CARTESIAN_POINT ( 'NONE',  ( -5.086556778380232124, -281.5465589776422348, -200.7831168718684296 ) ) ;
#52103 = CARTESIAN_POINT ( 'NONE',  ( -61.12305409306145521, -282.1489762642081587, -343.2344838265923954 ) ) ;
#52104 = CARTESIAN_POINT ( 'NONE',  ( -71.45548342034609846, -278.4329685435018291, -339.1293519536326357 ) ) ;
#52105 = ADVANCED_FACE ( 'NONE', ( #72023 ), #43117, .T. ) ;
#52106 = CARTESIAN_POINT ( 'NONE',  ( 0.000000000000000000, 0.000000000000000000, 0.000000000000000000 ) ) ;
#52107 = CARTESIAN_POINT ( 'NONE',  ( 36.57202372075288821, -277.3116924913637718, -289.3207904847089935 ) ) ;
#52108 = CARTESIAN_POINT ( 'NONE',  ( 7.450504543161046378, -290.9090924074130839, -326.4764044574609443 ) ) ;
#52109 = ORIENTED_EDGE ( 'NONE', *, *, #88840, .F. ) ;
#52110 = CARTESIAN_POINT ( 'NONE',  ( -108.7663181958378402, -298.2550165232029826, -293.4097201547684790 ) ) ;
#52111 = CARTESIAN_POINT ( 'NONE',  ( -66.70043993297734630, -292.7379041519777161, -203.1875333574132583 ) ) ;
#52112 = CARTESIAN_POINT ( 'NONE',  ( -54.35273317160154249, -275.2916962491779600, -343.0950508506979872 ) ) ;
#52113 = CARTESIAN_POINT ( 'NONE',  ( -3.491738771969169264, -290.3716985335921663, -338.4060939883290757 ) ) ;
#52114 = CARTESIAN_POINT ( 'NONE',  ( -0.03180194821504418734, -291.9115320143268946, -207.4972637735380374 ) ) ;
#52115 = CARTESIAN_POINT ( 'NONE',  ( -17.74605439000924889, -288.3136220129707681, -344.7623113276230242 ) ) ;
#52116 = CYLINDRICAL_SURFACE ( 'NONE', #32521, 2.000000000000001776 ) ;
#52117 = CARTESIAN_POINT ( 'NONE',  ( -109.4421566815660185, -283.1582669041812892, -254.5553008887981719 ) ) ;
#52118 = CARTESIAN_POINT ( 'NONE',  ( -107.1868467685962116, -292.0831787502150974, -295.5110875619837429 ) ) ;
#52119 = CARTESIAN_POINT ( 'NONE',  ( -101.0097886998090786, -282.5275351611591645, -307.4701768336705641 ) ) ;
#52120 = CARTESIAN_POINT ( 'NONE',  ( 34.23691015205043442, -282.6489508754667668, -253.6954037747211714 ) ) ;
#52121 = CARTESIAN_POINT ( 'NONE',  ( -97.09933241152299388, -290.8452386798986709, -318.5673772053381185 ) ) ;
#52122 = CARTESIAN_POINT ( 'NONE',  ( -101.9083808232471284, -278.5791308149198926, -304.5536929876997760 ) ) ;
#52123 = CARTESIAN_POINT ( 'NONE',  ( 10.88079596109349723, -291.4968410130016991, -210.7731203460172651 ) ) ;
#52124 = TOROIDAL_SURFACE ( 'NONE', #41502, 4.499999999999990230, 0.5000000000000000000 ) ;
#52125 = CARTESIAN_POINT ( 'NONE',  ( -1.054859161684753355, -287.3241470186201241, -202.6305931543492704 ) ) ;
#52126 = CARTESIAN_POINT ( 'NONE',  ( 19.58294209324710522, -288.7486735338324593, -322.1408827900740448 ) ) ;
#52127 = CARTESIAN_POINT ( 'NONE',  ( -83.64950768871226217, -285.5630604454160562, -213.8632928156920343 ) ) ;
#52128 = ORIENTED_EDGE ( 'NONE', *, *, #76268, .F. ) ;
#52129 = CARTESIAN_POINT ( 'NONE',  ( 207.7761861081325776, 35.69891260691534285, 14.41714557868295010 ) ) ;
#52130 = CARTESIAN_POINT ( 'NONE',  ( 36.84748508202453365, -295.2163851412431086, -254.9265398853929980 ) ) ;
#52131 = CARTESIAN_POINT ( 'NONE',  ( -106.7262191213813622, -294.8217780197038564, -302.5959872314968493 ) ) ;
#52132 = ADVANCED_FACE ( 'NONE', ( #86649 ), #92830, .T. ) ;
#52133 = CARTESIAN_POINT ( 'NONE',  ( -54.01912345500431201, -276.3301693208909455, -341.7245218092296000 ) ) ;
#52134 = CARTESIAN_POINT ( 'NONE',  ( -100.6620113337510674, -296.4778262537071214, -226.7048401822121946 ) ) ;
#52135 = CARTESIAN_POINT ( 'NONE',  ( 21.87213777095738720, -292.6413495833809861, -314.2294340561453510 ) ) ;
#52136 = CARTESIAN_POINT ( 'NONE',  ( -72.12162973394761423, -295.8254644295049047, -205.0142636252858779 ) ) ;
#52137 = CARTESIAN_POINT ( 'NONE',  ( -49.77098528653240095, -293.0953032023202240, -197.9724993497362391 ) ) ;
#52138 = CARTESIAN_POINT ( 'NONE',  ( 20.41797872154405979, -293.9979210339787414, -225.1960817692392425 ) ) ;
#52139 = CARTESIAN_POINT ( 'NONE',  ( 197.7335303680046650, 24.96166607582781083, 12.00000000000000000 ) ) ;
#52140 = CARTESIAN_POINT ( 'NONE',  ( 33.74409460231963465, -291.8692495823948434, -294.9507337451625517 ) ) ;
#52141 = CARTESIAN_POINT ( 'NONE',  ( -95.90639019058509973, -297.9078327160810886, -317.2339742737384540 ) ) ;
#52142 = CARTESIAN_POINT ( 'NONE',  ( -99.03353974879111377, -290.9492539205385242, -309.8266139531350518 ) ) ;
#52143 = CARTESIAN_POINT ( 'NONE',  ( -68.52251281566290686, -295.8067499217232807, -336.4039708155657991 ) ) ;
#52144 = CARTESIAN_POINT ( 'NONE',  ( -98.91977470617750612, -281.1192740225314992, -226.9267130101486885 ) ) ;
#52145 = CARTESIAN_POINT ( 'NONE',  ( -86.47511438163938635, -278.0713825403471446, -211.6473367878045906 ) ) ;
#52146 = CARTESIAN_POINT ( 'NONE',  ( -81.18545255908168201, -272.8223834378584343, -207.1219326708940400 ) ) ;
#52147 = CARTESIAN_POINT ( 'NONE',  ( 8.665118925045300458, -280.4963604258299483, -328.9477567559068234 ) ) ;
#52148 = CARTESIAN_POINT ( 'NONE',  ( -79.45153693740967071, -277.8940040383092764, -206.7903372285142893 ) ) ;
#52149 = CARTESIAN_POINT ( 'NONE',  ( -39.16387900916373610, -296.7136680926682288, -196.8780653055216590 ) ) ;
#52150 = CARTESIAN_POINT ( 'NONE',  ( 185.2169494693457921, 249.5000000000000568, 22.91843887563416615 ) ) ;
#52151 = CARTESIAN_POINT ( 'NONE',  ( 85.55100297371598117, -296.0521521680024080, -413.1172536214571096 ) ) ;
#52152 = CARTESIAN_POINT ( 'NONE',  ( -111.2596184192468343, -288.3842409438140066, -285.0740933994331954 ) ) ;
#52153 = CARTESIAN_POINT ( 'NONE',  ( -70.63907033646067646, -289.4791001695629689, -339.8038771182556843 ) ) ;
#52154 = CARTESIAN_POINT ( 'NONE',  ( -70.61474256897695057, -275.6145636512155193, -202.9598340352300454 ) ) ;
#52155 = CARTESIAN_POINT ( 'NONE',  ( -111.5581852811192931, -270.6953707836397029, -259.1943451678488941 ) ) ;
#52156 = CARTESIAN_POINT ( 'NONE',  ( -105.6453052450382017, -283.2934342122385942, -305.6734946699169768 ) ) ;
#52157 = CARTESIAN_POINT ( 'NONE',  ( 180.7149167944524493, 8.542400036368780647, 10.00000000000000000 ) ) ;
#52158 = CARTESIAN_POINT ( 'NONE',  ( 37.34402547939911443, -279.4570430021292395, -262.9665257646339001 ) ) ;
#52159 = DIRECTION ( 'NONE',  ( -0.000000000000000000, 1.000000000000000000, -0.000000000000000000 ) ) ;
#52160 = CARTESIAN_POINT ( 'NONE',  ( 2.468690539327602629, -291.3933823303848385, -208.6384096722917718 ) ) ;
#52161 = CARTESIAN_POINT ( 'NONE',  ( -111.2212738335056486, -282.7924386095645559, -262.5977180442585563 ) ) ;
#52162 = CARTESIAN_POINT ( 'NONE',  ( 201.2104617360081704, 41.21457449016152452, 9.999999999999998224 ) ) ;
#52163 = FACE_BOUND ( 'NONE', #27793, .T. ) ;
#52164 = CARTESIAN_POINT ( 'NONE',  ( 16.32392896252184045, -290.8135480300771860, -217.8939504077496281 ) ) ;
#52165 = CARTESIAN_POINT ( 'NONE',  ( -107.0127715417791592, -279.8302058885995507, -294.8548815900806517 ) ) ;
#52166 = CARTESIAN_POINT ( 'NONE',  ( -10.82500723068411652, -283.9191455476691885, -342.2845326428032990 ) ) ;
#52168 = CARTESIAN_POINT ( 'NONE',  ( -62.56287270591849392, -285.7147473351174085, -201.8025206523164456 ) ) ;
#52167 = CARTESIAN_POINT ( 'NONE',  ( 17.06994838128405334, -272.8998257158513638, -217.8580643132578416 ) ) ;
#52169 = AXIS2_PLACEMENT_3D ( 'NONE', #27385, #54843, #85134 ) ;
#52170 = CARTESIAN_POINT ( 'NONE',  ( 33.46976579056012469, -277.2406190765233873, -290.4350344631953362 ) ) ;
#52171 = CARTESIAN_POINT ( 'NONE',  ( -36.45397935899352149, -277.8436159201864371, -343.5297038731206385 ) ) ;
#52172 = EDGE_CURVE ( 'NONE', #59332, #5855, #63559, .T. ) ;
#52173 = CARTESIAN_POINT ( 'NONE',  ( -92.46748606184532093, -287.2637938610868105, -219.4307883144246318 ) ) ;
#52174 = EDGE_LOOP ( 'NONE', ( #42660, #14404, #70718 ) ) ;
#52175 = CARTESIAN_POINT ( 'NONE',  ( 175.2296996224750103, 20.00000000000000000, 24.00000000000000355 ) ) ;
#52176 = CARTESIAN_POINT ( 'NONE',  ( -114.3096149042389129, -296.4308450680517808, -266.7331628054485577 ) ) ;
#52177 = CARTESIAN_POINT ( 'NONE',  ( -27.64735173274831936, -288.1557945735045223, -196.3485081770893430 ) ) ;
#52178 = CARTESIAN_POINT ( 'NONE',  ( 189.9243309297870610, 275.0000000000000568, 20.22542485937349355 ) ) ;
#52179 = CARTESIAN_POINT ( 'NONE',  ( -2.602324593224659921, -289.9809262143061233, -198.2974183793908196 ) ) ;
#52180 = CARTESIAN_POINT ( 'NONE',  ( -103.1392927002287365, -277.9894602966368780, -230.8603112855608401 ) ) ;
#52181 = CARTESIAN_POINT ( 'NONE',  ( -58.69477911175830087, -290.1803518300372957, -197.2140986884464837 ) ) ;
#52182 = CARTESIAN_POINT ( 'NONE',  ( -62.82058670764900654, -287.2346241981953199, -201.1580543353766188 ) ) ;
#52183 = TOROIDAL_SURFACE ( 'NONE', #62842, 24.50000000000000355, 0.5000000000000000000 ) ;
#52184 = CARTESIAN_POINT ( 'NONE',  ( -60.06577537862530392, -281.5138556556065055, -199.8685097336237391 ) ) ;
#52185 = CARTESIAN_POINT ( 'NONE',  ( 38.09624322570690680, -289.1346567075709117, -282.8374009581613109 ) ) ;
#52186 = CARTESIAN_POINT ( 'NONE',  ( -29.20297966300415382, -284.9493176891267581, -344.9701106552531087 ) ) ;
#52187 = CARTESIAN_POINT ( 'NONE',  ( 20.82164410018379641, -276.4008681280163842, -320.8392292823531307 ) ) ;
#52188 = CARTESIAN_POINT ( 'NONE',  ( -44.70683831060090796, -295.9787234687999558, -196.0290414908731975 ) ) ;
#52189 = CARTESIAN_POINT ( 'NONE',  ( -68.67058123078733445, -279.4849870662441731, -200.0082564251513304 ) ) ;
#52190 = CARTESIAN_POINT ( 'NONE',  ( -106.1015046846996768, -298.8473535845913034, -241.8408887985676472 ) ) ;
#52191 = CARTESIAN_POINT ( 'NONE',  ( 139.6925840978351516, 0.000000000000000000, 22.50000000000000000 ) ) ;
#52192 = CARTESIAN_POINT ( 'NONE',  ( -54.49178911615187815, -276.3376638359844151, -195.3683826091709363 ) ) ;
#52193 = CARTESIAN_POINT ( 'NONE',  ( -2.995253580873811217, -272.7394940055267512, -202.5653733163308061 ) ) ;
#52194 = DIRECTION ( 'NONE',  ( -0.000000000000000000, -1.000000000000000000, -0.000000000000000000 ) ) ;
#52195 = CARTESIAN_POINT ( 'NONE',  ( -69.76195965430177637, -279.1209892610443717, -204.8727229373165812 ) ) ;
#52196 = CARTESIAN_POINT ( 'NONE',  ( -83.35390454241726843, -274.6426911799892423, -209.0502436942386169 ) ) ;
#52197 = CARTESIAN_POINT ( 'NONE',  ( 35.10960980415642751, -280.2881446735348732, -244.8324595290386583 ) ) ;
#52198 = CARTESIAN_POINT ( 'NONE',  ( -58.96405129887069307, -291.0957696810806965, -341.1991667748499140 ) ) ;
#52199 = CARTESIAN_POINT ( 'NONE',  ( -113.5424571414612842, -274.1878846411663062, -267.5437725780381584 ) ) ;
#52200 = CARTESIAN_POINT ( 'NONE',  ( -91.36641757709223555, -298.5090483409860553, -216.0533043404143712 ) ) ;
#52201 = CARTESIAN_POINT ( 'NONE',  ( -36.20316001007722662, -294.0665827789429727, -195.5236517174657536 ) ) ;
#52202 = CARTESIAN_POINT ( 'NONE',  ( 28.45519661566180858, -280.0264956285664084, -306.0093550024717501 ) ) ;
#52203 = CARTESIAN_POINT ( 'NONE',  ( 19.92860285743860516, -282.8106810769454000, -222.7868839446012714 ) ) ;
#52204 = CARTESIAN_POINT ( 'NONE',  ( -95.88742105534811344, -271.2113545362793730, -224.0551208737960849 ) ) ;
#52205 = CARTESIAN_POINT ( 'NONE',  ( -85.58003301266370499, -285.3069691600299507, -329.3484357205357469 ) ) ;
#52206 = CARTESIAN_POINT ( 'NONE',  ( -42.70017646613053586, -288.0415252847731722, -343.5249502488745179 ) ) ;
#52207 = CARTESIAN_POINT ( 'NONE',  ( 104.5201122122490460, 115.5852336579065565, -282.7634610850568038 ) ) ;
#52208 = ORIENTED_EDGE ( 'NONE', *, *, #57188, .F. ) ;
#52209 = CARTESIAN_POINT ( 'NONE',  ( -57.15574300866157387, -287.8775095005001390, -344.2128920102268239 ) ) ;
#52210 = CARTESIAN_POINT ( 'NONE',  ( -23.78541194014374227, -288.5409996045896150, -342.1645875696741541 ) ) ;
#52211 = ORIENTED_EDGE ( 'NONE', *, *, #87897, .T. ) ;
#52212 = CARTESIAN_POINT ( 'NONE',  ( -7.476245505745178654, -287.5141898714292097, -199.6679687439149689 ) ) ;
#52213 = CARTESIAN_POINT ( 'NONE',  ( 17.29855352770658783, -275.1927481479630728, -221.8452031013103749 ) ) ;
#52214 = CARTESIAN_POINT ( 'NONE',  ( 39.29747719142622486, -292.5078404395451912, -273.1769675353560274 ) ) ;
#52215 = CARTESIAN_POINT ( 'NONE',  ( 2.049056795971745615, -283.1906971140581959, -336.4041422583042049 ) ) ;
#52216 = CARTESIAN_POINT ( 'NONE',  ( 37.19251928460440837, -283.2793807728432967, -286.7726113737907099 ) ) ;
#52217 = CARTESIAN_POINT ( 'NONE',  ( -63.90073798441968478, -283.7225086566691061, -342.6131892306777331 ) ) ;
#52218 = CARTESIAN_POINT ( 'NONE',  ( 30.03937217322215503, -281.5080590244675705, -242.2207807027742206 ) ) ;
#52219 = CARTESIAN_POINT ( 'NONE',  ( -102.0455923789670294, -293.6237833571632905, -301.4846348637937581 ) ) ;
#52220 = CARTESIAN_POINT ( 'NONE',  ( -99.79643602748313924, -248.2790206999385418, -334.3247771912284065 ) ) ;
#52221 = ORIENTED_EDGE ( 'NONE', *, *, #24174, .F. ) ;
#52222 = CARTESIAN_POINT ( 'NONE',  ( -105.9420827738617419, -280.1586023711414555, -300.3909596906286197 ) ) ;
#52223 = CARTESIAN_POINT ( 'NONE',  ( -113.0788633804183974, -270.3086391544106846, -296.1849204825808783 ) ) ;
#52224 = CARTESIAN_POINT ( 'NONE',  ( -35.80457197443260497, -297.4204801403503211, -197.2593596909151188 ) ) ;
#52225 = CARTESIAN_POINT ( 'NONE',  ( 37.72250070525240062, -293.2718129439862196, -287.2993256315229473 ) ) ;
#52226 = CARTESIAN_POINT ( 'NONE',  ( -38.36988802025361167, -140.4513536128933708, -361.1260187711026219 ) ) ;
#52228 = CARTESIAN_POINT ( 'NONE',  ( -48.19858638698259767, -287.5923142738738534, -343.4097444477936278 ) ) ;
#52227 = CARTESIAN_POINT ( 'NONE',  ( -36.17716605900034921, -296.6411970502992403, -193.9506182268528107 ) ) ;
#52229 = CARTESIAN_POINT ( 'NONE',  ( -95.73053935388782065, -297.7768386694273204, -316.2044265199338611 ) ) ;
#52230 = CARTESIAN_POINT ( 'NONE',  ( 16.32319716211788929, -288.1495819208435023, -220.1297815052000999 ) ) ;
#52231 = VERTEX_POINT ( 'NONE', #20871 ) ;
#52232 = CARTESIAN_POINT ( 'NONE',  ( -71.95717423407748470, -296.4398537462719219, -338.8781900615294376 ) ) ;
#52233 = CARTESIAN_POINT ( 'NONE',  ( -109.4828918771271447, -285.1979156292162543, -258.7216874095224739 ) ) ;
#52234 = CARTESIAN_POINT ( 'NONE',  ( -107.4036183759300229, -295.7457955590860479, -239.2568745477867367 ) ) ;
#52235 = CARTESIAN_POINT ( 'NONE',  ( 29.33044666762119235, -293.8576570820348479, -232.1644733426883533 ) ) ;
#52236 = EDGE_CURVE ( 'NONE', #25460, #52628, #85725, .T. ) ;
#52237 = CARTESIAN_POINT ( 'NONE',  ( 28.05692516249162693, -294.5760738690443077, -310.9895673690463127 ) ) ;
#52238 = CARTESIAN_POINT ( 'NONE',  ( -91.67457854090307023, -291.4167528935680593, -221.5885660294431716 ) ) ;
#52239 = ORIENTED_EDGE ( 'NONE', *, *, #90876, .T. ) ;
#52240 = CARTESIAN_POINT ( 'NONE',  ( 206.1919228894574303, 35.96217941443950394, 14.00000000000000000 ) ) ;
#52241 = CARTESIAN_POINT ( 'NONE',  ( -32.04153465397340028, -299.9782412895974630, -194.5946519202969966 ) ) ;
#52242 = CARTESIAN_POINT ( 'NONE',  ( 36.10834357068222999, -274.6219025954721928, -292.1582231066766440 ) ) ;
#52243 = EDGE_CURVE ( 'NONE', #90976, #34178, #66752, .T. ) ;
#52244 = ORIENTED_EDGE ( 'NONE', *, *, #80432, .F. ) ;
#52245 = CARTESIAN_POINT ( 'NONE',  ( 21.67938326231145396, -275.7245556980903416, -319.7173599271187641 ) ) ;
#52246 = CARTESIAN_POINT ( 'NONE',  ( -59.69880733101615533, -272.1576865900379971, -199.9755513670415041 ) ) ;
#52247 = CARTESIAN_POINT ( 'NONE',  ( -93.15247091760456044, -281.0997360828169462, -221.3925815079106769 ) ) ;
#52248 = CARTESIAN_POINT ( 'NONE',  ( 29.12608476439344329, -274.1339236686507093, -303.5359506368039320 ) ) ;
#52249 = CARTESIAN_POINT ( 'NONE',  ( -106.6029141340631128, -273.9499625306101507, -246.3379977065959281 ) ) ;
#52250 = CARTESIAN_POINT ( 'NONE',  ( -83.34766954163977459, -274.3447446375503205, -213.3798997989499071 ) ) ;
#52251 = CARTESIAN_POINT ( 'NONE',  ( -112.0758621855516566, -274.4899798628269991, -256.3400642169655157 ) ) ;
#52252 = CARTESIAN_POINT ( 'NONE',  ( -36.92299820561722612, -272.0775152233853760, -194.9943032149767248 ) ) ;
#52253 = CARTESIAN_POINT ( 'NONE',  ( -28.87594990684027252, -295.5935514561290347, -343.0222835012285145 ) ) ;
#52254 = CARTESIAN_POINT ( 'NONE',  ( -39.72616871266622240, -293.6573735594915320, -343.9242381158488797 ) ) ;
#52255 = CARTESIAN_POINT ( 'NONE',  ( 152.4536156746142410, 275.0000000000000568, -14.50000000000000000 ) ) ;
#52256 = CARTESIAN_POINT ( 'NONE',  ( 27.60025669824054972, -276.5867490848583543, -311.7163031328891520 ) ) ;
#52257 = CARTESIAN_POINT ( 'NONE',  ( -19.27367601625923754, -274.4577180917642636, -199.5800088567652608 ) ) ;
#52258 = CIRCLE ( 'NONE', #91589, 1.000000000000000888 ) ;
#52259 = CARTESIAN_POINT ( 'NONE',  ( -78.24457982879074791, -284.1990046914297636, -205.7062441964519337 ) ) ;
#52260 = CARTESIAN_POINT ( 'NONE',  ( -111.0949054073396383, -298.7390324594260278, -255.7864317656489277 ) ) ;
#52261 = DIRECTION ( 'NONE',  ( 0.000000000000000000, 1.000000000000000000, 0.000000000000000000 ) ) ;
#52262 = CARTESIAN_POINT ( 'NONE',  ( -62.60906559795499504, -284.9120442018341350, -201.6473387331715514 ) ) ;
#52263 = CARTESIAN_POINT ( 'NONE',  ( -78.18542002612213082, -281.5999099524242979, -333.4627738237135759 ) ) ;
#52264 = CARTESIAN_POINT ( 'NONE',  ( -107.2283657833909842, -276.4704778003267052, -294.8852725946598525 ) ) ;
#52265 = CARTESIAN_POINT ( 'NONE',  ( -74.32497404582281320, -276.1290275065254605, -333.9819665128457018 ) ) ;
#52266 = CARTESIAN_POINT ( 'NONE',  ( -79.22866505866824127, -281.4875137572931294, -208.0864290716669416 ) ) ;
#52267 = CARTESIAN_POINT ( 'NONE',  ( 29.44099802228070573, -276.3474348901758049, -239.7882390472778980 ) ) ;
#52268 = CARTESIAN_POINT ( 'NONE',  ( 159.4851178187871312, 15.00000000000000000, 10.00000000000000000 ) ) ;
#52269 = CARTESIAN_POINT ( 'NONE',  ( -97.17213311375004992, -271.5898310211052831, -223.1725631474939178 ) ) ;
#52270 = ADVANCED_FACE ( 'NONE', ( #58727, #60129 ), #965, .T. ) ;
#52271 = CARTESIAN_POINT ( 'NONE',  ( -71.69226807176488592, -281.5995509806118093, -203.4882545163977170 ) ) ;
#52272 = CARTESIAN_POINT ( 'NONE',  ( -47.80257052418233599, -229.5268262511776527, 22.50000000000000000 ) ) ;
#52273 = CARTESIAN_POINT ( 'NONE',  ( -62.74083993830809192, -287.6442476405991329, -199.1979400461866305 ) ) ;
#52274 = CARTESIAN_POINT ( 'NONE',  ( 153.9445672679333939, 19.37982107813205701, -11.06488088134649139 ) ) ;
#52275 = CARTESIAN_POINT ( 'NONE',  ( -107.9953965008220251, -288.2242014640054322, -295.6740867377243376 ) ) ;
#52276 = CARTESIAN_POINT ( 'NONE',  ( 165.4421947725420523, 250.5000000000000568, 22.46007009812166544 ) ) ;
#52277 = CARTESIAN_POINT ( 'NONE',  ( -86.35410667279552399, -296.1483796986403263, -215.7267468545307167 ) ) ;
#52278 = CARTESIAN_POINT ( 'NONE',  ( -111.1994714745900978, -288.7887144184945782, -262.8848160411922095 ) ) ;
#52279 = CARTESIAN_POINT ( 'NONE',  ( 176.3450237082407170, 252.7779579681928510, -162.7338909149122799 ) ) ;
#52280 = CARTESIAN_POINT ( 'NONE',  ( -36.42824076990669369, -296.0634301785021307, -195.3614206927910288 ) ) ;
#52281 = CARTESIAN_POINT ( 'NONE',  ( 33.39228819982854901, -286.4003668629079584, -299.1271209836299363 ) ) ;
#52282 = CARTESIAN_POINT ( 'NONE',  ( -65.48099292909800795, -283.9291461649952453, -199.7627751490661581 ) ) ;
#52283 = CARTESIAN_POINT ( 'NONE',  ( -64.07161016993896396, -291.6935386965579937, -202.4173861224734310 ) ) ;
#52284 = CARTESIAN_POINT ( 'NONE',  ( 33.53178848499534581, -283.2371216244124525, -290.1682765343626897 ) ) ;
#52285 = CARTESIAN_POINT ( 'NONE',  ( 35.86453168550522719, -282.3674224830651838, -271.3056627519301287 ) ) ;
#52286 = CARTESIAN_POINT ( 'NONE',  ( -36.08835932941323676, -291.0164317800134768, -345.7187284094392794 ) ) ;
#52287 = CARTESIAN_POINT ( 'NONE',  ( -105.5921610927945693, -273.3461394712598462, -234.6422622789075945 ) ) ;
#52288 = ORIENTED_EDGE ( 'NONE', *, *, #43641, .T. ) ;
#52289 = CARTESIAN_POINT ( 'NONE',  ( -74.96822895289646738, -287.6290991539262905, -335.8863690472172152 ) ) ;
#52290 = CARTESIAN_POINT ( 'NONE',  ( 26.93056093854354671, -274.9945429980666063, -227.9573863380029195 ) ) ;
#52291 = CARTESIAN_POINT ( 'NONE',  ( -70.98410693037212127, -293.5858316258687069, -203.7275283237966335 ) ) ;
#52292 = DIRECTION ( 'NONE',  ( -0.000000000000000000, -0.000000000000000000, -1.000000000000000000 ) ) ;
#52293 = CARTESIAN_POINT ( 'NONE',  ( -37.37352853689063892, -276.5519495502701943, -195.3611179825600175 ) ) ;
#52294 = ADVANCED_FACE ( 'NONE', ( #29844 ), #28731, .T. ) ;
#52295 = CARTESIAN_POINT ( 'NONE',  ( -74.45373774874848039, -275.5444467006205969, -335.7272031572723563 ) ) ;
#52296 = EDGE_CURVE ( 'NONE', #74338, #52100, #23190, .T. ) ;
#52297 = CARTESIAN_POINT ( 'NONE',  ( 201.2104617360081704, 0.000000000000000000, 10.00000000000000000 ) ) ;
#52298 = CARTESIAN_POINT ( 'NONE',  ( -36.53050614715974831, -296.4620263312577890, -194.1613290880058287 ) ) ;
#52299 = CARTESIAN_POINT ( 'NONE',  ( 19.08281540511503138, -274.2429869052108984, -223.8835242907718452 ) ) ;
#52300 = CARTESIAN_POINT ( 'NONE',  ( -109.3924920092680537, -292.2744608631003302, -254.8888478261050352 ) ) ;
#52301 = CARTESIAN_POINT ( 'NONE',  ( -37.56265529339778908, -292.9906090994365968, -197.1136725838293273 ) ) ;
#52302 = CARTESIAN_POINT ( 'NONE',  ( -110.8769012073965854, -286.1972786594106992, -279.2013363439521072 ) ) ;
#52303 = CARTESIAN_POINT ( 'NONE',  ( 35.81091884827876015, -295.2586736805342298, -292.6153884610375258 ) ) ;
#52304 = CARTESIAN_POINT ( 'NONE',  ( 38.33125616875052089, -295.0091159676366601, -281.6261949062842973 ) ) ;
#52305 = CARTESIAN_POINT ( 'NONE',  ( 35.62139719961320594, -293.3548549169972262, -268.0402490001837918 ) ) ;
#52306 = CARTESIAN_POINT ( 'NONE',  ( 35.65105399330508362, -289.3302962857743523, -253.0703076809304264 ) ) ;
#52307 = CARTESIAN_POINT ( 'NONE',  ( 23.40422678958352876, -282.3511815743451052, -317.6997836591381201 ) ) ;
#52308 = CARTESIAN_POINT ( 'NONE',  ( -75.03984912860983059, -295.6343364933470639, -204.8170072491263056 ) ) ;
#52309 = CARTESIAN_POINT ( 'NONE',  ( -83.27417751675818636, -285.2759011029294243, -208.4948925254547873 ) ) ;
#52310 = CARTESIAN_POINT ( 'NONE',  ( 36.64761386858147318, -277.4047072812848000, -260.4905447091874748 ) ) ;
#52311 = CARTESIAN_POINT ( 'NONE',  ( -70.14620202639585500, -284.4049355590382220, -204.6889301401840555 ) ) ;
#52312 = CARTESIAN_POINT ( 'NONE',  ( 35.44225815491537901, -285.3195529179867549, -252.2642655184450575 ) ) ;
#52313 = CARTESIAN_POINT ( 'NONE',  ( -112.0150127718244022, -276.8546106223477068, -257.5469906024507623 ) ) ;
#52314 = CARTESIAN_POINT ( 'NONE',  ( -96.12512592106646991, -239.9971452530988358, -342.0757611934672582 ) ) ;
#52315 = CARTESIAN_POINT ( 'NONE',  ( -110.2892526500924504, -284.1244694689802941, -265.4548301130283789 ) ) ;
#52316 = CARTESIAN_POINT ( 'NONE',  ( 39.24300616143346332, -282.7157161040599931, -267.0591067904675810 ) ) ;
#52317 = CARTESIAN_POINT ( 'NONE',  ( -65.37231033901473154, -288.4683628268691677, -341.8813056416111635 ) ) ;
#52318 = CARTESIAN_POINT ( 'NONE',  ( -59.41361302702041769, -278.9334098876110488, -343.2944510668927478 ) ) ;
#52319 = CARTESIAN_POINT ( 'NONE',  ( -14.71942797581068163, -278.0802905493025605, -343.5023688635482131 ) ) ;
#52320 = CARTESIAN_POINT ( 'NONE',  ( -108.8868216375025071, -278.5775993403344160, -255.7967833659311907 ) ) ;
#52321 = CARTESIAN_POINT ( 'NONE',  ( -108.7778476816431521, -274.8144592959327497, -248.5338331468987860 ) ) ;
#52322 = CARTESIAN_POINT ( 'NONE',  ( 34.43548766501601932, -285.2782388294936595, -249.1483444866740058 ) ) ;
#52323 = VECTOR ( 'NONE', #75624, 1000.000000000000000 ) ;
#52324 = CARTESIAN_POINT ( 'NONE',  ( -71.52909317333094918, -291.0963266965711114, -338.4615039932623404 ) ) ;
#52325 = CARTESIAN_POINT ( 'NONE',  ( 19.06215812625640282, -293.1338711974787543, -317.1887898077374075 ) ) ;
#52326 = VERTEX_POINT ( 'NONE', #8512 ) ;
#52327 = CARTESIAN_POINT ( 'NONE',  ( 35.44517167726820617, -293.2959459824859891, -276.2056692489124430 ) ) ;
#52328 = CARTESIAN_POINT ( 'NONE',  ( -97.23083220015577410, -292.2760525810689956, -222.4572103016551239 ) ) ;
#52329 = CARTESIAN_POINT ( 'NONE',  ( -93.17341507491963171, -279.8734165986069797, -223.1538078118960868 ) ) ;
#52330 = CARTESIAN_POINT ( 'NONE',  ( -37.24013962337803463, -296.9737320793004756, -193.6694850293974923 ) ) ;
#52331 = CARTESIAN_POINT ( 'NONE',  ( 30.27701715302099572, -288.6791610273500055, -307.0924682078160686 ) ) ;
#52332 = CARTESIAN_POINT ( 'NONE',  ( -28.97525765558017596, -289.2822734023411044, -346.9374817757678215 ) ) ;
#52333 = CARTESIAN_POINT ( 'NONE',  ( -87.71215491142604037, -285.6579220070659062, -217.4942590666043429 ) ) ;
#52334 = LINE ( 'NONE', #293, #89808 ) ;
#52335 = CARTESIAN_POINT ( 'NONE',  ( 101.3871863598238150, 116.2727258721154016, -280.9442760304585818 ) ) ;
#52336 = CARTESIAN_POINT ( 'NONE',  ( 64.67481406031001256, 46.43102927970478078, -315.2674948880320471 ) ) ;
#52337 = CARTESIAN_POINT ( 'NONE',  ( 0.9472411158466204073, -275.7245445414006895, -332.7629115109273243 ) ) ;
#52338 = CARTESIAN_POINT ( 'NONE',  ( -109.7996693342661558, -277.3261591556681651, -281.4997342510224598 ) ) ;
#52339 = CARTESIAN_POINT ( 'NONE',  ( 99.05675807372718111, -299.2246248443447598, -193.4335806325171063 ) ) ;
#52340 = CARTESIAN_POINT ( 'NONE',  ( 198.1527406508571403, 281.8181044100605277, -110.6140813440772206 ) ) ;
#52341 = CARTESIAN_POINT ( 'NONE',  ( -34.32739795775894720, -275.6998269976061238, -346.8085656587232961 ) ) ;
#52342 = APPLICATION_CONTEXT ( 'automotive_design' ) ;
#52343 = CARTESIAN_POINT ( 'NONE',  ( 34.53530344557626819, -295.6289451990185171, -295.1734719724599358 ) ) ;
#52344 = CARTESIAN_POINT ( 'NONE',  ( -6.020930759994383763, -292.9676237087123241, -204.3397661662521614 ) ) ;
#52345 = CARTESIAN_POINT ( 'NONE',  ( -60.11001654370966918, -298.5673208123796485, -196.9179546232559801 ) ) ;
#52346 = CARTESIAN_POINT ( 'NONE',  ( 24.64536334402888684, -286.7792410129834479, -309.8433600644539752 ) ) ;
#52347 = CARTESIAN_POINT ( 'NONE',  ( -110.0082557544233026, -273.5211440984238607, -245.2039225932294642 ) ) ;
#52348 = CARTESIAN_POINT ( 'NONE',  ( -101.4663034235060763, -296.2426583400958862, -305.2471503836522970 ) ) ;
#52349 = VERTEX_POINT ( 'NONE', #88515 ) ;
#52350 = CYLINDRICAL_SURFACE ( 'NONE', #65883, 4.999999999999986677 ) ;
#52351 = CARTESIAN_POINT ( 'NONE',  ( -111.8746498547990882, -280.3140671629762437, -282.7769789732384993 ) ) ;
#52352 = CARTESIAN_POINT ( 'NONE',  ( -52.91129460743638191, -282.7540768230894059, -345.7621972615469303 ) ) ;
#52353 = CARTESIAN_POINT ( 'NONE',  ( -102.1236871655778486, -279.1663604890888450, -304.6761325999314636 ) ) ;
#52354 = CARTESIAN_POINT ( 'NONE',  ( -72.35357213905712115, -279.2690556255807337, -337.8155466222253267 ) ) ;
#52355 = CARTESIAN_POINT ( 'NONE',  ( -19.08127780748096214, -272.7711875065089089, -198.9130584666494315 ) ) ;
#52356 = CARTESIAN_POINT ( 'NONE',  ( 196.5880405626493257, 70.38190996880992145, -11.16570917829870702 ) ) ;
#52357 = CARTESIAN_POINT ( 'NONE',  ( 76.08708295871279859, -296.0521521680024080, -430.6442049081568939 ) ) ;
#52358 = CARTESIAN_POINT ( 'NONE',  ( -37.01045736687348153, -280.2230949378517835, -197.3618694742876301 ) ) ;
#52359 = CARTESIAN_POINT ( 'NONE',  ( -4.055529868744314648, -277.4271652916872313, -339.6301157917125124 ) ) ;
#52360 = EDGE_CURVE ( 'NONE', #77270, #21926, #15626, .T. ) ;
#52361 = CARTESIAN_POINT ( 'NONE',  ( -2.376937179892249397, -278.5896319205613167, -336.7121993858632436 ) ) ;
#52362 = CARTESIAN_POINT ( 'NONE',  ( -31.51346126257525881, -275.5547949551692000, -346.6015131596551555 ) ) ;
#52363 = ORIENTED_EDGE ( 'NONE', *, *, #72959, .F. ) ;
#52364 = CARTESIAN_POINT ( 'NONE',  ( 200.3691939011709735, 41.41475569181790206, 9.000000000000000000 ) ) ;
#52365 = CARTESIAN_POINT ( 'NONE',  ( 22.12090015254715070, -284.1641002632627533, -316.6702701252370957 ) ) ;
#52366 = CARTESIAN_POINT ( 'NONE',  ( -72.69603300476974539, -290.7687560346113287, -206.2520816521913218 ) ) ;
#52367 = CARTESIAN_POINT ( 'NONE',  ( -23.79569790784137240, -285.5693231229910225, -194.6114066283914497 ) ) ;
#52368 = CARTESIAN_POINT ( 'NONE',  ( -70.69132299255099383, -281.7379893869597822, -336.4493165470716463 ) ) ;
#52370 = CARTESIAN_POINT ( 'NONE',  ( -1.471439006538290517, -284.6110733983196042, -205.0756838971511797 ) ) ;
#52369 = CARTESIAN_POINT ( 'NONE',  ( -13.35431244945859142, -281.3092974053558919, -339.9851159264639477 ) ) ;
#52371 = CARTESIAN_POINT ( 'NONE',  ( -5.399483264460136489, -281.6871709029481394, -204.2791591125973696 ) ) ;
#52372 = CARTESIAN_POINT ( 'NONE',  ( -109.8772534207676301, -270.7993796934649140, -251.0944607303940472 ) ) ;
#52373 = CARTESIAN_POINT ( 'NONE',  ( 20.98438742906629528, -280.6192550429955190, -319.3969000997288958 ) ) ;
#52374 = CARTESIAN_POINT ( 'NONE',  ( 26.34034625178250622, -295.0190670008250322, -230.6448913260919653 ) ) ;
#52375 = CARTESIAN_POINT ( 'NONE',  ( -91.03709241739313995, -278.4914154407168780, -320.0401568655017854 ) ) ;
#52376 = CARTESIAN_POINT ( 'NONE',  ( -67.78222292530867321, -287.6537837865798792, -201.6200634679121606 ) ) ;
#52377 = CARTESIAN_POINT ( 'NONE',  ( 151.6545379164648750, 20.00000000000000000, 4.874475407329899923 ) ) ;
#52378 = CARTESIAN_POINT ( 'NONE',  ( -98.06227083150329804, -293.0817304693117649, -225.3691499501454416 ) ) ;
#52379 = CARTESIAN_POINT ( 'NONE',  ( 17.03074158712967190, -274.2768656515434600, -322.0199819911745180 ) ) ;
#52380 = CARTESIAN_POINT ( 'NONE',  ( -6.993132136467158588, -287.8611281778326543, -340.9665677939642592 ) ) ;
#52381 = CARTESIAN_POINT ( 'NONE',  ( 30.60013466689604655, -291.5677956961148993, -241.4145391574006112 ) ) ;
#52382 = CARTESIAN_POINT ( 'NONE',  ( 104.1964229570258311, -299.5541904835127980, -195.3611179825600175 ) ) ;
#52383 = CARTESIAN_POINT ( 'NONE',  ( -110.4549175772959870, -277.3411416829256382, -262.4111418263187829 ) ) ;
#52384 = CARTESIAN_POINT ( 'NONE',  ( -109.9829726674479957, -294.8909945743895378, -254.9994061884682708 ) ) ;
#52385 = CARTESIAN_POINT ( 'NONE',  ( -110.1088799110917620, -291.7311299096236326, -280.7556769328962787 ) ) ;
#52386 = CYLINDRICAL_SURFACE ( 'NONE', #80483, 4.025000000000000355 ) ;
#52387 = CARTESIAN_POINT ( 'NONE',  ( 144.7857639756989272, -299.5541904835127980, -193.4639945212225882 ) ) ;
#52388 = CARTESIAN_POINT ( 'NONE',  ( 6.117384586893342302, -291.1101648205416836, -207.6393856486895686 ) ) ;
#52389 = CARTESIAN_POINT ( 'NONE',  ( 32.15957837496912930, -289.4791597784695227, -295.1807211375624433 ) ) ;
#52390 = CARTESIAN_POINT ( 'NONE',  ( -90.90040963242593364, -288.0390466126032720, -324.3372796021014324 ) ) ;
#52391 = CARTESIAN_POINT ( 'NONE',  ( 5.050100288672720872, -288.0627099524260188, -210.1463796360941387 ) ) ;
#52392 = CARTESIAN_POINT ( 'NONE',  ( 29.33919985515026596, -285.8906705383787994, 54.50000000000000711 ) ) ;
#52393 = CARTESIAN_POINT ( 'NONE',  ( 9.125190330691086871, -287.5122677333324077, -213.8506780841118768 ) ) ;
#52394 = CARTESIAN_POINT ( 'NONE',  ( -5.181125409545572325, -296.6108969255783450, -338.5229464285263248 ) ) ;
#52395 = CYLINDRICAL_SURFACE ( 'NONE', #2043, 4.999999999999997335 ) ;
#52396 = CARTESIAN_POINT ( 'NONE',  ( -65.28778883781605202, -290.6143442295254999, -341.7405471317194952 ) ) ;
#52397 = CARTESIAN_POINT ( 'NONE',  ( -101.9873113512920071, -277.0893845098545398, -231.5382513952465615 ) ) ;
#52398 = CARTESIAN_POINT ( 'NONE',  ( -71.55763747030638910, -277.8250961219876558, -339.3177269728706165 ) ) ;
#52399 = CARTESIAN_POINT ( 'NONE',  ( -50.93172707210779038, -279.5497596932047486, -194.5913650523636989 ) ) ;
#52400 = CARTESIAN_POINT ( 'NONE',  ( -61.06194253584868648, -299.7227565946490131, -199.5307572127530591 ) ) ;
#52401 = CARTESIAN_POINT ( 'NONE',  ( -111.1570253307531146, -282.7234030645911957, -257.0112620146076097 ) ) ;
#52402 = CARTESIAN_POINT ( 'NONE',  ( -110.3557390660489546, -272.8426144905440651, -270.3648162637165910 ) ) ;
#52403 = CARTESIAN_POINT ( 'NONE',  ( -43.83593020672741147, -278.1089255674569927, -196.3594393412735712 ) ) ;
#52404 = ADVANCED_FACE ( 'NONE', ( #88033 ), #81622, .F. ) ;
#52405 = CARTESIAN_POINT ( 'NONE',  ( -108.7882805279044049, -282.2570618759681906, -293.2155039428967598 ) ) ;
#52406 = DIRECTION ( 'NONE',  ( 0.000000000000000000, -1.000000000000000000, 0.000000000000000000 ) ) ;
#52407 = CARTESIAN_POINT ( 'NONE',  ( 32.37836650704268493, -274.4314699551513854, -301.3743419256232983 ) ) ;
#52408 =( BOUNDED_CURVE ( )  B_SPLINE_CURVE ( 3, ( #17801, #46654, #75558, #4520 ),
 .UNSPECIFIED., .F., .F. ) 
 B_SPLINE_CURVE_WITH_KNOTS ( ( 4, 4 ),
 ( 4.712388980384689674, 5.553457650952619673 ),
 .UNSPECIFIED. ) 
 CURVE ( )  GEOMETRIC_REPRESENTATION_ITEM ( )  RATIONAL_B_SPLINE_CURVE ( ( 1.000000000000000000, 0.9419139527835179715, 0.9419139527835179715, 1.000000000000000000 ) ) 
 REPRESENTATION_ITEM ( '' )  );
#52409 = CARTESIAN_POINT ( 'NONE',  ( -100.5009135111393448, -298.5909439488834209, -232.2931477166583250 ) ) ;
#52410 = CARTESIAN_POINT ( 'NONE',  ( -79.00338075339101351, -282.5202507145826871, -334.7489807884668949 ) ) ;
#52411 = CARTESIAN_POINT ( 'NONE',  ( -109.1129221040446993, -297.3009943647230671, -284.9940441137471794 ) ) ;
#52412 = CARTESIAN_POINT ( 'NONE',  ( -78.53925624087929691, -274.9343058753559035, -206.0076591605692613 ) ) ;
#52413 = CARTESIAN_POINT ( 'NONE',  ( -87.34469137041550368, -272.9985724966560952, -217.0773419629727528 ) ) ;
#52414 = CARTESIAN_POINT ( 'NONE',  ( 31.68679697324006739, -295.1675051200704729, -240.9014555438631362 ) ) ;
#52415 = CARTESIAN_POINT ( 'NONE',  ( 18.64627367818471271, -288.4407241664070511, -323.2226994342595958 ) ) ;
#52416 = CARTESIAN_POINT ( 'NONE',  ( -90.03608180449151632, -277.3949769852837335, -216.1345633064935612 ) ) ;
#52417 = CARTESIAN_POINT ( 'NONE',  ( -99.87150825291023182, -289.7896485194476099, -315.3172497210196639 ) ) ;
#52418 = CARTESIAN_POINT ( 'NONE',  ( -13.22165112776366236, -287.7897306041386400, -339.5104613209703643 ) ) ;
#52419 = CARTESIAN_POINT ( 'NONE',  ( -17.14018917502054862, -290.3127891147919968, -198.1330098721718400 ) ) ;
#52420 = ORIENTED_EDGE ( 'NONE', *, *, #6914, .F. ) ;
#52421 = CARTESIAN_POINT ( 'NONE',  ( 151.6916247871641303, 20.99999999999999645, 4.896253172919318608 ) ) ;
#52422 = CARTESIAN_POINT ( 'NONE',  ( -106.6276633170962640, -290.3674417480760894, -247.1782849673035116 ) ) ;
#52423 = DIRECTION ( 'NONE',  ( -0.000000000000000000, 1.000000000000000000, -0.000000000000000000 ) ) ;
#52424 = CARTESIAN_POINT ( 'NONE',  ( -68.41652929817374229, -286.5950465038032462, -200.1529442076306111 ) ) ;
#52425 = CARTESIAN_POINT ( 'NONE',  ( -67.68488546085839630, -285.9805209788416391, -333.4427485647536855 ) ) ;
#52426 = CARTESIAN_POINT ( 'NONE',  ( -64.19513912797437172, -294.4528645062738406, -342.2757411595842427 ) ) ;
#52427 = CARTESIAN_POINT ( 'NONE',  ( -35.89163966851172916, -284.3495241195543031, -346.8672589026031687 ) ) ;
#52428 = CARTESIAN_POINT ( 'NONE',  ( -97.35473082005590584, -284.9647930023663776, -228.7765863489638321 ) ) ;
#52429 = CARTESIAN_POINT ( 'NONE',  ( 32.99318850367090050, -277.1481589334998716, -291.7178459323778839 ) ) ;
#52430 = CARTESIAN_POINT ( 'NONE',  ( -32.01530749876538096, -290.1397599142433705, -195.8936879466484129 ) ) ;
#52431 = CARTESIAN_POINT ( 'NONE',  ( 24.13441779724263014, -273.7944709788256432, -230.2635191818106648 ) ) ;
#52432 = ORIENTED_EDGE ( 'NONE', *, *, #7938, .T. ) ;
#52433 = CARTESIAN_POINT ( 'NONE',  ( 193.6056169066500274, 279.7126221763799094, -126.0203154767880989 ) ) ;
#52434 = CARTESIAN_POINT ( 'NONE',  ( -82.36865183200259821, -287.3521690720007769, -211.0830628928584929 ) ) ;
#52435 = CARTESIAN_POINT ( 'NONE',  ( -113.2975372549769730, -297.7660238535736426, -259.6733947777154299 ) ) ;
#52436 = CARTESIAN_POINT ( 'NONE',  ( -39.98590122183763640, -286.6694679753457535, -197.3070224846128440 ) ) ;
#52437 = CARTESIAN_POINT ( 'NONE',  ( -91.17261100891231251, -276.8530948807335221, -325.1626483146377495 ) ) ;
#52438 = CARTESIAN_POINT ( 'NONE',  ( 23.88902485567300360, -293.5825681142474082, -223.8194447735538688 ) ) ;
#52439 = CARTESIAN_POINT ( 'NONE',  ( -1.532106799640005512, -284.6613288703608760, -203.5930229971604319 ) ) ;
#52440 = CARTESIAN_POINT ( 'NONE',  ( 11.18827304455897576, -294.7345294640700786, -330.1841937565848752 ) ) ;
#52441 = CARTESIAN_POINT ( 'NONE',  ( -28.10788012022588589, -292.5057275594162434, -197.8753908599403530 ) ) ;
#52442 = LINE ( 'NONE', #22628, #26737 ) ;
#52443 = DIRECTION ( 'NONE',  ( -0.000000000000000000, -0.000000000000000000, -1.000000000000000000 ) ) ;
#52444 = CARTESIAN_POINT ( 'NONE',  ( 103.5299684544230132, 114.3122098872502903, -279.6362027374893273 ) ) ;
#52445 = CARTESIAN_POINT ( 'NONE',  ( -49.25574556654544267, -287.4232086373899051, -194.9370262290599953 ) ) ;
#52446 = CARTESIAN_POINT ( 'NONE',  ( -72.08107566293803359, -274.9809262143061233, -342.4248175857292154 ) ) ;
#52447 = EDGE_LOOP ( 'NONE', ( #2040, #34560, #21500, #38478 ) ) ;
#52448 = CARTESIAN_POINT ( 'NONE',  ( -59.05273952577334740, -282.2599783257348349, -340.4348910940807968 ) ) ;
#52449 = CARTESIAN_POINT ( 'NONE',  ( -106.1547724962572943, -278.6641666460085389, -235.7387116239097509 ) ) ;
#52450 = CARTESIAN_POINT ( 'NONE',  ( 3.688413325188839575, -282.6053565908349015, -207.7165416612079127 ) ) ;
#52451 = CARTESIAN_POINT ( 'NONE',  ( 201.3362163961940894, 286.9516950286333667, -97.02954773690071022 ) ) ;
#52452 = CARTESIAN_POINT ( 'NONE',  ( -76.47187148977623394, -282.1391075178447068, -336.0535317128639576 ) ) ;
#52453 = CARTESIAN_POINT ( 'NONE',  ( 27.81515970384150904, -285.0838445413864406, -233.8351088032227381 ) ) ;
#52454 = CARTESIAN_POINT ( 'NONE',  ( -4.385165432208308012, -276.3422400265334318, -202.1253504088959687 ) ) ;
#52455 = CARTESIAN_POINT ( 'NONE',  ( -99.95276298598618325, -297.5633347333634902, -232.6084591510642383 ) ) ;
#52456 = CARTESIAN_POINT ( 'NONE',  ( 26.21077360547631230, -292.7399702983381644, -307.2708261826982152 ) ) ;
#52457 = CARTESIAN_POINT ( 'NONE',  ( -99.35059563998457577, -279.8085729565765973, -224.8613183859665128 ) ) ;
#52458 = CARTESIAN_POINT ( 'NONE',  ( -29.71342446088390332, -276.9530217965064480, -343.0123641852457581 ) ) ;
#52459 = CARTESIAN_POINT ( 'NONE',  ( -114.0325882487032771, -273.6316498053999453, -270.3748343644707006 ) ) ;
#52460 = CARTESIAN_POINT ( 'NONE',  ( -9.337548418294215224, -275.6148612043954245, -341.7562158312675820 ) ) ;
#52461 = CARTESIAN_POINT ( 'NONE',  ( 169.2744399300530347, 8.542400036368780647, 10.00000000000000000 ) ) ;
#52462 = CARTESIAN_POINT ( 'NONE',  ( -81.72547948933774364, -275.6558952928574513, -330.8819030204403475 ) ) ;
#52463 = CARTESIAN_POINT ( 'NONE',  ( -96.93638943534148211, -297.3314612213697501, -318.2052376438608121 ) ) ;
#52464 = CARTESIAN_POINT ( 'NONE',  ( -35.09237171215954731, -55.96374926131387895, -21.50000000000000000 ) ) ;
#52465 = CARTESIAN_POINT ( 'NONE',  ( 85.37101130053461873, 80.99577858023421584, -298.5812782549759845 ) ) ;
#52466 = CARTESIAN_POINT ( 'NONE',  ( -104.3904941616219020, -285.2345786884110908, -300.0037442383627990 ) ) ;
#52467 = CARTESIAN_POINT ( 'NONE',  ( -55.43883764788490964, -285.0420571346780889, -344.1613051428636822 ) ) ;
#52468 = CARTESIAN_POINT ( 'NONE',  ( -81.53361516298525657, -284.7810156614873449, -212.1291051941864225 ) ) ;
#52469 = CARTESIAN_POINT ( 'NONE',  ( -96.74897785680791173, -276.3447727814161681, -314.1683300977257431 ) ) ;
#52470 = CARTESIAN_POINT ( 'NONE',  ( -105.7447925619772207, -286.7947869522911333, -241.3865179874723026 ) ) ;
#52471 = CARTESIAN_POINT ( 'NONE',  ( -41.06705688715102553, -278.4842915597006368, -196.7620047374585113 ) ) ;
#52472 = CARTESIAN_POINT ( 'NONE',  ( 7.781432718798567016, -277.4992812736093697, -328.2023553674400205 ) ) ;
#52473 = DIRECTION ( 'NONE',  ( 0.000000000000000000, 0.000000000000000000, -1.000000000000000000 ) ) ;
#52474 = CARTESIAN_POINT ( 'NONE',  ( -59.50026941607413278, -274.2498251955237833, -200.6878495533262594 ) ) ;
#52475 = CARTESIAN_POINT ( 'NONE',  ( 22.74263381614980162, -281.7121468791281700, -222.4441534035236998 ) ) ;
#52476 = CARTESIAN_POINT ( 'NONE',  ( -24.53764419255239559, -283.3854183337106747, -346.2807504653053456 ) ) ;
#52477 = ORIENTED_EDGE ( 'NONE', *, *, #73694, .T. ) ;
#52478 = EDGE_LOOP ( 'NONE', ( #20361, #10630, #79282, #20760 ) ) ;
#52479 = FACE_OUTER_BOUND ( 'NONE', #3311, .T. ) ;
#52480 = CARTESIAN_POINT ( 'NONE',  ( 21.12168618264349007, -288.7544897939970951, -222.1704763067948249 ) ) ;
#52481 = CARTESIAN_POINT ( 'NONE',  ( -107.9889243777503651, -296.0004932117155931, -251.2978366723341423 ) ) ;
#52482 = CARTESIAN_POINT ( 'NONE',  ( -53.35997526107881583, -291.2006243366212743, -195.0954732389131152 ) ) ;
#52483 = CARTESIAN_POINT ( 'NONE',  ( -10.48933625865610964, -287.1753552467637292, -339.0427926207207179 ) ) ;
#52484 = CARTESIAN_POINT ( 'NONE',  ( -75.03316443154132287, -288.1395540132069755, -333.5797893537370555 ) ) ;
#52485 = CARTESIAN_POINT ( 'NONE',  ( -81.73084617045694245, -286.6372058348181326, -211.9082804357130385 ) ) ;
#52486 = CARTESIAN_POINT ( 'NONE',  ( -109.7922315684898962, -276.8018089381834557, -250.9229145987291076 ) ) ;
#52487 = CARTESIAN_POINT ( 'NONE',  ( -37.52038352759148410, -287.4541964633958173, -346.5738469064804121 ) ) ;
#52488 = CARTESIAN_POINT ( 'NONE',  ( 16.88731185407780444, -288.8241946479845979, -218.4768376535166681 ) ) ;
#52489 = CARTESIAN_POINT ( 'NONE',  ( -104.8777640831846583, -288.1165675301670035, -303.4781241977089508 ) ) ;
#52490 = CARTESIAN_POINT ( 'NONE',  ( -8.390229859892091469, -283.6048060190160527, -337.6308795245256533 ) ) ;
#52491 = CARTESIAN_POINT ( 'NONE',  ( -106.6858705355471955, -292.9302466538327394, -241.3539730976788746 ) ) ;
#52492 = CARTESIAN_POINT ( 'NONE',  ( 82.13248925020795355, -300.8400434547833129, -193.8278775912719993 ) ) ;
#52493 = CARTESIAN_POINT ( 'NONE',  ( -36.93173961908839686, -299.9773941857664568, -194.8009771340476561 ) ) ;
#52494 = CARTESIAN_POINT ( 'NONE',  ( 32.89246609102586660, -280.4788835943680283, -249.8729842779206933 ) ) ;
#52495 = CARTESIAN_POINT ( 'NONE',  ( 10.57332435206023646, -278.7133933265144492, -212.5946024002020636 ) ) ;
#52496 = CARTESIAN_POINT ( 'NONE',  ( 37.30069955418279193, -292.9785815627571424, -288.6554127986520939 ) ) ;
#52497 = CARTESIAN_POINT ( 'NONE',  ( -101.5863744136171789, -271.2899124802105462, -233.5076557777846915 ) ) ;
#52498 = CARTESIAN_POINT ( 'NONE',  ( -41.97007588457124427, -275.1907469621421569, -344.6699407535705859 ) ) ;
#52499 = CARTESIAN_POINT ( 'NONE',  ( -34.26389064143585728, -296.3278239790259931, -343.7897947222320454 ) ) ;
#52500 = CARTESIAN_POINT ( 'NONE',  ( 152.4536156746142410, 250.0000000000000568, -14.50000000000000000 ) ) ;
#52501 = CARTESIAN_POINT ( 'NONE',  ( -76.11793485492106015, -272.1197923858541685, -204.4591959942287644 ) ) ;
#52502 = CARTESIAN_POINT ( 'NONE',  ( -96.63104715675237344, -294.1465636135915247, -317.9079980111311556 ) ) ;
#52503 = CARTESIAN_POINT ( 'NONE',  ( -5.805447809746892673, -293.9003977623427772, -203.8578313996530085 ) ) ;
#52504 = EDGE_CURVE ( 'NONE', #4883, #35594, #59188, .T. ) ;
#52505 = DIRECTION ( 'NONE',  ( -0.000000000000000000, -0.000000000000000000, 1.000000000000000000 ) ) ;
#52506 = CARTESIAN_POINT ( 'NONE',  ( 34.64021106261860439, -294.1818450371639528, -257.2069297958757375 ) ) ;
#52507 = FACE_OUTER_BOUND ( 'NONE', #41035, .T. ) ;
#52509 = CARTESIAN_POINT ( 'NONE',  ( -13.00824282778969199, -294.7271025551924026, -339.2393921967025676 ) ) ;
#52508 = CARTESIAN_POINT ( 'NONE',  ( -108.4173242812693729, -282.8949612528888338, -245.3278910065147329 ) ) ;
#52510 = CARTESIAN_POINT ( 'NONE',  ( 35.60908434820196078, -281.8643890117031674, -295.1679019736784539 ) ) ;
#52511 = CARTESIAN_POINT ( 'NONE',  ( 29.43749453929426352, -283.0057799938489325, -234.8963726358827273 ) ) ;
#52512 = CARTESIAN_POINT ( 'NONE',  ( -78.50757173945926581, -285.1807392696085799, -205.3140941770536188 ) ) ;
#52513 = CARTESIAN_POINT ( 'NONE',  ( -75.90301674169830903, -289.5362158941690609, -206.1675414716499404 ) ) ;
#52514 = LINE ( 'NONE', #81390, #1815 ) ;
#52515 = CARTESIAN_POINT ( 'NONE',  ( 18.15953800471899626, -285.5548350011254115, -222.1858541566391807 ) ) ;
#52516 = CARTESIAN_POINT ( 'NONE',  ( -110.4911888724279549, -289.1798710766777276, -293.5704393380333954 ) ) ;
#52517 = DIRECTION ( 'NONE',  ( -0.000000000000000000, -0.000000000000000000, -1.000000000000000000 ) ) ;
#52518 = CARTESIAN_POINT ( 'NONE',  ( 4.284233765214266576, -296.0805612752665752, -331.3014333836509309 ) ) ;
#52519 = CARTESIAN_POINT ( 'NONE',  ( -113.6426508860114808, -279.9258110459821296, -274.4563841396836779 ) ) ;
#52521 = CARTESIAN_POINT ( 'NONE',  ( 0.4145165703888758491, -280.2366115610857946, -207.8001399213111142 ) ) ;
#52520 = CARTESIAN_POINT ( 'NONE',  ( 7.898142624106161414, -292.4575675126488363, -330.6252319112911664 ) ) ;
#52522 = CARTESIAN_POINT ( 'NONE',  ( -5.795760295993536815, -294.8153886807336903, -340.6025137875776636 ) ) ;
#52523 = CARTESIAN_POINT ( 'NONE',  ( -110.4872666179995946, -282.3897395652596174, -289.3608382218905604 ) ) ;
#52524 = EDGE_CURVE ( 'NONE', #39706, #36049, #87572, .T. ) ;
#52525 = CARTESIAN_POINT ( 'NONE',  ( -85.78348016252591890, -279.7225441534340575, -327.6863160859580262 ) ) ;
#52526 = CARTESIAN_POINT ( 'NONE',  ( 3.939165828551679294, -293.5395901612440070, -330.8532542772171610 ) ) ;
#52527 = CARTESIAN_POINT ( 'NONE',  ( -105.1774863663427766, -270.9772121210194769, -237.9831234665645638 ) ) ;
#52528 = VERTEX_POINT ( 'NONE', #52529 ) ;
#52529 = CARTESIAN_POINT ( 'NONE',  ( 151.4851178187871312, 21.00000000000000000, -3.492110388858666870 ) ) ;
#52530 = CARTESIAN_POINT ( 'NONE',  ( 22.63587310320395218, -282.9224551999581081, -225.9038460735818035 ) ) ;
#52531 = CARTESIAN_POINT ( 'NONE',  ( -109.2037973509218176, -295.8851120624425448, -283.6148179868723673 ) ) ;
#52532 = DIRECTION ( 'NONE',  ( -0.000000000000000000, -1.000000000000000000, -0.000000000000000000 ) ) ;
#52533 = CARTESIAN_POINT ( 'NONE',  ( 31.95455697924147032, -273.4809262143061233, -303.7686719486574702 ) ) ;
#52534 = CARTESIAN_POINT ( 'NONE',  ( -87.92237192801130163, -272.5633859286510869, -212.4478887049433808 ) ) ;
#52535 = CARTESIAN_POINT ( 'NONE',  ( 25.45657604314171962, -289.4495432376438657, -314.1519322168629174 ) ) ;
#52536 = CARTESIAN_POINT ( 'NONE',  ( -100.3050261004794947, -289.8770450642638252, -307.4014418045969705 ) ) ;
#52537 = CARTESIAN_POINT ( 'NONE',  ( -57.31958891093502473, -281.3097404250933096, -199.4274044850136818 ) ) ;
#52538 = CARTESIAN_POINT ( 'NONE',  ( -69.86164106181914235, -275.2166414825958896, -204.1123907548458760 ) ) ;
#52539 = CARTESIAN_POINT ( 'NONE',  ( -22.09703248697899980, -279.0465900044581531, -198.5125239602838008 ) ) ;
#52540 = CARTESIAN_POINT ( 'NONE',  ( 29.83286993179561719, -277.9938789019153091, -303.8336019008612539 ) ) ;
#52541 = ORIENTED_EDGE ( 'NONE', *, *, #83711, .F. ) ;
#52542 = CARTESIAN_POINT ( 'NONE',  ( -67.53368684079607931, -273.5001876856134118, -199.5271999569542345 ) ) ;
#52543 = CARTESIAN_POINT ( 'NONE',  ( -78.06293712174220900, -293.4202074867801002, -208.0466328765600394 ) ) ;
#52544 = FACE_BOUND ( 'NONE', #67699, .T. ) ;
#52545 = CARTESIAN_POINT ( 'NONE',  ( 208.4306832106271088, -44.55766379199612004, 7.500000000000012434 ) ) ;
#52546 = CARTESIAN_POINT ( 'NONE',  ( 38.42173754026815402, -291.6554605458762808, -267.5071506028702970 ) ) ;
#52547 = CARTESIAN_POINT ( 'NONE',  ( 51.70597994816300513, -298.8638448402078893, -197.3452296079273651 ) ) ;
#52548 = LINE ( 'NONE', #45909, #64752 ) ;
#52549 = CARTESIAN_POINT ( 'NONE',  ( -111.3271405602741311, -292.3086944255701951, -251.6305753479940961 ) ) ;
#52550 = CARTESIAN_POINT ( 'NONE',  ( 21.27581636871892101, -277.4090924074130839, -223.5744983911110353 ) ) ;
#52551 = CARTESIAN_POINT ( 'NONE',  ( 23.46680027001436741, -288.9565606152380610, -226.6578009446622559 ) ) ;
#52552 = CARTESIAN_POINT ( 'NONE',  ( 31.96661642615042354, -273.9223669913845356, -298.7191901260448503 ) ) ;
#52553 = CARTESIAN_POINT ( 'NONE',  ( 0.1584299730664475991, -276.4756645730788023, -206.0418528563278073 ) ) ;
#52554 = CARTESIAN_POINT ( 'NONE',  ( -27.89993318475723783, -290.2526553408465588, -196.4705754324701559 ) ) ;
#52555 = CARTESIAN_POINT ( 'NONE',  ( -73.20225697391897768, -281.4423689042412775, -203.6056682192553922 ) ) ;
#52556 = ORIENTED_EDGE ( 'NONE', *, *, #56386, .T. ) ;
#52557 = CARTESIAN_POINT ( 'NONE',  ( -5.996753444133307021, -281.9775826779881527, -336.4156848240585873 ) ) ;
#52558 = CARTESIAN_POINT ( 'NONE',  ( -59.56225951221558290, -278.4130367143945364, -343.7623390193990076 ) ) ;
#52559 = CARTESIAN_POINT ( 'NONE',  ( 15.46863383773208156, -281.1200989619532038, -325.8505525105308038 ) ) ;
#52560 = CARTESIAN_POINT ( 'NONE',  ( -7.963562319901559050, -277.6178267542222216, -341.2960568440491897 ) ) ;
#52561 = CARTESIAN_POINT ( 'NONE',  ( 29.94095155121660312, -277.5429890985238899, -306.4693004799062805 ) ) ;
#52562 = CARTESIAN_POINT ( 'NONE',  ( -21.33282851196159058, -291.3376638359844719, -340.3538533559490702 ) ) ;
#52563 = VERTEX_POINT ( 'NONE', #88968 ) ;
#52564 = CARTESIAN_POINT ( 'NONE',  ( -111.7865451712130493, -298.4300368579363862, -279.8843936647900250 ) ) ;
#52565 = CARTESIAN_POINT ( 'NONE',  ( -96.00745841876324960, -291.0170900445153279, -314.3428957959031322 ) ) ;
#52566 = CARTESIAN_POINT ( 'NONE',  ( -18.62840938020975301, -274.8300442100257328, -342.6221693801379047 ) ) ;
#52567 = CARTESIAN_POINT ( 'NONE',  ( -17.96086906392792315, -290.5657478694196811, -343.8346329294922157 ) ) ;
#52568 = CARTESIAN_POINT ( 'NONE',  ( -49.69780222124557412, -291.2391130690448904, -198.2596040534082249 ) ) ;
#52569 = CARTESIAN_POINT ( 'NONE',  ( -28.99009523785359121, -288.4567781038294356, -346.8984396358637809 ) ) ;
#52570 = CARTESIAN_POINT ( 'NONE',  ( 219.8344101925596021, 35.72494958537217968, 10.00000000000000000 ) ) ;
#52571 = CARTESIAN_POINT ( 'NONE',  ( -71.80027827851007771, -281.9154717984976628, -335.6224910033434981 ) ) ;
#52572 = CARTESIAN_POINT ( 'NONE',  ( -110.9277180711544730, -292.5446068176033805, -260.1828460679031423 ) ) ;
#52573 = CARTESIAN_POINT ( 'NONE',  ( -96.30920432704658651, -283.6466384216956840, -226.1622356147237269 ) ) ;
#52574 = CARTESIAN_POINT ( 'NONE',  ( 33.58513878264707131, -282.6141505130743212, -251.0613363609991495 ) ) ;
#52575 = CARTESIAN_POINT ( 'NONE',  ( -1.898672013780521750, -289.5355096448350309, -338.4537899210238834 ) ) ;
#52576 = CARTESIAN_POINT ( 'NONE',  ( -95.66465954718233888, -279.6623486220472614, -226.3355672370708191 ) ) ;
#52577 = CARTESIAN_POINT ( 'NONE',  ( 17.21763306045860986, -291.6041349281219937, -216.5157116783219067 ) ) ;
#52578 = CARTESIAN_POINT ( 'NONE',  ( -37.99135895101665739, -286.8470348876525691, -193.5253400875681393 ) ) ;
#52579 = CARTESIAN_POINT ( 'NONE',  ( -4.353759592239997644, -289.1213033552859883, -339.8833032786220656 ) ) ;
#52580 = CARTESIAN_POINT ( 'NONE',  ( -109.4980266451586886, -284.5685718249876004, -281.7517358723518441 ) ) ;
#52581 = EDGE_LOOP ( 'NONE', ( #24063, #88414 ) ) ;
#52582 = CARTESIAN_POINT ( 'NONE',  ( 207.0561972617101674, 35.35788477359429294, 14.49999999999999822 ) ) ;
#52583 = CARTESIAN_POINT ( 'NONE',  ( -28.02486418271881163, -294.0294952511274005, -195.1185325640414874 ) ) ;
#52584 = CARTESIAN_POINT ( 'NONE',  ( 37.84373358426017830, -292.0587765759620424, -256.2031226685676870 ) ) ;
#52585 = CARTESIAN_POINT ( 'NONE',  ( -7.422457413245961533, -275.7086466902309780, -337.2060681591815410 ) ) ;
#52586 = CARTESIAN_POINT ( 'NONE',  ( -65.49694695131958611, -297.0422731591007164, -198.7458750182212555 ) ) ;
#52587 = CARTESIAN_POINT ( 'NONE',  ( 26.38259440541440526, -292.5350553551820667, -307.3735758496896437 ) ) ;
#52588 = CARTESIAN_POINT ( 'NONE',  ( -97.69625947043124370, -295.3820592037396864, -227.5207027046176904 ) ) ;
#52589 = CARTESIAN_POINT ( 'NONE',  ( -100.0588241604511381, -292.2794788511437218, -232.2337936940608643 ) ) ;
#52590 = CARTESIAN_POINT ( 'NONE',  ( 27.43763179995663037, -295.0986580454518844, -304.7896572345953246 ) ) ;
#52591 = CARTESIAN_POINT ( 'NONE',  ( 113.5000000000000568, -190.7866584945343504, -447.4016117689005796 ) ) ;
#52592 = CARTESIAN_POINT ( 'NONE',  ( -19.74186261568116407, -292.8263582785700692, -343.4918720160446242 ) ) ;
#52593 = CARTESIAN_POINT ( 'NONE',  ( -106.5187409717126457, -298.1724126029107538, -299.4680911956714340 ) ) ;
#52594 = CARTESIAN_POINT ( 'NONE',  ( -29.13489213650443332, -289.8868512351302229, -343.1351294874123710 ) ) ;
#52595 = CARTESIAN_POINT ( 'NONE',  ( 34.92344219847572617, -277.8063563093791117, -291.7645055544556953 ) ) ;
#52596 = CARTESIAN_POINT ( 'NONE',  ( -72.26665628135998531, -278.2847526583374247, -202.2764089129724141 ) ) ;
#52597 = CARTESIAN_POINT ( 'NONE',  ( -27.00200147216099111, -273.5287749168124947, -194.1079983406012843 ) ) ;
#52598 = CARTESIAN_POINT ( 'NONE',  ( 36.78872309555949016, -279.5371985651728437, -263.0334407236534844 ) ) ;
#52599 = CARTESIAN_POINT ( 'NONE',  ( -101.4352498721113136, -276.4045509919511687, -311.6697826534248748 ) ) ;
#52600 = EDGE_CURVE ( 'NONE', #90042, #92711, #77109, .T. ) ;
#52601 = CARTESIAN_POINT ( 'NONE',  ( -80.45753435868844861, -294.3352919958117582, -329.8780761990958581 ) ) ;
#52602 = CARTESIAN_POINT ( 'NONE',  ( -73.43786540279265296, -275.5738618339977961, -204.5613507086511333 ) ) ;
#52603 = CARTESIAN_POINT ( 'NONE',  ( -32.69282475682609856, -274.7636705991545796, -197.3946117842211549 ) ) ;
#52604 = CARTESIAN_POINT ( 'NONE',  ( 196.5998995412811041, 25.70598842973115694, 11.15476524095018007 ) ) ;
#52605 = CARTESIAN_POINT ( 'NONE',  ( -89.62616398344084701, -289.3399644500694876, -216.0232488371607644 ) ) ;
#52606 = CARTESIAN_POINT ( 'NONE',  ( -54.50161534199090596, -289.2666166408383219, -345.4793849556406826 ) ) ;
#52607 = CARTESIAN_POINT ( 'NONE',  ( -77.87489449231253502, -275.5091014185332483, -207.0595494411959407 ) ) ;
#52608 = CARTESIAN_POINT ( 'NONE',  ( -95.86965410561414558, -295.1944313365081598, -223.7295081601799893 ) ) ;
#52609 = CARTESIAN_POINT ( 'NONE',  ( 4.449280717170755572, -281.7013157469030489, -334.9040171347362502 ) ) ;
#52610 = CARTESIAN_POINT ( 'NONE',  ( 208.6208076322478746, 32.98517505407394168, 10.50000000000000000 ) ) ;
#52611 = CARTESIAN_POINT ( 'NONE',  ( 28.81783187126130485, -280.0219006508491475, -305.7955748485454137 ) ) ;
#52612 = DIRECTION ( 'NONE',  ( 0.000000000000000000, -0.000000000000000000, 1.000000000000000000 ) ) ;
#52613 = CARTESIAN_POINT ( 'NONE',  ( -106.0771239745501475, -289.6903339982882244, -244.4765102920835602 ) ) ;
#52614 = CARTESIAN_POINT ( 'NONE',  ( -83.58232285556076135, -281.8333180403552660, -328.5017928378059651 ) ) ;
#52615 = CARTESIAN_POINT ( 'NONE',  ( 82.64890176555634582, -299.5541904835127980, -195.3611179825600175 ) ) ;
#52616 = CARTESIAN_POINT ( 'NONE',  ( 175.2296996224750103, 275.0000000000000568, 0.000000000000000000 ) ) ;
#52617 = CARTESIAN_POINT ( 'NONE',  ( -22.31570140609487396, -290.2444268900834459, -196.8817330632668927 ) ) ;
#52618 = CARTESIAN_POINT ( 'NONE',  ( -29.60956401823413486, -278.5528922474309752, -343.8064140483295432 ) ) ;
#52619 = CARTESIAN_POINT ( 'NONE',  ( -5.605944055364151524, -283.8490138042897684, -340.0809179424495028 ) ) ;
#52621 = CARTESIAN_POINT ( 'NONE',  ( -14.56600449232711014, -286.3556093030103398, -200.9520061194560867 ) ) ;
#52620 = CARTESIAN_POINT ( 'NONE',  ( -36.92269341036211472, -272.1372436690941754, -194.7894673150107110 ) ) ;
#52622 = CARTESIAN_POINT ( 'NONE',  ( 36.23163741906842006, -276.9574188222558178, -268.8317659534246786 ) ) ;
#52623 = CARTESIAN_POINT ( 'NONE',  ( -35.10247309152077122, -277.8261519372910016, -343.4883194173067977 ) ) ;
#52624 = EDGE_CURVE ( 'NONE', #84200, #36049, #51591, .T. ) ;
#52625 = ADVANCED_FACE ( 'NONE', ( #81404 ), #13598, .T. ) ;
#52626 = CARTESIAN_POINT ( 'NONE',  ( -94.31442759118930041, -287.2286414211441183, -221.5070858983209519 ) ) ;
#52627 = CIRCLE ( 'NONE', #42021, 0.5000000000000004441 ) ;
#52628 = VERTEX_POINT ( 'NONE', #80955 ) ;
#52629 = CARTESIAN_POINT ( 'NONE',  ( 158.6539576904058606, 293.9636489450775230, -9.103929867429224387 ) ) ;
#52630 = CARTESIAN_POINT ( 'NONE',  ( -50.46961047978744119, -295.0485259551674631, -346.2877062656752969 ) ) ;
#52631 = CARTESIAN_POINT ( 'NONE',  ( 196.1072012964043267, 25.48927062411483391, 14.15988601298065674 ) ) ;
#52632 = CARTESIAN_POINT ( 'NONE',  ( -37.37352853689063181, -292.5523547857346784, -350.3611179825600175 ) ) ;
#52633 = CARTESIAN_POINT ( 'NONE',  ( -111.4288308098553273, -277.7221492231461752, -250.4965797437095318 ) ) ;
#52634 = CARTESIAN_POINT ( 'NONE',  ( -11.40617662614166683, -290.7842112735534670, -198.6551916763846179 ) ) ;
#52635 = CARTESIAN_POINT ( 'NONE',  ( -67.85225702386543389, -287.1643463226504309, -203.2804674777293314 ) ) ;
#52636 = CARTESIAN_POINT ( 'NONE',  ( -84.09496531641927675, -281.1598431612854938, -212.9178878779722766 ) ) ;
#52637 = CARTESIAN_POINT ( 'NONE',  ( 4.839166937267678215, -288.0347628429412339, -206.5848362945725967 ) ) ;
#52638 = CARTESIAN_POINT ( 'NONE',  ( 21.77266947861653890, -284.1855163762223242, -316.5183704909322842 ) ) ;
#52639 = CARTESIAN_POINT ( 'NONE',  ( -35.70938148302340664, -277.1989171208280709, -347.3569378957428171 ) ) ;
#52640 = CARTESIAN_POINT ( 'NONE',  ( -99.34835060316936506, -271.1211597243290612, -228.3735661696755983 ) ) ;
#52641 = CARTESIAN_POINT ( 'NONE',  ( -106.1746257757665290, -278.8307409744800225, -235.7310946939329312 ) ) ;
#52642 = CARTESIAN_POINT ( 'NONE',  ( -87.08026348660725091, -299.2731063423513547, -214.9770994351865738 ) ) ;
#52643 = CARTESIAN_POINT ( 'NONE',  ( 180.2288731078812702, 275.5000000000000568, -24.90909090909093848 ) ) ;
#52644 = CARTESIAN_POINT ( 'NONE',  ( -110.4683760289727132, -275.2662352645559167, -253.7030783399848985 ) ) ;
#52645 = CARTESIAN_POINT ( 'NONE',  ( -34.08881529147114975, -296.2320524517635931, -194.5973284279544373 ) ) ;
#52646 = DIRECTION ( 'NONE',  ( 8.659560562354828088E-17, 0.7071067811865561215, -0.7071067811865389130 ) ) ;
#52647 = CARTESIAN_POINT ( 'NONE',  ( -87.14205353033921142, -277.2765237406758843, -323.8205721748724955 ) ) ;
#52648 = CARTESIAN_POINT ( 'NONE',  ( -0.2512162469553667066, -275.7391696561791719, -203.3215459071010116 ) ) ;
#52649 = CARTESIAN_POINT ( 'NONE',  ( 4.407645986672851457, -281.5629186366799672, -334.8429746093233348 ) ) ;
#52650 = CARTESIAN_POINT ( 'NONE',  ( 16.76688925948248965, -290.0293004739678508, -320.9359810329539187 ) ) ;
#52651 = CARTESIAN_POINT ( 'NONE',  ( -103.2607064427807444, -298.5781174793947343, -231.8200814929145110 ) ) ;
#52652 = CARTESIAN_POINT ( 'NONE',  ( -102.7684346936857622, -297.2342641213754177, -310.2026932776382750 ) ) ;
#52653 = CARTESIAN_POINT ( 'NONE',  ( 35.07609064888190176, -295.3094169972781629, -251.5013192430557467 ) ) ;
#52654 = CARTESIAN_POINT ( 'NONE',  ( 36.95692165498365966, -279.6723202598245166, -279.7119766175076165 ) ) ;
#52655 = CARTESIAN_POINT ( 'NONE',  ( -6.188666745529876501, -282.3848272374017938, -202.7394928500793014 ) ) ;
#52656 = CARTESIAN_POINT ( 'NONE',  ( -55.62412464102188636, -295.8950013746932655, -198.1477697394450956 ) ) ;
#52657 = CARTESIAN_POINT ( 'NONE',  ( -82.81497259496194374, -287.0424251864471330, -209.1510349148578882 ) ) ;
#52658 = CARTESIAN_POINT ( 'NONE',  ( -5.671286685325179988, -287.5458573154012925, -336.4762523097759868 ) ) ;
#52659 = CARTESIAN_POINT ( 'NONE',  ( -29.74821284649360109, -125.1331993717982272, -364.1253139031180694 ) ) ;
#52660 = ORIENTED_EDGE ( 'NONE', *, *, #6101, .T. ) ;
#52661 = CARTESIAN_POINT ( 'NONE',  ( -45.97734613929616643, -287.7342121783263451, -346.3350604306444325 ) ) ;
#52662 = CARTESIAN_POINT ( 'NONE',  ( 35.29586074006135021, -287.1202929560498660, -262.8863445504107403 ) ) ;
#52663 = EDGE_LOOP ( 'NONE', ( #63354, #69032, #90855, #24336 ) ) ;
#52664 = CARTESIAN_POINT ( 'NONE',  ( -41.53841591312731651, -284.1833711727791183, -346.9892107964356569 ) ) ;
#52665 = CARTESIAN_POINT ( 'NONE',  ( 15.45914512182664780, -275.1573632520764932, -219.8482788284892990 ) ) ;
#52666 = CARTESIAN_POINT ( 'NONE',  ( -94.47181848533857362, -290.1693203314193283, -219.1982204239498628 ) ) ;
#52667 = CARTESIAN_POINT ( 'NONE',  ( 37.57630530788240009, -281.9857845721157332, -252.9653204307675196 ) ) ;
#52668 = CARTESIAN_POINT ( 'NONE',  ( 10.37423572682743611, -282.2168516784700500, -210.7459696539853553 ) ) ;
#52669 = CARTESIAN_POINT ( 'NONE',  ( -21.72613013204149013, -283.1905272761580932, -345.7394853377573440 ) ) ;
#52670 = CARTESIAN_POINT ( 'NONE',  ( -89.47357884723847121, -279.2925092449667659, -219.1889198564007302 ) ) ;
#52671 = CARTESIAN_POINT ( 'NONE',  ( -20.19161114001082069, -277.7666405000204009, -195.3683826091709363 ) ) ;
#52672 = CARTESIAN_POINT ( 'NONE',  ( 204.1737866480590924, 295.5637011240619927, -68.68209524862845683 ) ) ;
#52673 = ORIENTED_EDGE ( 'NONE', *, *, #55414, .F. ) ;
#52674 = CARTESIAN_POINT ( 'NONE',  ( 34.61601920761162177, -277.2851623686695461, -249.6307470447542016 ) ) ;
#52675 = CARTESIAN_POINT ( 'NONE',  ( -22.99186949233678945, -107.8477965757182204, -362.2362941995334040 ) ) ;
#52676 = CARTESIAN_POINT ( 'NONE',  ( -52.64834823549384168, -297.1995538209649226, -198.8277007655893556 ) ) ;
#52677 = CARTESIAN_POINT ( 'NONE',  ( 37.36369790267395530, -292.8294194253056730, -251.9592048057795353 ) ) ;
#52678 = CARTESIAN_POINT ( 'NONE',  ( 193.8404912568037446, 275.6304219183343207, -124.1201750202075687 ) ) ;
#52680 = CARTESIAN_POINT ( 'NONE',  ( -37.28766759898142169, -287.4513352148392187, -344.1611010333646732 ) ) ;
#52679 = CARTESIAN_POINT ( 'NONE',  ( -77.87441223988015793, -296.0936238627925832, -205.5868519423754321 ) ) ;
#52681 = CARTESIAN_POINT ( 'NONE',  ( -50.67011203268599218, -297.0846205352576135, -343.3900089355659020 ) ) ;
#52682 = CARTESIAN_POINT ( 'NONE',  ( -74.98700277213917786, -286.8544849772890757, -207.2415911555131061 ) ) ;
#52683 = EDGE_LOOP ( 'NONE', ( #74210, #27455, #83059, #15999, #15572 ) ) ;
#52684 = CARTESIAN_POINT ( 'NONE',  ( -64.17268463485460472, -296.3350648556469764, -342.2841218353725026 ) ) ;
#52685 = CARTESIAN_POINT ( 'NONE',  ( -110.2900917439872615, -285.1090053368810686, -265.4673239033900245 ) ) ;
#52686 = CARTESIAN_POINT ( 'NONE',  ( -26.26561591906065729, -296.9828540441263840, -193.7603967612039924 ) ) ;
#52687 = CARTESIAN_POINT ( 'NONE',  ( -68.27316159071216362, -292.4589576487653630, -200.0089986674241800 ) ) ;
#52688 = CARTESIAN_POINT ( 'NONE',  ( 19.36606221550634999, -293.3364986157773160, -218.3634584847602014 ) ) ;
#52689 = CARTESIAN_POINT ( 'NONE',  ( -50.74938228436087684, -289.3947620357002961, -342.1709602780546788 ) ) ;
#52690 = VERTEX_POINT ( 'NONE', #37846 ) ;
#52691 = CARTESIAN_POINT ( 'NONE',  ( 159.3464669004306984, 16.14910309755062556, 9.103988188768894929 ) ) ;
#52692 = CARTESIAN_POINT ( 'NONE',  ( -36.23122460170400672, -299.9263225365933181, -194.5959630375046743 ) ) ;
#52693 = CARTESIAN_POINT ( 'NONE',  ( -32.69129527004988489, -272.9044345745654141, -193.8863948477479369 ) ) ;
#52694 = ADVANCED_FACE ( 'NONE', ( #1879 ), #72343, .T. ) ;
#52695 = ORIENTED_EDGE ( 'NONE', *, *, #9884, .F. ) ;
#52696 = VERTEX_POINT ( 'NONE', #45888 ) ;
#52697 = CARTESIAN_POINT ( 'NONE',  ( 27.59352157778364401, -275.6022134199692459, -311.7268783411288950 ) ) ;
#52698 = VECTOR ( 'NONE', #7789, 1000.000000000000000 ) ;
#52699 = CARTESIAN_POINT ( 'NONE',  ( -54.37663549347558956, -272.2295192979731269, -198.5540752214207032 ) ) ;
#52700 = CARTESIAN_POINT ( 'NONE',  ( -107.4225647998200373, -280.0904514913161734, -295.0023346710380565 ) ) ;
#52701 = CARTESIAN_POINT ( 'NONE',  ( -7.024518934781800006, -274.7896313874917382, -338.1234527071920297 ) ) ;
#52702 = CARTESIAN_POINT ( 'NONE',  ( -84.34080488233216499, -298.5939842164213474, -213.9190915884640560 ) ) ;
#52703 = CARTESIAN_POINT ( 'NONE',  ( -63.40161717392884810, -274.6453448481150872, -201.9057128947075341 ) ) ;
#52704 = CARTESIAN_POINT ( 'NONE',  ( -32.00007760669642920, -299.7180926278506945, -194.1596863099827885 ) ) ;
#52705 = CARTESIAN_POINT ( 'NONE',  ( 22.34581165502161326, -272.9447924783620465, -224.3421961973749319 ) ) ;
#52706 = CARTESIAN_POINT ( 'NONE',  ( 34.81321736065179095, -294.0480334721162876, -258.5542756019498825 ) ) ;
#52707 = CARTESIAN_POINT ( 'NONE',  ( -41.60900291774942872, -290.5722191460443469, -196.8454682842868237 ) ) ;
#52708 = LINE ( 'NONE', #66483, #45787 ) ;
#52709 = CARTESIAN_POINT ( 'NONE',  ( -39.95457795819446289, -277.5764680703449585, -347.2682553160324233 ) ) ;
#52710 = CARTESIAN_POINT ( 'NONE',  ( 35.35420273350267450, -275.8066402417032918, -277.0173715558327672 ) ) ;
#52711 = CARTESIAN_POINT ( 'NONE',  ( 165.1508121697700346, 214.6009552038360084, 22.87850562931658871 ) ) ;
#52712 = CARTESIAN_POINT ( 'NONE',  ( -106.2277704425618197, -283.6668320181299237, -237.0743700481887402 ) ) ;
#52713 = CARTESIAN_POINT ( 'NONE',  ( 20.88308640062745170, -296.2061393548696628, -317.9197665947267524 ) ) ;
#52714 = FACE_OUTER_BOUND ( 'NONE', #6319, .T. ) ;
#52715 = CARTESIAN_POINT ( 'NONE',  ( -89.77145539793603746, -284.4862672667557035, -219.2617449393218578 ) ) ;
#52716 = CARTESIAN_POINT ( 'NONE',  ( -110.7405302030631589, -282.3443717192058102, -286.5672950407857797 ) ) ;
#52717 = CARTESIAN_POINT ( 'NONE',  ( -41.94165185004501950, -275.3507339666684288, -344.2441434208323585 ) ) ;
#52718 = CARTESIAN_POINT ( 'NONE',  ( -7.283448734543601866, -275.2247046621117192, -337.5316207478356318 ) ) ;
#52719 = CARTESIAN_POINT ( 'NONE',  ( 36.55104501111865289, -283.3865060799023468, -257.4477512657309148 ) ) ;
#52720 = CARTESIAN_POINT ( 'NONE',  ( 33.63004823419364442, -277.0029778877860167, -289.0731846822382067 ) ) ;
#52721 = CARTESIAN_POINT ( 'NONE',  ( -23.40286736638519471, -122.5496321078137356, 22.50000000000000000 ) ) ;
#52722 = CARTESIAN_POINT ( 'NONE',  ( -46.76169259700797198, -272.3343199022644399, -194.7456158935853807 ) ) ;
#52723 = CARTESIAN_POINT ( 'NONE',  ( -34.02234085966953359, -282.0939795260514416, -195.2677741847248285 ) ) ;
#52724 = CARTESIAN_POINT ( 'NONE',  ( 195.8698257649199377, 19.45052997590691390, 12.70854403887906514 ) ) ;
#52725 = CARTESIAN_POINT ( 'NONE',  ( 6.684667905823711287, -288.5653779333867419, -208.8882781638876907 ) ) ;
#52726 = CARTESIAN_POINT ( 'NONE',  ( 156.9594811538141244, 18.65395765032456765, -11.57852291560661762 ) ) ;
#52727 = CARTESIAN_POINT ( 'NONE',  ( -108.8813797260759486, -288.2595266195689305, -293.0472744037678581 ) ) ;
#52728 = CARTESIAN_POINT ( 'NONE',  ( 208.6208076322478746, 32.98517505407394168, 9.000000000000001776 ) ) ;
#52729 = CARTESIAN_POINT ( 'NONE',  ( -108.6886094718227866, -295.1203636427646302, -287.6405681808222425 ) ) ;
#52730 = CARTESIAN_POINT ( 'NONE',  ( -111.5420422543510170, -288.6452337711638165, -273.9453638151793484 ) ) ;
#52731 = CARTESIAN_POINT ( 'NONE',  ( 201.7648208617462728, 289.3015991269851384, -82.29596988341933184 ) ) ;
#52732 = CARTESIAN_POINT ( 'NONE',  ( 208.9495066643430903, 38.23465321184740873, 12.02381566707520477 ) ) ;
#52733 = CARTESIAN_POINT ( 'NONE',  ( -3.386799957615262535, -287.0919661782725143, -338.7113471063460111 ) ) ;
#52734 = CARTESIAN_POINT ( 'NONE',  ( 18.22044941193164647, -283.8377616127854139, -318.9336200276972022 ) ) ;
#52735 = CARTESIAN_POINT ( 'NONE',  ( -104.8937111162223346, -282.3362796204760343, -305.2711007055088430 ) ) ;
#52736 = CARTESIAN_POINT ( 'NONE',  ( -89.81632044842253038, -291.2854897873501159, -219.6125788682560938 ) ) ;
#52737 = CARTESIAN_POINT ( 'NONE',  ( 24.16511653705481777, -282.4206611920876639, -229.8676902555195625 ) ) ;
#52738 = CARTESIAN_POINT ( 'NONE',  ( 30.48805397941071504, -282.7213310520731966, -297.7787434135553326 ) ) ;
#52739 = CARTESIAN_POINT ( 'NONE',  ( -109.2054530565073520, -292.2389411195912317, -293.2031420081622741 ) ) ;
#52740 = B_SPLINE_CURVE_WITH_KNOTS ( 'NONE', 3,
 ( #7105, #43990, #28877, #65353 ),
 .UNSPECIFIED., .F., .F.,
 ( 4, 4 ),
 ( 0.000000000000000000, 9.632970524406137035E-05 ),
 .UNSPECIFIED. ) ;
#52741 = CARTESIAN_POINT ( 'NONE',  ( -37.60979226633180872, -298.2155611169161489, -193.3615846648643810 ) ) ;
#52742 = ORIENTED_EDGE ( 'NONE', *, *, #34428, .T. ) ;
#52743 = CARTESIAN_POINT ( 'NONE',  ( -67.50198497119713181, -287.5245596067173324, -339.6407789118019309 ) ) ;
#52744 = CARTESIAN_POINT ( 'NONE',  ( 37.28522715503766705, -275.3147902972951897, -251.3921505810363044 ) ) ;
#52745 = CARTESIAN_POINT ( 'NONE',  ( -58.13681119472654757, -293.7621706632082805, -198.6173647044027746 ) ) ;
#52746 = DIRECTION ( 'NONE',  ( 0.000000000000000000, 1.000000000000000000, 0.000000000000000000 ) ) ;
#52747 = CARTESIAN_POINT ( 'NONE',  ( -4.829096099716510437, -282.9805209788416391, -202.7746430608542312 ) ) ;
#52748 = CARTESIAN_POINT ( 'NONE',  ( -42.70148299504471368, -275.1194821086073148, -345.3364549598027224 ) ) ;
#52749 = LINE ( 'NONE', #74540, #21631 ) ;
#52750 = CARTESIAN_POINT ( 'NONE',  ( -110.0436413100536441, -295.2438037109412221, -247.3638211004543734 ) ) ;
#52751 = CARTESIAN_POINT ( 'NONE',  ( -82.23163505869359824, -293.0285670518632628, -211.7188467496689839 ) ) ;
#52752 = CARTESIAN_POINT ( 'NONE',  ( 11.62094243344143685, -274.1014709532460643, -216.0107967717650581 ) ) ;
#52753 = CARTESIAN_POINT ( 'NONE',  ( -109.3359468303453639, -291.8659714999176913, -286.1529908743489727 ) ) ;
#52754 = CARTESIAN_POINT ( 'NONE',  ( -30.79784705659721311, -293.0781552111933479, -197.4187679031359721 ) ) ;
#52756 = ADVANCED_FACE ( 'NONE', ( #7586 ), #66512, .T. ) ;
#52755 = CARTESIAN_POINT ( 'NONE',  ( -88.40966833911096501, -287.0845522022424348, -216.7883951211339024 ) ) ;
#52757 = CARTESIAN_POINT ( 'NONE',  ( 21.74201416361712447, -294.3217109682483397, -221.9078311938118588 ) ) ;
#52758 = CARTESIAN_POINT ( 'NONE',  ( -25.11684727967028863, -293.5200938648910665, -194.8372724470382593 ) ) ;
#52759 = CARTESIAN_POINT ( 'NONE',  ( 19.69243349044737101, -294.0293084894926210, -315.9453681172162192 ) ) ;
#52760 = CARTESIAN_POINT ( 'NONE',  ( 35.32004266666400127, -289.3129832617185002, -251.7278616859402405 ) ) ;
#52761 = CARTESIAN_POINT ( 'NONE',  ( 38.14596882137117007, -281.9087520919610483, -285.5470272772021190 ) ) ;
#52762 = CARTESIAN_POINT ( 'NONE',  ( -108.0058485851963610, -271.0452241381656791, -242.8876531527655800 ) ) ;
#52763 = CARTESIAN_POINT ( 'NONE',  ( -91.90149400844251204, -285.1328143694960886, -216.0267007478929600 ) ) ;
#52764 = CARTESIAN_POINT ( 'NONE',  ( 37.28684134950955098, -277.5119494470968675, -268.8030433531653216 ) ) ;
#52765 = EDGE_CURVE ( 'NONE', #14152, #70640, #78614, .T. ) ;
#52766 = CARTESIAN_POINT ( 'NONE',  ( -97.67363213449614534, -283.9265649402213398, -228.5395246498943891 ) ) ;
#52767 = AXIS2_PLACEMENT_3D ( 'NONE', #90557, #62683, #77329 ) ;
#52768 = CARTESIAN_POINT ( 'NONE',  ( 24.71716566015151884, -284.9816810456520670, -228.2228731065362695 ) ) ;
#52769 = CARTESIAN_POINT ( 'NONE',  ( -71.92157598159991494, -277.7395989226884012, -202.9335173445587088 ) ) ;
#52770 = DIRECTION ( 'NONE',  ( 1.000000000000000000, 0.000000000000000000, 0.000000000000000000 ) ) ;
#52771 = CARTESIAN_POINT ( 'NONE',  ( -73.83296191148022558, -283.0580651437806523, -333.7147145270577653 ) ) ;
#52772 = CARTESIAN_POINT ( 'NONE',  ( -112.8477081509243760, -279.9196071709312719, -257.4440180173717749 ) ) ;
#52773 = CARTESIAN_POINT ( 'NONE',  ( 35.72012185478266133, -286.9080193733327064, -293.9151066341677279 ) ) ;
#52774 = CARTESIAN_POINT ( 'NONE',  ( -34.23655326212983852, -296.7727192773767229, -344.3092895495694279 ) ) ;
#52775 = CARTESIAN_POINT ( 'NONE',  ( -4.322871206772958885, -278.2243319901469363, -339.0500441296923668 ) ) ;
#52776 = CARTESIAN_POINT ( 'NONE',  ( -88.86755277788768126, -279.0734126108891928, -326.9153820160118471 ) ) ;
#52777 = CARTESIAN_POINT ( 'NONE',  ( -109.9658807617877017, -278.4894505899445107, -262.4789091549683349 ) ) ;
#52778 = CARTESIAN_POINT ( 'NONE',  ( -97.59114340725315628, -299.1593410089073473, -225.9544209299175463 ) ) ;
#52779 = CARTESIAN_POINT ( 'NONE',  ( 36.77263327021314154, -285.6863584788189883, -280.8028135161503087 ) ) ;
#52780 = CARTESIAN_POINT ( 'NONE',  ( -45.91530714428242987, -290.7591252826912296, -346.1298310116757193 ) ) ;
#52781 = PRODUCT_RELATED_PRODUCT_CATEGORY ( 'part', '', ( #15547 ) ) ;
#52782 = CARTESIAN_POINT ( 'NONE',  ( -41.06862874634942528, -294.0204468436998582, -343.5880544860913233 ) ) ;
#52783 = EDGE_LOOP ( 'NONE', ( #35722, #52288, #80026, #31954 ) ) ;
#52784 = CARTESIAN_POINT ( 'NONE',  ( 33.46552525166386260, -293.4543078974760419, -288.2055658832317135 ) ) ;
#52785 = VERTEX_POINT ( 'NONE', #89426 ) ;
#52786 = CARTESIAN_POINT ( 'NONE',  ( -12.31157078130881288, -289.8138243848017055, -342.9080456449955250 ) ) ;
#52787 = CARTESIAN_POINT ( 'NONE',  ( -64.86217238904167459, -280.3343581237639910, -202.6372944427344578 ) ) ;
#52788 = CARTESIAN_POINT ( 'NONE',  ( -85.01348543588264306, -296.3319389294528605, -210.2870520769135680 ) ) ;
#52789 = CARTESIAN_POINT ( 'NONE',  ( 31.32704074539721617, -287.7575967804397123, -235.7501831046484426 ) ) ;
#52790 = CARTESIAN_POINT ( 'NONE',  ( -78.12160448586301698, -289.9174123739140327, -335.7129868138432585 ) ) ;
#52791 = CARTESIAN_POINT ( 'NONE',  ( -108.4449147762774572, -284.6655195997381611, -287.0416297760234556 ) ) ;
#52792 = DIRECTION ( 'NONE',  ( 1.000000000000000000, 0.000000000000000000, 0.000000000000000000 ) ) ;
#52793 = CARTESIAN_POINT ( 'NONE',  ( 159.4317074227722912, 220.1917126582878268, -204.0458204816173691 ) ) ;
#52794 = CARTESIAN_POINT ( 'NONE',  ( -39.68813811115344947, -139.7239799056983998, -360.9171517653596197 ) ) ;
#52795 = CARTESIAN_POINT ( 'NONE',  ( -85.21861693474863841, -276.9303143095906421, -325.7491400160296280 ) ) ;
#52796 = CARTESIAN_POINT ( 'NONE',  ( -109.9258838242978982, -277.6121890963433998, -259.7252640482822699 ) ) ;
#52797 = CARTESIAN_POINT ( 'NONE',  ( -55.32456115304022148, -273.4936205805251461, -195.5121968093566238 ) ) ;
#52798 = CARTESIAN_POINT ( 'NONE',  ( -104.5539746777214702, -261.5182135941884098, -316.0123334579292873 ) ) ;
#52799 = CARTESIAN_POINT ( 'NONE',  ( -77.56993866038361318, -276.2645236304657601, -335.4994676586070455 ) ) ;
#52800 = VERTEX_POINT ( 'NONE', #31698 ) ;
#52801 = CARTESIAN_POINT ( 'NONE',  ( -109.8498178543374593, -290.9261986689280661, -279.3367129728978853 ) ) ;
#52802 = CARTESIAN_POINT ( 'NONE',  ( -14.87906221710319521, -299.1295042059245475, -193.5196183270483061 ) ) ;
#52803 = CARTESIAN_POINT ( 'NONE',  ( 28.66337167796363516, -286.6718405963765122, -302.6809876054566075 ) ) ;
#52804 = CARTESIAN_POINT ( 'NONE',  ( -113.4446582428203101, -273.3462381016220206, -258.9680425074045047 ) ) ;
#52805 = CARTESIAN_POINT ( 'NONE',  ( -107.9690378533114625, -296.4745153769831063, -288.8707401918701407 ) ) ;
#52806 = ORIENTED_EDGE ( 'NONE', *, *, #37560, .T. ) ;
#52807 = DIRECTION ( 'NONE',  ( -0.000000000000000000, 0.000000000000000000, -1.000000000000000000 ) ) ;
#52808 = CARTESIAN_POINT ( 'NONE',  ( -77.03719570818101658, -279.4993301686889140, -334.7148469967547726 ) ) ;
#52809 = CARTESIAN_POINT ( 'NONE',  ( 32.33399618368085982, -281.4793906983199463, -303.1182592167069174 ) ) ;
#52810 = CARTESIAN_POINT ( 'NONE',  ( -110.5884271342985272, -279.5921097571983296, -273.3848665844764128 ) ) ;
#52811 = CARTESIAN_POINT ( 'NONE',  ( -110.7578647047998857, -280.5615028494339640, -250.7138682111082062 ) ) ;
#52812 = CARTESIAN_POINT ( 'NONE',  ( -99.85852029930474316, -271.5655069418538119, -231.3437507282046681 ) ) ;
#52813 = CARTESIAN_POINT ( 'NONE',  ( 152.4536156746142410, 130.6065089285656313, -11.50000000000000000 ) ) ;
#52814 = CARTESIAN_POINT ( 'NONE',  ( -30.26449800094154696, -280.3107140210297530, -197.6546329628944818 ) ) ;
#52815 = CARTESIAN_POINT ( 'NONE',  ( -2.788545181048796007, -277.4099544044010486, -339.0069418778946897 ) ) ;
#52816 = CARTESIAN_POINT ( 'NONE',  ( 24.48114636701398794, -276.9766916701054242, -227.8773682684846165 ) ) ;
#52817 = CARTESIAN_POINT ( 'NONE',  ( -8.126841969556080514, -275.2516846503793886, -340.9805206333419960 ) ) ;
#52818 = ORIENTED_EDGE ( 'NONE', *, *, #21848, .F. ) ;
#52819 = CARTESIAN_POINT ( 'NONE',  ( 198.3438837837159383, 40.55036610199213953, 11.14960445194775041 ) ) ;
#52820 = CARTESIAN_POINT ( 'NONE',  ( -106.7211857637723114, -290.0570064304056359, -247.1428342424025857 ) ) ;
#52821 = CARTESIAN_POINT ( 'NONE',  ( -35.14282849889130489, -285.4276391690336254, -193.4813689071053773 ) ) ;
#52822 = CARTESIAN_POINT ( 'NONE',  ( -110.8822364370469700, -282.6775636605867135, -279.1568319559953579 ) ) ;
#52823 = EDGE_CURVE ( 'NONE', #13665, #73985, #82759, .T. ) ;
#52825 = CARTESIAN_POINT ( 'NONE',  ( -19.44646104965246991, -284.3639727740243188, -198.1041140780924650 ) ) ;
#52824 = CARTESIAN_POINT ( 'NONE',  ( -7.027200495402667890, -281.2211402287438204, -337.4301864915074702 ) ) ;
#52827 = CARTESIAN_POINT ( 'NONE',  ( 25.22149642160500704, -290.1119102845617022, -311.8161132101660655 ) ) ;
#52826 = AXIS2_PLACEMENT_3D ( 'NONE', #1069, #87678, #22829 ) ;
#52828 = CARTESIAN_POINT ( 'NONE',  ( -22.12699886173711050, -281.4563536819765659, -198.5061716987787008 ) ) ;
#52829 = CARTESIAN_POINT ( 'NONE',  ( -111.8722755992515800, -270.6595642643046631, -261.9829339559319692 ) ) ;
#52830 = CARTESIAN_POINT ( 'NONE',  ( 30.35697287138012967, -280.4076286439792511, -305.3372539550782108 ) ) ;
#52831 = CARTESIAN_POINT ( 'NONE',  ( 16.15335719093937072, -296.2938587509344188, -323.0019167985424247 ) ) ;
#52832 = CARTESIAN_POINT ( 'NONE',  ( -94.18861208088614489, -277.4843187276652543, -219.9388747130817023 ) ) ;
#52833 = VECTOR ( 'NONE', #73598, 1000.000000000000000 ) ;
#52834 = CARTESIAN_POINT ( 'NONE',  ( -72.88431817205568564, -278.1877008478857647, -334.2552104160218391 ) ) ;
#52835 = CARTESIAN_POINT ( 'NONE',  ( -37.99274674150289854, -288.0441689586845087, -195.1972665018789996 ) ) ;
#52836 = CARTESIAN_POINT ( 'NONE',  ( 161.2494399300530290, -11.64849832608277325, -3.999999999999998224 ) ) ;
#52837 = CARTESIAN_POINT ( 'NONE',  ( -70.29226251824722738, -293.5414334964053751, -202.3642456944826620 ) ) ;
#52838 = CARTESIAN_POINT ( 'NONE',  ( 35.16948615312456639, -273.7982598852104843, -289.5217159807754683 ) ) ;
#52839 = CARTESIAN_POINT ( 'NONE',  ( -73.10779325498795345, -288.7111114407824743, -338.3827954629169881 ) ) ;
#52840 = CARTESIAN_POINT ( 'NONE',  ( -14.58052054456640079, -290.7520197055860081, -200.1587738769403018 ) ) ;
#52841 = CARTESIAN_POINT ( 'NONE',  ( -48.18343439341505530, -270.7767787986900316, -433.0017230881019827 ) ) ;
#52842 = CARTESIAN_POINT ( 'NONE',  ( -74.27549655622148350, -276.2391080209486631, -333.8995957708779088 ) ) ;
#52843 = CARTESIAN_POINT ( 'NONE',  ( -99.78492158301806114, -294.1443065307786355, -310.6014342814366387 ) ) ;
#52844 = CARTESIAN_POINT ( 'NONE',  ( -109.4191141173435824, -291.6783802566276904, -284.7812456618848955 ) ) ;
#52845 =( NAMED_UNIT ( * ) SI_UNIT ( $, .STERADIAN. ) SOLID_ANGLE_UNIT ( ) );
#52846 = DIRECTION ( 'NONE',  ( 0.000000000000000000, 1.000000000000000000, 0.000000000000000000 ) ) ;
#52847 = CARTESIAN_POINT ( 'NONE',  ( 36.04275873721073964, -291.7669403933651893, -249.3986615262905104 ) ) ;
#52848 = CARTESIAN_POINT ( 'NONE',  ( 27.05560708662114777, -288.6632888032719393, -234.2090409928904648 ) ) ;
#52849 = CARTESIAN_POINT ( 'NONE',  ( -101.4584337724489416, -288.2492599616738289, -311.2381121573827158 ) ) ;
#52850 = CARTESIAN_POINT ( 'NONE',  ( 26.87274919344519475, -288.4884608640265355, -234.3141791509244740 ) ) ;
#52851 = CARTESIAN_POINT ( 'NONE',  ( 125.9462722777150958, 8.500086813760361792, 21.50000000000000000 ) ) ;
#52852 = CARTESIAN_POINT ( 'NONE',  ( 31.12209605237864096, -288.0098328072009508, -244.4245517556633160 ) ) ;
#52853 = CARTESIAN_POINT ( 'NONE',  ( -58.36767796827526666, -297.3023644872446312, -342.7778845247910340 ) ) ;
#52854 = DIRECTION ( 'NONE',  ( -0.8660254037844368202, -0.5000000000000032196, 0.000000000000000000 ) ) ;
#52855 = CARTESIAN_POINT ( 'NONE',  ( 37.44067781889307156, -288.9666742209906261, -287.0224002332747091 ) ) ;
#52856 = CARTESIAN_POINT ( 'NONE',  ( -34.37262320475240074, -275.0949447357804729, -345.8627655304486552 ) ) ;
#52857 = CARTESIAN_POINT ( 'NONE',  ( -111.4190136797459445, -278.6229744271665822, -291.2966358536714324 ) ) ;
#52858 = CARTESIAN_POINT ( 'NONE',  ( -93.05551746675897107, -278.9460170913204138, -217.1651463320342543 ) ) ;
#52859 = CARTESIAN_POINT ( 'NONE',  ( -97.43923713673152065, -299.1390759897273597, -226.0661418624069938 ) ) ;
#52860 = CARTESIAN_POINT ( 'NONE',  ( -96.51986230846380010, -283.1841407724330679, -224.2648371492523438 ) ) ;
#52861 = CARTESIAN_POINT ( 'NONE',  ( -48.18343439339133027, -253.2160367275913018, -476.5905725147042062 ) ) ;
#52862 = CARTESIAN_POINT ( 'NONE',  ( -27.36937928137762555, -278.3196412620700926, -196.7467161590899991 ) ) ;
#52863 = CARTESIAN_POINT ( 'NONE',  ( -70.86816973665412434, -281.4943253534577821, -337.4504352275245083 ) ) ;
#52864 = FACE_OUTER_BOUND ( 'NONE', #42187, .T. ) ;
#52865 = CARTESIAN_POINT ( 'NONE',  ( -3.054153816885291750, -275.0873756752500299, -338.5450976772041827 ) ) ;
#52866 = CARTESIAN_POINT ( 'NONE',  ( -97.74064010755812149, -297.4890610725284432, -312.5828635937504600 ) ) ;
#52867 = CARTESIAN_POINT ( 'NONE',  ( -71.61299339516558859, -282.4146654591520473, -338.9684861646819058 ) ) ;
#52868 = CARTESIAN_POINT ( 'NONE',  ( -107.6887101570641079, -297.7618895802689281, -249.9967709899610497 ) ) ;
#52869 = CARTESIAN_POINT ( 'NONE',  ( -26.31508129919702554, -299.5026522738583026, -193.8518589591636783 ) ) ;
#52870 = CARTESIAN_POINT ( 'NONE',  ( -14.05468214643588887, -274.0294635639677949, -201.1527205133580480 ) ) ;
#52871 = CARTESIAN_POINT ( 'NONE',  ( 30.53809882329510472, -295.1315086098708207, -238.3429694970579931 ) ) ;
#52872 = CARTESIAN_POINT ( 'NONE',  ( 28.90482438819904232, -288.2301685438775394, -309.6090223088555717 ) ) ;
#52873 = CARTESIAN_POINT ( 'NONE',  ( -103.5203790401297823, -277.1133310609986324, -233.8961121139607826 ) ) ;
#52874 = CARTESIAN_POINT ( 'NONE',  ( -97.29141447937213627, -289.7374861096076302, -318.7040782949550248 ) ) ;
#52875 = CARTESIAN_POINT ( 'NONE',  ( -100.5129623374312757, -289.1025978490149555, -307.5123437947870002 ) ) ;
#52876 = CARTESIAN_POINT ( 'NONE',  ( 34.38200405421400774, -291.2693564601977414, -248.4359975098352891 ) ) ;
#52877 = ORIENTED_EDGE ( 'NONE', *, *, #68122, .T. ) ;
#52878 = CARTESIAN_POINT ( 'NONE',  ( 197.8058612754009289, 70.97294607549092404, 10.93316417084198910 ) ) ;
#52879 = CARTESIAN_POINT ( 'NONE',  ( -104.1065005738800266, -289.6591952903842753, -300.1584588779952014 ) ) ;
#52880 = CARTESIAN_POINT ( 'NONE',  ( 209.4907211740960804, 29.55254324029474233, 13.48241519114203690 ) ) ;
#52881 = CARTESIAN_POINT ( 'NONE',  ( -65.15572444676007535, -284.3480930052128883, -341.9238641087768542 ) ) ;
#52882 = CARTESIAN_POINT ( 'NONE',  ( 39.26644811233330756, -292.6820633193152617, -276.0337351328423097 ) ) ;
#52883 = CARTESIAN_POINT ( 'NONE',  ( 37.66539852573927050, -283.0570603285356128, -285.4353816718631833 ) ) ;
#52884 = CARTESIAN_POINT ( 'NONE',  ( -1.253852617203371267, -282.3923338942843770, -333.8171442254862313 ) ) ;
#52885 = CARTESIAN_POINT ( 'NONE',  ( -80.62502170165275572, -297.4831521112486143, -206.6137783220986250 ) ) ;
#52886 = CARTESIAN_POINT ( 'NONE',  ( 21.24008799144644399, -277.4867559308806335, -314.7392384929083846 ) ) ;
#52887 = CARTESIAN_POINT ( 'NONE',  ( 30.23813378314736866, -291.1520963426760886, -238.5402586313514917 ) ) ;
#52888 = CARTESIAN_POINT ( 'NONE',  ( -16.51336718030072959, -273.1221465266997370, -199.9283559951378493 ) ) ;
#52889 = ORIENTED_EDGE ( 'NONE', *, *, #50363, .F. ) ;
#52890 = ORIENTED_EDGE ( 'NONE', *, *, #38393, .F. ) ;
#52891 = CARTESIAN_POINT ( 'NONE',  ( 175.2296996224750103, 275.5000000000000568, 0.000000000000000000 ) ) ;
#52892 = CARTESIAN_POINT ( 'NONE',  ( -24.92523695310635645, -288.1317618822296254, -196.9116328052222400 ) ) ;
#52893 = CARTESIAN_POINT ( 'NONE',  ( -96.26505957714701367, -296.9686803682694176, -319.4684986374722371 ) ) ;
#52894 = CARTESIAN_POINT ( 'NONE',  ( -107.8572869369304783, -284.9487349115707957, -289.6812583194907802 ) ) ;
#52895 = CARTESIAN_POINT ( 'NONE',  ( -68.92954192339310282, -276.5161724624428530, -340.3399598094454745 ) ) ;
#52896 = CARTESIAN_POINT ( 'NONE',  ( 37.00015142589705164, -294.4500412056358982, -290.0233125297866081 ) ) ;
#52897 = CARTESIAN_POINT ( 'NONE',  ( 31.72894637059891920, -286.0959716072634933, -301.4987362296672586 ) ) ;
#52898 = AXIS2_PLACEMENT_3D ( 'NONE', #23663, #8051, #74307 ) ;
#52899 = CARTESIAN_POINT ( 'NONE',  ( 33.39881656458503301, -294.2737037300373686, -300.8523605945501345 ) ) ;
#52900 = CARTESIAN_POINT ( 'NONE',  ( -83.84576561169004094, -291.7259993838657124, -214.0631661532510179 ) ) ;
#52901 = CARTESIAN_POINT ( 'NONE',  ( 140.6539576904058606, 275.5000000000000568, 12.00000000000000178 ) ) ;
#52902 = CARTESIAN_POINT ( 'NONE',  ( 223.4306832106271372, -147.4436952405746695, -21.50000000000000000 ) ) ;
#52903 = CARTESIAN_POINT ( 'NONE',  ( -109.4300717440927997, -269.0112169713434582, -295.3470023912169609 ) ) ;
#52904 = TOROIDAL_SURFACE ( 'NONE', #28735, 24.16304133878946558, 4.003189038634632269 ) ;
#52905 = CARTESIAN_POINT ( 'NONE',  ( -110.8185765141799664, -285.8119414575437531, -290.9488908156019420 ) ) ;
#52906 = CARTESIAN_POINT ( 'NONE',  ( -69.91165696735023971, -292.9809262143061801, -337.9199732462171255 ) ) ;
#52907 = ORIENTED_EDGE ( 'NONE', *, *, #72224, .T. ) ;
#52908 = CARTESIAN_POINT ( 'NONE',  ( -51.08928946488654788, -282.1521856814465536, -342.4214544691175206 ) ) ;
#52909 = CARTESIAN_POINT ( 'NONE',  ( -114.1894973160493834, -278.2750411820364889, -265.8710891626689090 ) ) ;
#52910 = CARTESIAN_POINT ( 'NONE',  ( 26.69217992362646186, -283.0311184695250404, -231.5349147641474872 ) ) ;
#52911 = CARTESIAN_POINT ( 'NONE',  ( 186.9921997741134874, 261.2987433936410753, -152.4087338747540343 ) ) ;
#52912 = CARTESIAN_POINT ( 'NONE',  ( -41.55494075974604584, -281.6788319875972775, -346.7075708460292276 ) ) ;
#52913 = CARTESIAN_POINT ( 'NONE',  ( 37.27298318533834021, -285.6174132796443246, -273.8615511421464248 ) ) ;
#52914 = CARTESIAN_POINT ( 'NONE',  ( 15.15386417747978065, -276.6441548003469961, -215.7303463689980276 ) ) ;
#52915 = CARTESIAN_POINT ( 'NONE',  ( -41.03606502414044144, -295.5922114829648990, -343.3417718623419432 ) ) ;
#52916 = CARTESIAN_POINT ( 'NONE',  ( -7.051796838840049375, -291.1429634180491917, -203.4001947657375524 ) ) ;
#52917 = CARTESIAN_POINT ( 'NONE',  ( -113.1374199070956337, -279.3660340736049079, -257.3872346043302741 ) ) ;
#52918 = CARTESIAN_POINT ( 'NONE',  ( -45.90809833673234408, -277.1636558391409721, -342.9073768484916513 ) ) ;
#52919 = CARTESIAN_POINT ( 'NONE',  ( -91.95860984523744719, -274.3742695399199647, -216.5235318333530188 ) ) ;
#52920 = CARTESIAN_POINT ( 'NONE',  ( -62.31836764008141927, -276.2897727279634523, -342.9269177751296525 ) ) ;
#52921 = CARTESIAN_POINT ( 'NONE',  ( -114.1313572138536756, -273.4603215278654034, -270.3726811538930406 ) ) ;
#52922 = CARTESIAN_POINT ( 'NONE',  ( -71.10962066431646633, -275.4976060606911688, -337.3433636945234184 ) ) ;
#52923 = CARTESIAN_POINT ( 'NONE',  ( 13.02120570071824801, -295.7904190895197303, -327.8959196409172705 ) ) ;
#52924 = CARTESIAN_POINT ( 'NONE',  ( 197.2116943569230330, 250.5000000000000568, -12.92446933126074882 ) ) ;
#52925 = CARTESIAN_POINT ( 'NONE',  ( 222.8344101925596306, 0.000000000000000000, 7.000000000000000000 ) ) ;
#52926 = CARTESIAN_POINT ( 'NONE',  ( -110.5377808231913264, -285.6962349906131635, -265.4581718816438070 ) ) ;
#52927 = CARTESIAN_POINT ( 'NONE',  ( -107.2855023687954343, -285.9277146292558314, -300.1913977338916766 ) ) ;
#52928 = CARTESIAN_POINT ( 'NONE',  ( 25.04202366807640701, -286.3764446069573637, -232.2538526206583356 ) ) ;
#52929 = CARTESIAN_POINT ( 'NONE',  ( -67.14420636782639917, -275.8494032447125051, -337.8759388639248300 ) ) ;
#52930 = CARTESIAN_POINT ( 'NONE',  ( 27.95254771904341240, -283.8864505880648039, -305.6814616368637871 ) ) ;
#52931 = CARTESIAN_POINT ( 'NONE',  ( -26.94262829620306121, -275.3973957843101630, -343.3170434189988214 ) ) ;
#52932 = ADVANCED_FACE ( 'NONE', ( #38784 ), #48364, .T. ) ;
#52933 = CARTESIAN_POINT ( 'NONE',  ( -59.27443785015729816, -278.4225302841888947, -340.3123945185845400 ) ) ;
#52934 = EDGE_CURVE ( 'NONE', #24951, #135, #39693, .T. ) ;
#52935 = CARTESIAN_POINT ( 'NONE',  ( 184.5358909326088792, 2.965303559109565779, -9.000000000000001776 ) ) ;
#52936 = CARTESIAN_POINT ( 'NONE',  ( -65.84292934857880653, -274.1612808213567405, -203.0880299406145753 ) ) ;
#52937 = CARTESIAN_POINT ( 'NONE',  ( -1.220403248673440633, -281.3218338926274100, -202.5421624273162706 ) ) ;
#52938 = CARTESIAN_POINT ( 'NONE',  ( -19.77637039212308778, -280.7643475223692349, -195.3998767140380721 ) ) ;
#52939 = ORIENTED_EDGE ( 'NONE', *, *, #24999, .F. ) ;
#52940 = ORIENTED_EDGE ( 'NONE', *, *, #37043, .F. ) ;
#52941 = CARTESIAN_POINT ( 'NONE',  ( 113.5000000000000568, -218.8335761803644743, -490.8867980474134356 ) ) ;
#52942 = CARTESIAN_POINT ( 'NONE',  ( 37.56078752127080378, -289.2665936233599382, -258.8765448690845687 ) ) ;
#52943 = CARTESIAN_POINT ( 'NONE',  ( -110.5458421655025631, -295.7349115658649339, -271.4553519522693819 ) ) ;
#52944 = CARTESIAN_POINT ( 'NONE',  ( -92.73289361938923037, -290.6326221338760547, -216.9456264775200225 ) ) ;
#52945 = CARTESIAN_POINT ( 'NONE',  ( 35.20081947324865723, -286.2015476355265378, -283.3338048062519192 ) ) ;
#52946 = CARTESIAN_POINT ( 'NONE',  ( -15.69551543743928690, -287.3413870195105915, -340.7479812429321555 ) ) ;
#52947 = CARTESIAN_POINT ( 'NONE',  ( -27.80004502404392142, -287.3811029544205553, -197.5868964331813231 ) ) ;
#52948 = CARTESIAN_POINT ( 'NONE',  ( -68.21596190209044153, -275.4574352439856852, -338.7255761431582641 ) ) ;
#52949 = CARTESIAN_POINT ( 'NONE',  ( 30.96119841013293694, -286.3920612148663167, -304.2610323384864728 ) ) ;
#52950 = CARTESIAN_POINT ( 'NONE',  ( -67.71477923858087422, -287.6537837843613374, -201.7725056304563509 ) ) ;
#52951 = CARTESIAN_POINT ( 'NONE',  ( -10.24848132093128683, -286.6991876887565809, -340.4752101572107108 ) ) ;
#52952 = CARTESIAN_POINT ( 'NONE',  ( -59.00633739944922240, -284.2805763211763974, -340.3719291050030051 ) ) ;
#52953 = CARTESIAN_POINT ( 'NONE',  ( -85.36186015661988336, -293.3909304980733737, -212.4653850451964843 ) ) ;
#52954 = CARTESIAN_POINT ( 'NONE',  ( 82.15278769198762632, -299.2458075654235472, -193.3794153738201942 ) ) ;
#52955 = CARTESIAN_POINT ( 'NONE',  ( 155.3770881450957688, 21.00000000067973005, -15.20409621215713969 ) ) ;
#52956 = CARTESIAN_POINT ( 'NONE',  ( -105.2304370271346556, -298.9063830277762008, -237.1883339964281276 ) ) ;
#52957 =( BOUNDED_CURVE ( )  B_SPLINE_CURVE ( 3, ( #61492, #91260, #90779, #25938 ),
 .UNSPECIFIED., .F., .F. ) 
 B_SPLINE_CURVE_WITH_KNOTS ( ( 4, 4 ),
 ( 2.029441677703989644, 3.141592653589793116 ),
 .UNSPECIFIED. ) 
 CURVE ( )  GEOMETRIC_REPRESENTATION_ITEM ( )  RATIONAL_B_SPLINE_CURVE ( ( 1.000000000000000000, 0.8995554851227762772, 0.8995554851227762772, 1.000000000000000000 ) ) 
 REPRESENTATION_ITEM ( '' )  );
#52958 = CARTESIAN_POINT ( 'NONE',  ( -24.83876581564859265, -279.4129113542517189, -198.2759020219323247 ) ) ;
#52959 = CARTESIAN_POINT ( 'NONE',  ( 23.41763057008242654, -280.1509791256234507, -314.3524546316896817 ) ) ;
#52960 = CARTESIAN_POINT ( 'NONE',  ( -32.03389183627948000, -294.1839943711370893, -347.0293249437656300 ) ) ;
#52961 = CARTESIAN_POINT ( 'NONE',  ( -111.1983153317845705, -270.8641581079432967, -264.8155075547770139 ) ) ;
#52962 = CARTESIAN_POINT ( 'NONE',  ( 36.81500955481342174, -273.5407523786277011, -263.3081620640912206 ) ) ;
#52963 = CARTESIAN_POINT ( 'NONE',  ( -50.54346519758605893, -296.5394663848581445, -342.6588141822074931 ) ) ;
#52964 = DIRECTION ( 'NONE',  ( -0.000000000000000000, -1.000000000000000000, -0.000000000000000000 ) ) ;
#52965 = CARTESIAN_POINT ( 'NONE',  ( -113.7524713807139847, -271.1271092548682873, -270.3430111821825790 ) ) ;
#52966 = CARTESIAN_POINT ( 'NONE',  ( -69.12476854696672035, -293.7043150738253985, -339.3957269854918195 ) ) ;
#52967 = CARTESIAN_POINT ( 'NONE',  ( 30.39103089515177558, -294.5927094717742989, -241.4618840749325841 ) ) ;
#52968 = CARTESIAN_POINT ( 'NONE',  ( 160.5350683151633291, 250.5000000000000568, 20.22542485937379908 ) ) ;
#52969 = CARTESIAN_POINT ( 'NONE',  ( 13.00689367574113398, -293.5803556918614277, -217.2798517143304764 ) ) ;
#52970 = TOROIDAL_SURFACE ( 'NONE', #51475, 2.500000000000000000, 0.5000000000000000000 ) ;
#52971 = DIRECTION ( 'NONE',  ( -0.000000000000000000, -1.000000000000000000, -0.000000000000000000 ) ) ;
#52972 = EDGE_CURVE ( 'NONE', #39851, #73473, #56020, .T. ) ;
#52974 = CARTESIAN_POINT ( 'NONE',  ( -42.38972445051935978, -295.1175873543253942, -343.1863708172744509 ) ) ;
#52973 = CARTESIAN_POINT ( 'NONE',  ( -32.38879771034004307, -284.1343958998429571, -195.1559757263966617 ) ) ;
#52975 = CARTESIAN_POINT ( 'NONE',  ( -31.63628840493104022, -282.9820349885084170, -347.1627201842926524 ) ) ;
#52976 = CARTESIAN_POINT ( 'NONE',  ( 38.26933019700478411, -283.4666088895169196, -269.9139198983525603 ) ) ;
#52977 = AXIS2_PLACEMENT_3D ( 'NONE', #25732, #49401, #48442 ) ;
#52978 = CARTESIAN_POINT ( 'NONE',  ( -32.30356362843286888, -285.7807410796282852, -193.5341449109557175 ) ) ;
#52979 = CARTESIAN_POINT ( 'NONE',  ( -84.97693536769345712, -289.3929332568648078, -212.6470574160508136 ) ) ;
#52980 = CARTESIAN_POINT ( 'NONE',  ( 13.20688177674606045, -280.8407585787695666, -327.5939101614723086 ) ) ;
#52981 = B_SPLINE_CURVE_WITH_KNOTS ( 'NONE', 3,
 ( #1168, #73142, #44705, #73606 ),
 .UNSPECIFIED., .F., .F.,
 ( 4, 4 ),
 ( 0.000000000000000000, 9.632970524405802288E-05 ),
 .UNSPECIFIED. ) ;
#52982 = CARTESIAN_POINT ( 'NONE',  ( 5.023221169071004688, -285.3227047679677071, -210.2450494071990192 ) ) ;
#52983 = CARTESIAN_POINT ( 'NONE',  ( -23.38175571388271123, -287.7981557650520017, -345.8246450283934905 ) ) ;
#52984 = CARTESIAN_POINT ( 'NONE',  ( 184.7149167944524493, 8.542400036368780647, 13.00000000000000178 ) ) ;
#52985 = CARTESIAN_POINT ( 'NONE',  ( 17.69057799172644607, -295.8482004993076657, -319.5522096877774061 ) ) ;
#52986 = CARTESIAN_POINT ( 'NONE',  ( -113.7950496592970779, -279.9615961741182559, -271.6169663873831155 ) ) ;
#52988 = CARTESIAN_POINT ( 'NONE',  ( -67.31108647503970133, -279.3147082179402219, -203.7597963752540124 ) ) ;
#52987 = CARTESIAN_POINT ( 'NONE',  ( 35.50002531251338667, -291.8191611890306945, -289.6611138460939401 ) ) ;
#52989 = CARTESIAN_POINT ( 'NONE',  ( 34.46205805791058197, -293.3649064608505341, -242.4069416680160032 ) ) ;
#52990 = CARTESIAN_POINT ( 'NONE',  ( -99.79227414052319034, -283.2047112595854514, -227.7335719275758663 ) ) ;
#52991 = CARTESIAN_POINT ( 'NONE',  ( -98.01637611950918938, -279.9515046978928012, -314.4690477051376547 ) ) ;
#52992 = CARTESIAN_POINT ( 'NONE',  ( -93.26982013910412661, -294.9409382661231689, -317.6611356547886089 ) ) ;
#52993 = CARTESIAN_POINT ( 'NONE',  ( -30.68020254121020329, -296.1353836042920307, -195.3633804044103215 ) ) ;
#52994 = VERTEX_POINT ( 'NONE', #32161 ) ;
#52995 = DIRECTION ( 'NONE',  ( 0.000000000000000000, 0.000000000000000000, 1.000000000000000000 ) ) ;
#52996 = CARTESIAN_POINT ( 'NONE',  ( 27.88413399525486369, -283.0466931843626526, -234.0645979971862118 ) ) ;
#52997 = CARTESIAN_POINT ( 'NONE',  ( -109.3354294181779238, -296.2238419858752536, -257.9155812456735362 ) ) ;
#52998 = CARTESIAN_POINT ( 'NONE',  ( 195.0023263777187879, -0.4142135623730946459, 22.50000000000000000 ) ) ;
#52999 = CARTESIAN_POINT ( 'NONE',  ( -20.19161114001082069, -271.7666405000205714, -195.3683826091709363 ) ) ;
#53000 = CARTESIAN_POINT ( 'NONE',  ( 1.123461091271782619, -273.7491908978996094, -203.8282707832596827 ) ) ;
#53001 = CARTESIAN_POINT ( 'NONE',  ( 23.75853831036545927, -289.4843685441786647, -316.4052178972695515 ) ) ;
#53002 = CARTESIAN_POINT ( 'NONE',  ( -107.3946968973942688, -290.6576443695460625, -249.7843809094832750 ) ) ;
#53003 = CARTESIAN_POINT ( 'NONE',  ( -70.06543656954286803, -281.1331322640704684, -204.3178663081950504 ) ) ;
#53004 = CARTESIAN_POINT ( 'NONE',  ( 96.68924888517000227, -301.5126242020289169, -196.3069997221729182 ) ) ;
#53005 = CARTESIAN_POINT ( 'NONE',  ( -87.79248114618259535, -278.1233576937960379, -216.9818968792185956 ) ) ;
#53006 = CARTESIAN_POINT ( 'NONE',  ( -102.7179183965434106, -272.9176807552647688, -229.6800402017144620 ) ) ;
#53007 = CARTESIAN_POINT ( 'NONE',  ( -95.42965408058364574, -293.1176511800382514, -223.7886927239548527 ) ) ;
#53008 = CARTESIAN_POINT ( 'NONE',  ( 196.7806748523260012, 275.5000000000000568, -12.67104836398113399 ) ) ;
#53009 = CARTESIAN_POINT ( 'NONE',  ( -108.2093379558849051, -291.4405548779228639, -252.3750077615254384 ) ) ;
#53010 = CARTESIAN_POINT ( 'NONE',  ( -43.18343439339132317, -283.1093320178187582, -507.6442049081570076 ) ) ;
#53011 = CARTESIAN_POINT ( 'NONE',  ( -61.27555736024090294, -289.8843411434714312, -198.4207100790942491 ) ) ;
#53012 = CARTESIAN_POINT ( 'NONE',  ( -90.05819054004119550, -296.9485288423666134, -219.7609553567533851 ) ) ;
#53013 = CARTESIAN_POINT ( 'NONE',  ( 164.2231345125756263, 264.6571197653884155, 7.500000000000000000 ) ) ;
#53014 = CARTESIAN_POINT ( 'NONE',  ( -86.08515411122583316, -292.9109692148467161, -211.5831819810707941 ) ) ;
#53015 = CARTESIAN_POINT ( 'NONE',  ( 40.65961533371913106, -290.2662352645559167, -288.1317622949166548 ) ) ;
#53016 = CARTESIAN_POINT ( 'NONE',  ( 16.32701712819017459, -288.8167080040751102, -218.2104016491132938 ) ) ;
#53017 = CARTESIAN_POINT ( 'NONE',  ( -0.5915648041198875440, -274.5628873244131114, -335.6075981082368003 ) ) ;
#53018 = CARTESIAN_POINT ( 'NONE',  ( 34.29008848677463561, -277.7354209081919407, -290.6612418364263135 ) ) ;
#53019 = CARTESIAN_POINT ( 'NONE',  ( -38.90375606591197055, -290.1122500275077414, -195.9375049135655615 ) ) ;
#53020 = CARTESIAN_POINT ( 'NONE',  ( -79.24763684613134274, -281.3539909854462735, -207.1776680982772803 ) ) ;
#53021 = ORIENTED_EDGE ( 'NONE', *, *, #45025, .T. ) ;
#53022 = CARTESIAN_POINT ( 'NONE',  ( -73.85489126903598844, -282.8990247954959614, -333.7487314242565617 ) ) ;
#53023 = CARTESIAN_POINT ( 'NONE',  ( -114.0688391286936110, -279.6519961044837146, -268.7544982487737002 ) ) ;
#53024 = CARTESIAN_POINT ( 'NONE',  ( -0.5795466856604392092, -281.3697773409666638, -337.5812819858398939 ) ) ;
#53025 = CARTESIAN_POINT ( 'NONE',  ( -17.40741497080009026, -277.7422512970396156, -344.4923832326744559 ) ) ;
#53026 = EDGE_CURVE ( 'NONE', #76418, #25970, #89182, .T. ) ;
#53027 =( LENGTH_UNIT ( ) NAMED_UNIT ( * ) SI_UNIT ( .MILLI., .METRE. ) );
#53028 = CARTESIAN_POINT ( 'NONE',  ( 11.32844739937061185, -276.2323756685872809, -211.5223723098345658 ) ) ;
#53029 = CARTESIAN_POINT ( 'NONE',  ( 30.89617123739170168, -277.8376638359844719, -254.7536222014695397 ) ) ;
#53030 = ORIENTED_EDGE ( 'NONE', *, *, #49884, .F. ) ;
#53031 = EDGE_CURVE ( 'NONE', #3893, #81225, #71106, .T. ) ;
#53032 = CARTESIAN_POINT ( 'NONE',  ( -109.5208497428386494, -298.2901384315509858, -290.7368636486585842 ) ) ;
#53033 = VECTOR ( 'NONE', #67809, 1000.000000000000000 ) ;
#53034 = CARTESIAN_POINT ( 'NONE',  ( -8.082532586125303453, -289.7394651209468748, -337.6324074843216181 ) ) ;
#53035 = CARTESIAN_POINT ( 'NONE',  ( -34.67957604879136824, -290.7792651970697761, -346.3011411006759772 ) ) ;
#53036 = CARTESIAN_POINT ( 'NONE',  ( -36.19622276349792145, -291.4154381539049723, -197.2556659408412827 ) ) ;
#53037 = CARTESIAN_POINT ( 'NONE',  ( 34.79870787013732070, -286.7214059749196622, -243.6162411466187621 ) ) ;
#53038 = CARTESIAN_POINT ( 'NONE',  ( 200.4946632162240405, 214.9970011440365454, -2.952039013598904749 ) ) ;
#53039 = CARTESIAN_POINT ( 'NONE',  ( -96.57590147151967130, -282.3412929085624796, -314.3809976734893326 ) ) ;
#53040 = CARTESIAN_POINT ( 'NONE',  ( -99.86962490730880404, -291.8682696704935893, -310.3751667958574672 ) ) ;
#53041 = CARTESIAN_POINT ( 'NONE',  ( -108.6951794500373296, -283.2729355634384660, -251.9386115642138293 ) ) ;
#53042 = EDGE_CURVE ( 'NONE', #55081, #54755, #60567, .T. ) ;
#53043 = CARTESIAN_POINT ( 'NONE',  ( -4.139662744114851023, -281.8145574705715717, -204.7813796066878922 ) ) ;
#53044 = CARTESIAN_POINT ( 'NONE',  ( 7.805841084176246447, -289.3938539990620029, -332.5114538443609149 ) ) ;
#53045 = CARTESIAN_POINT ( 'NONE',  ( -110.2204724192045973, -279.1125744993161106, -265.1965278867569964 ) ) ;
#53046 = CARTESIAN_POINT ( 'NONE',  ( -74.47292207905763917, -290.3644405673160236, -203.3590204376128838 ) ) ;
#53047 = CARTESIAN_POINT ( 'NONE',  ( -46.49642105660959857, -286.7415999113241583, -194.0699002380351885 ) ) ;
#53048 = CARTESIAN_POINT ( 'NONE',  ( 2.703626289413516570, -287.0665495901047848, -204.6656178680383391 ) ) ;
#53049 = CARTESIAN_POINT ( 'NONE',  ( -109.9946368399960903, -284.8192079691270351, -262.7521607666493537 ) ) ;
#53050 = EDGE_LOOP ( 'NONE', ( #11233, #53864, #62871, #70407 ) ) ;
#53051 = CARTESIAN_POINT ( 'NONE',  ( -48.18343439339133027, -253.0206516614774728, -430.6442049081568939 ) ) ;
#53052 = CARTESIAN_POINT ( 'NONE',  ( -22.45997228950932723, -294.1010007409788045, -196.0187729305145012 ) ) ;
#53053 = CARTESIAN_POINT ( 'NONE',  ( 0.2832901835247852995, -293.2467705303265575, -336.9919503981581101 ) ) ;
#53054 = CARTESIAN_POINT ( 'NONE',  ( -69.36509140515003935, -276.5428862207825773, -336.2378189899075664 ) ) ;
#53055 = CARTESIAN_POINT ( 'NONE',  ( -112.4991034928404332, -296.1051980012548484, -254.0307771500460774 ) ) ;
#53056 = CARTESIAN_POINT ( 'NONE',  ( 29.37436662899752804, -291.6117925792218557, -238.9408694813325553 ) ) ;
#53057 = CARTESIAN_POINT ( 'NONE',  ( -109.7661201162576106, -294.9912530385681748, -255.0465033180652199 ) ) ;
#53058 = CARTESIAN_POINT ( 'NONE',  ( -107.7806711441714782, -292.0291786409208612, -249.6892464931493407 ) ) ;
#53059 = CARTESIAN_POINT ( 'NONE',  ( 8.431853164986209848, -295.4883968045187430, -327.6889906226460880 ) ) ;
#53060 = CARTESIAN_POINT ( 'NONE',  ( 175.2296996224750103, 250.0000000000000568, 0.000000000000000000 ) ) ;
#53061 = CARTESIAN_POINT ( 'NONE',  ( -5.307539361340629647, -292.6314885058652067, -338.3740712721836417 ) ) ;
#53062 = CARTESIAN_POINT ( 'NONE',  ( -11.08832550499942116, -300.3809508611794854, -195.3521588642121571 ) ) ;
#53063 = CARTESIAN_POINT ( 'NONE',  ( 35.22763264693584517, -288.3589713167405648, -260.1371975069002929 ) ) ;
#53064 = CARTESIAN_POINT ( 'NONE',  ( 34.50225496963312111, -277.8240175483897474, -293.0955174419003697 ) ) ;
#53065 = CARTESIAN_POINT ( 'NONE',  ( 7.993650690917188051, -275.2431296414775943, -332.1739661845221008 ) ) ;
#53066 = CARTESIAN_POINT ( 'NONE',  ( -2.596169063361186247, -273.8480426571001658, -201.7456988806351887 ) ) ;
#53067 = CARTESIAN_POINT ( 'NONE',  ( 37.00287235400327290, -279.6807381723089634, -274.1292392309097181 ) ) ;
#53068 = CARTESIAN_POINT ( 'NONE',  ( -35.74887623184653052, -275.4323944858504092, -346.5574588081581169 ) ) ;
#53069 = CARTESIAN_POINT ( 'NONE',  ( -110.5398752692821063, -295.3303424341170285, -263.2352950540829966 ) ) ;
#53070 = CARTESIAN_POINT ( 'NONE',  ( -106.3221749556402642, -274.9386761118286699, -240.7908190081843713 ) ) ;
#53071 = CARTESIAN_POINT ( 'NONE',  ( -93.86247401662384959, -273.8595552451971002, -223.9810552638743957 ) ) ;
#53072 = CARTESIAN_POINT ( 'NONE',  ( 208.4306832106270804, -324.2391364535881735, 0.000000000000000000 ) ) ;
#53074 = CARTESIAN_POINT ( 'NONE',  ( -43.48000795694964893, -273.8059169533816544, -197.5689391568368194 ) ) ;
#53073 = CARTESIAN_POINT ( 'NONE',  ( -111.7402384325737330, -288.4193012115740657, -282.3304246411586291 ) ) ;
#53075 = CARTESIAN_POINT ( 'NONE',  ( 39.35466548195799419, -287.4595567307200668, -262.9572619183762185 ) ) ;
#53076 = CARTESIAN_POINT ( 'NONE',  ( -26.53034998962469970, -300.1667386724928974, -195.0022827325802837 ) ) ;
#53077 = CARTESIAN_POINT ( 'NONE',  ( -74.22770907569548626, -293.5435474187963223, -335.4721828747001382 ) ) ;
#53078 = CARTESIAN_POINT ( 'NONE',  ( -97.92343253587729635, -283.1164804569623925, -317.6264596162449152 ) ) ;
#53079 = CARTESIAN_POINT ( 'NONE',  ( 197.1656530321902494, 41.90019538913895758, 12.64285714285713169 ) ) ;
#53080 = CARTESIAN_POINT ( 'NONE',  ( 24.49356269736469116, -280.1281015268789361, -312.8931178943216764 ) ) ;
#53081 = CARTESIAN_POINT ( 'NONE',  ( 194.3594942055387094, 21.00000000000000000, -14.50689422379897842 ) ) ;
#53082 = CARTESIAN_POINT ( 'NONE',  ( -99.18454879530479218, -288.8032722392601954, -309.8907596876761090 ) ) ;
#53083 = CARTESIAN_POINT ( 'NONE',  ( -94.38618975279069900, -282.0289136621867669, -317.8668196045017567 ) ) ;
#53084 = DIRECTION ( 'NONE',  ( 0.000000000000000000, 0.000000000000000000, 1.000000000000000000 ) ) ;
#53085 = CARTESIAN_POINT ( 'NONE',  ( -111.3978944739675967, -288.3986596511339258, -282.3029557302596686 ) ) ;
#53086 = CARTESIAN_POINT ( 'NONE',  ( -64.84535885508721265, -275.2064405000169813, -201.9789738510249606 ) ) ;
#53087 = CARTESIAN_POINT ( 'NONE',  ( -94.09460407729157794, -285.0544610868515178, -321.8307052268637563 ) ) ;
#53089 = CARTESIAN_POINT ( 'NONE',  ( -108.0932257389820847, -284.3148596790021543, -288.3394834179954955 ) ) ;
#53088 = CARTESIAN_POINT ( 'NONE',  ( -68.23255946046616316, -271.7294917379506956, -201.3899860719557182 ) ) ;
#53090 = CARTESIAN_POINT ( 'NONE',  ( 5.756450122681592951, -277.8808192620658133, -330.0723936471982825 ) ) ;
#53091 = CARTESIAN_POINT ( 'NONE',  ( 31.41702368083613450, -276.6890631944721122, -295.5051851116778039 ) ) ;
#53092 = CARTESIAN_POINT ( 'NONE',  ( 20.98441271096739413, -284.2015567171311545, -317.5307825527482919 ) ) ;
#53093 = EDGE_LOOP ( 'NONE', ( #37403, #80967, #18124, #33015 ) ) ;
#53094 = CARTESIAN_POINT ( 'NONE',  ( -111.3722443963805944, -270.7948086242133741, -270.3387427897214366 ) ) ;
#53095 = CARTESIAN_POINT ( 'NONE',  ( -19.28934018835978037, -294.6595437023015620, -345.2699430561930285 ) ) ;
#53097 = CARTESIAN_POINT ( 'NONE',  ( 36.90796428035401533, -289.4330935638645315, -262.6907766247290397 ) ) ;
#53096 = VECTOR ( 'NONE', #53842, 1000.000000000000000 ) ;
#53098 = CARTESIAN_POINT ( 'NONE',  ( 195.8534385314006556, 25.84060167483426085, 14.48761588863094119 ) ) ;
#53099 = CARTESIAN_POINT ( 'NONE',  ( 25.22466315766302358, -290.4094976428775112, -220.5068182859052968 ) ) ;
#53100 = CARTESIAN_POINT ( 'NONE',  ( -99.17047664396717721, -278.0777680996212098, -224.9661163902325995 ) ) ;
#53101 = CARTESIAN_POINT ( 'NONE',  ( -25.12936684835842627, -290.6052608892674129, -195.1460973443744535 ) ) ;
#53102 = EDGE_CURVE ( 'NONE', #70513, #47159, #18173, .T. ) ;
#53103 = CARTESIAN_POINT ( 'NONE',  ( -106.2197743360474789, -286.4188098488127139, -244.1596171725175282 ) ) ;
#53104 = CARTESIAN_POINT ( 'NONE',  ( -104.2959747123585714, -280.7341000127553912, -238.6953854289459684 ) ) ;
#53105 = CARTESIAN_POINT ( 'NONE',  ( -5.039664744714470679, -287.8943973664414102, -201.1138450738742165 ) ) ;
#53106 = CARTESIAN_POINT ( 'NONE',  ( 25.82836802917675101, -284.0977715741896077, -310.8861224016510505 ) ) ;
#53107 = CARTESIAN_POINT ( 'NONE',  ( 38.73609110630037122, -275.8716117948317219, -282.5773027869169027 ) ) ;
#53108 = CARTESIAN_POINT ( 'NONE',  ( -61.01415464943616485, -295.7636101426791129, -199.5147726885362829 ) ) ;
#53109 = CARTESIAN_POINT ( 'NONE',  ( -112.7171070979885172, -278.5830350032547358, -254.5638826296090542 ) ) ;
#53110 = CARTESIAN_POINT ( 'NONE',  ( -39.22887118328734601, -299.9484728844831238, -195.9323858445324618 ) ) ;
#53111 = CARTESIAN_POINT ( 'NONE',  ( 157.9772837799791319, 17.93151222991711791, 10.94239627425259442 ) ) ;
#53112 = CARTESIAN_POINT ( 'NONE',  ( 35.77081079830085031, -277.8376638359845288, -253.6410175316879361 ) ) ;
#53113 = CARTESIAN_POINT ( 'NONE',  ( -79.91111264041815332, -295.6230357541203375, -207.6230913565478318 ) ) ;
#53114 = CARTESIAN_POINT ( 'NONE',  ( 202.9738562182569694, 291.9636489450776367, -53.99999999998589573 ) ) ;
#53115 = CARTESIAN_POINT ( 'NONE',  ( -78.67197487995659344, -277.1329472997456378, -330.6705213806835104 ) ) ;
#53116 = CARTESIAN_POINT ( 'NONE',  ( -58.02921237668380172, -274.9958717929322347, -196.5493790434523476 ) ) ;
#53117 = CARTESIAN_POINT ( 'NONE',  ( 38.43364710046513721, -280.7660423054147145, -282.7279770925704270 ) ) ;
#53118 = CARTESIAN_POINT ( 'NONE',  ( -69.17376816947050600, -291.2369097079285893, -337.1794796870520372 ) ) ;
#53119 = CARTESIAN_POINT ( 'NONE',  ( -107.7279442483919780, -297.6924742345010486, -299.9678498616898423 ) ) ;
#53120 = CARTESIAN_POINT ( 'NONE',  ( -113.3824888224443157, -297.8736747972851049, -261.0979018603624695 ) ) ;
#53121 = CARTESIAN_POINT ( 'NONE',  ( 20.75333946067408775, -294.9010370192700634, -223.1710098276439282 ) ) ;
#53122 = CARTESIAN_POINT ( 'NONE',  ( 20.75973241486496690, -280.2031966318053264, -317.5432843601915351 ) ) ;
#53123 = CARTESIAN_POINT ( 'NONE',  ( 34.49695675517361337, -283.2190327955023008, -250.8054480651313440 ) ) ;
#53124 = CARTESIAN_POINT ( 'NONE',  ( -111.2067164228949849, -270.7156358070457713, -259.2473669982903743 ) ) ;
#53125 = CARTESIAN_POINT ( 'NONE',  ( -112.2160862844201716, -286.3345478224298404, -255.9346161509436968 ) ) ;
#53126 = CARTESIAN_POINT ( 'NONE',  ( 35.58328662822450639, -286.3740230092009824, -262.8662944469925264 ) ) ;
#53127 = CARTESIAN_POINT ( 'NONE',  ( 7.222567447766102156, -59.30128903974464549, -354.3697514511841291 ) ) ;
#53128 = ORIENTED_EDGE ( 'NONE', *, *, #3249, .F. ) ;
#53129 = CARTESIAN_POINT ( 'NONE',  ( 28.38757444900029014, -286.6384726524639177, -309.3260862918506859 ) ) ;
#53130 = CARTESIAN_POINT ( 'NONE',  ( 30.99588644589087139, -286.8739020207829640, -244.4877991421641354 ) ) ;
#53131 = ORIENTED_EDGE ( 'NONE', *, *, #2228, .F. ) ;
#53132 = CARTESIAN_POINT ( 'NONE',  ( -8.143784945859268376, -283.7583993691098385, -341.3326965424229797 ) ) ;
#53133 = CARTESIAN_POINT ( 'NONE',  ( 32.87917625717777526, -275.6185522417418383, -250.1525995261814046 ) ) ;
#53134 = CARTESIAN_POINT ( 'NONE',  ( -25.05735290322474640, -291.1256340710792756, -194.6604751697547329 ) ) ;
#53135 = CARTESIAN_POINT ( 'NONE',  ( 33.47530174809608638, -282.5870429639839472, -300.4682081209094804 ) ) ;
#53136 = EDGE_CURVE ( 'NONE', #20475, #27913, #83175, .T. ) ;
#53137 = CARTESIAN_POINT ( 'NONE',  ( 37.30236197100010287, -282.8715525308364249, -254.4565934074510380 ) ) ;
#53138 = CARTESIAN_POINT ( 'NONE',  ( 24.24074137218694958, -282.5003303425487502, -316.5492895254176346 ) ) ;
#53139 = CARTESIAN_POINT ( 'NONE',  ( -5.558494192811491708, -280.4822903412832602, -204.6433287586655183 ) ) ;
#53140 = CARTESIAN_POINT ( 'NONE',  ( 27.33386217378598815, -291.4809262143062369, -301.5434626090942629 ) ) ;
#53141 = CARTESIAN_POINT ( 'NONE',  ( 139.4746202765078635, 180.3694368708648881, -241.5727912977973517 ) ) ;
#53142 = ORIENTED_EDGE ( 'NONE', *, *, #20462, .F. ) ;
#53143 = CARTESIAN_POINT ( 'NONE',  ( 12.99937841255446891, -278.3477951860328972, -325.8011604366477627 ) ) ;
#53144 = CARTESIAN_POINT ( 'NONE',  ( 184.6061638061233623, 263.7319966466967571, -153.1343895057649149 ) ) ;
#53145 = CARTESIAN_POINT ( 'NONE',  ( 18.30545796200765452, -278.8762099623819495, -220.6093280588681296 ) ) ;
#53146 = CARTESIAN_POINT ( 'NONE',  ( -66.85289343556999597, -297.0035275889329682, -203.4670629724890887 ) ) ;
#53147 = CARTESIAN_POINT ( 'NONE',  ( 4.113661539522734500, -292.1020349893318553, -205.4829984225391968 ) ) ;
#53148 = CARTESIAN_POINT ( 'NONE',  ( 6.586641810477393832, -59.71310429701481581, -351.1713004201100716 ) ) ;
#53150 = CARTESIAN_POINT ( 'NONE',  ( -111.1675578940935480, -288.9773369555932732, -268.4206126772065204 ) ) ;
#53149 = CARTESIAN_POINT ( 'NONE',  ( -113.6876631197567207, -271.3089124547065012, -264.6462902796607750 ) ) ;
#53151 = CARTESIAN_POINT ( 'NONE',  ( -94.88522819567236866, -297.7594964438854390, -317.2810664774769407 ) ) ;
#53152 = CARTESIAN_POINT ( 'NONE',  ( 0.4076873518200785917, -287.8812678645984420, -207.2444627014909315 ) ) ;
#53153 = ORIENTED_EDGE ( 'NONE', *, *, #49214, .F. ) ;
#53154 = CARTESIAN_POINT ( 'NONE',  ( 8.700195859958466116, -293.6068816611182228, -208.8703248258991607 ) ) ;
#53155 = CARTESIAN_POINT ( 'NONE',  ( -97.41010596873425698, -285.6237138482405840, -228.7484364484415380 ) ) ;
#53156 = CARTESIAN_POINT ( 'NONE',  ( -87.19216369623259766, -296.1706932979686258, -212.1281569087043692 ) ) ;
#53157 = CARTESIAN_POINT ( 'NONE',  ( -30.72139348939228043, -292.9365220751944889, -193.7556757403533823 ) ) ;
#53158 = CARTESIAN_POINT ( 'NONE',  ( -7.220078199748824588, -292.9291235076543671, -199.5498112497721479 ) ) ;
#53159 = CARTESIAN_POINT ( 'NONE',  ( -108.9383144368351282, -290.5300720249093729, -284.6702148773316594 ) ) ;
#53160 = ORIENTED_EDGE ( 'NONE', *, *, #15556, .F. ) ;
#53161 = CARTESIAN_POINT ( 'NONE',  ( 158.5846220834750397, 17.78059845260490590, 9.675371801486511103 ) ) ;
#53162 = CARTESIAN_POINT ( 'NONE',  ( -65.11169700461144316, -299.5536969880821516, -199.8129591888135792 ) ) ;
#53163 = CARTESIAN_POINT ( 'NONE',  ( -93.84197009086221897, -272.0544989609218192, -218.6143137164453378 ) ) ;
#53164 = ADVANCED_FACE ( 'NONE', ( #61062 ), #17954, .T. ) ;
#53165 = CARTESIAN_POINT ( 'NONE',  ( 21.19075931006214120, -281.2272264910766921, -314.3972846656168940 ) ) ;
#53166 = ORIENTED_EDGE ( 'NONE', *, *, #51325, .F. ) ;
#53167 = VERTEX_POINT ( 'NONE', #69083 ) ;
#53168 = CARTESIAN_POINT ( 'NONE',  ( -20.14596317591239583, -276.3447053597206491, -345.4080151431380159 ) ) ;
#53169 = CARTESIAN_POINT ( 'NONE',  ( -110.9855806072527145, -271.0241451809015985, -264.8334572699994851 ) ) ;
#53170 = CARTESIAN_POINT ( 'NONE',  ( -101.8974378896173363, -280.9061790864847694, -233.7083936606909162 ) ) ;
#53171 = CARTESIAN_POINT ( 'NONE',  ( 20.12295111955519644, -274.3463404851326004, -317.3777291786734054 ) ) ;
#53172 = AXIS2_PLACEMENT_3D ( 'NONE', #12189, #77060, #32583 ) ;
#53173 = CARTESIAN_POINT ( 'NONE',  ( -110.4936033283150749, -297.6707798004966889, -276.9504786201209754 ) ) ;
#53174 = CARTESIAN_POINT ( 'NONE',  ( -110.5769942451401704, -273.4932526910073989, -270.3730743911539776 ) ) ;
#53175 = CARTESIAN_POINT ( 'NONE',  ( -54.43572055365810769, -299.4362059628888915, -196.1032235936009727 ) ) ;
#53176 = CARTESIAN_POINT ( 'NONE',  ( 16.92304405480740215, -272.8400972220205745, -218.0009651343474957 ) ) ;
#53177 = CARTESIAN_POINT ( 'NONE',  ( -4.283151202243660194, -295.2558588116890519, -335.5750214408553234 ) ) ;
#53178 = CARTESIAN_POINT ( 'NONE',  ( -38.89194050737955166, -290.6070517462883345, -196.7882175810221952 ) ) ;
#53179 = DIRECTION ( 'NONE',  ( 0.000000000000000000, 0.000000000000000000, -1.000000000000000000 ) ) ;
#53180 = CARTESIAN_POINT ( 'NONE',  ( -51.29529987717894102, -277.7183217067786245, -346.0236844015495308 ) ) ;
#53181 = CARTESIAN_POINT ( 'NONE',  ( -39.17311196632604009, -298.3618566532203999, -197.3505314855477479 ) ) ;
#53182 = VECTOR ( 'NONE', #37707, 1000.000000000000000 ) ;
#53183 = CARTESIAN_POINT ( 'NONE',  ( 4.263380231796848108, -281.1890568535980606, -334.6289856000636860 ) ) ;
#53184 = CARTESIAN_POINT ( 'NONE',  ( 23.41969440745005571, -296.1541468766243383, -314.6330216019263162 ) ) ;
#53185 = ADVANCED_FACE ( 'NONE', ( #3753 ), #54391, .F. ) ;
#53186 = CARTESIAN_POINT ( 'NONE',  ( 219.8344101925596021, 35.72494958537217968, -7.000000000000000888 ) ) ;
#53187 = CARTESIAN_POINT ( 'NONE',  ( -65.38703105931877246, -282.6255385255211081, -337.9473835880162369 ) ) ;
#53188 = CARTESIAN_POINT ( 'NONE',  ( -111.7873673732580357, -282.4142092780639928, -281.1157403056614044 ) ) ;
#53189 = CARTESIAN_POINT ( 'NONE',  ( 27.16168139506032730, -273.6456624114957776, -234.8332814406924740 ) ) ;
#53190 = CARTESIAN_POINT ( 'NONE',  ( 23.91032801655921958, -282.9640423458236569, -227.0588760057046613 ) ) ;
#53191 = CARTESIAN_POINT ( 'NONE',  ( 160.5350683151633291, 275.0000000000000568, 20.22542485937379908 ) ) ;
#53192 = FACE_OUTER_BOUND ( 'NONE', #47547, .T. ) ;
#53193 = CARTESIAN_POINT ( 'NONE',  ( -21.50100266378104052, -272.6518762875633115, -195.8258061011742086 ) ) ;
#53194 = CARTESIAN_POINT ( 'NONE',  ( -79.18398686719039858, -279.6149906439246138, -332.8677480620823417 ) ) ;
#53195 = DIRECTION ( 'NONE',  ( -1.000000000000000000, -0.000000000000000000, -0.000000000000000000 ) ) ;
#53196 = CARTESIAN_POINT ( 'NONE',  ( -70.45759954843084927, -287.5391475790112850, -202.4446147732228951 ) ) ;
#53197 = CARTESIAN_POINT ( 'NONE',  ( 156.0603832538683093, 17.29324094227624187, -10.42473456490740169 ) ) ;
#53198 = CARTESIAN_POINT ( 'NONE',  ( -111.7067687828262166, -288.6819412171976182, -260.2402206439201109 ) ) ;
#53199 = LINE ( 'NONE', #46097, #11956 ) ;
#53200 = CARTESIAN_POINT ( 'NONE',  ( -108.5564991955320266, -295.5808450781406123, -252.5450553201070250 ) ) ;
#53201 = CARTESIAN_POINT ( 'NONE',  ( -76.54074725841762472, -287.7222619714048051, -333.4031688978202510 ) ) ;
#53202 = CARTESIAN_POINT ( 'NONE',  ( -72.76141013609318975, -193.8959084914727669, -354.0272458012134393 ) ) ;
#53203 = CARTESIAN_POINT ( 'NONE',  ( -111.3402603691592674, -294.3951485864391771, -282.5764252751562253 ) ) ;
#53204 = CARTESIAN_POINT ( 'NONE',  ( 38.10302698336676741, -285.8866013197556981, -258.8371542206519962 ) ) ;
#53205 = CARTESIAN_POINT ( 'NONE',  ( 28.48585653638552984, -282.7028302378168974, -236.8836160027974245 ) ) ;
#53206 = CARTESIAN_POINT ( 'NONE',  ( -47.14808262679986939, -281.4149660246019380, -345.7123546981116533 ) ) ;
#53207 = CARTESIAN_POINT ( 'NONE',  ( -94.29090639493006165, -291.1978081416179407, -224.6708273778320972 ) ) ;
#53208 = CARTESIAN_POINT ( 'NONE',  ( 31.61614055084014652, -282.6357301102995052, -244.5208381995067271 ) ) ;
#53209 = CARTESIAN_POINT ( 'NONE',  ( 35.59088192707488219, -282.4391504593885429, -276.7551007935517191 ) ) ;
#53210 = CARTESIAN_POINT ( 'NONE',  ( 17.46619677065141119, -290.2536437759505930, -322.0766982301693133 ) ) ;
#53211 = CARTESIAN_POINT ( 'NONE',  ( -97.79909679341338347, -273.5229275846163546, -222.7098065618112059 ) ) ;
#53212 = CARTESIAN_POINT ( 'NONE',  ( 18.54243952888901958, -286.3365617539775485, -321.2358361579501889 ) ) ;
#53213 = CARTESIAN_POINT ( 'NONE',  ( 31.25029666173524845, -275.1015462326435568, -235.3734347728104694 ) ) ;
#53214 = CARTESIAN_POINT ( 'NONE',  ( 28.93565103743292966, -295.0753337591519880, -236.0222257148051597 ) ) ;
#53215 = DIRECTION ( 'NONE',  ( 0.000000000000000000, 0.000000000000000000, 1.000000000000000000 ) ) ;
#53216 = CARTESIAN_POINT ( 'NONE',  ( 10.59707575819634329, -283.1948066931273047, -210.1954327657594490 ) ) ;
#53217 = CARTESIAN_POINT ( 'NONE',  ( 30.19655231208273705, -273.9873451788620287, -303.4737239230440196 ) ) ;
#53218 = FACE_OUTER_BOUND ( 'NONE', #70755, .T. ) ;
#53219 = CARTESIAN_POINT ( 'NONE',  ( -104.5384193880964006, -295.4225277694550300, -234.3181771353212355 ) ) ;
#53220 = CARTESIAN_POINT ( 'NONE',  ( -110.0686411521480608, -292.3197179683884315, -257.5296459578963209 ) ) ;
#53221 = CARTESIAN_POINT ( 'NONE',  ( -74.31779062108446965, -272.8954765581785296, -207.2417080407740286 ) ) ;
#53222 = CARTESIAN_POINT ( 'NONE',  ( -92.20213089438688314, -292.7699762491427009, -221.1381636908673158 ) ) ;
#53223 = CARTESIAN_POINT ( 'NONE',  ( -86.09457117559314554, -292.2979480365151517, -215.6433673060070930 ) ) ;
#53224 = CARTESIAN_POINT ( 'NONE',  ( -110.6185932857513166, -286.4478074503168727, -259.9461795396508705 ) ) ;
#53225 = CARTESIAN_POINT ( 'NONE',  ( -111.0690885312376821, -292.2313127495139611, -250.2395914609065812 ) ) ;
#53226 = CARTESIAN_POINT ( 'NONE',  ( -27.92649790953471367, -293.4843411741887849, -194.3824814416859681 ) ) ;
#53227 = CARTESIAN_POINT ( 'NONE',  ( 14.31477911683075988, -294.1346789447569563, -322.0132735675327922 ) ) ;
#53228 = CARTESIAN_POINT ( 'NONE',  ( 35.97096331013060677, -289.7561556857563119, -286.2408678831799307 ) ) ;
#53229 = CARTESIAN_POINT ( 'NONE',  ( 36.17507721616056671, -281.4311824980786696, -247.4638811749261436 ) ) ;
#53230 = CARTESIAN_POINT ( 'NONE',  ( -103.1447997570861190, -271.1886675844338015, -232.7024905364028768 ) ) ;
#53231 = CARTESIAN_POINT ( 'NONE',  ( -112.2196487879977838, -284.1602541102888040, -288.3694544525799870 ) ) ;
#53232 = CARTESIAN_POINT ( 'NONE',  ( 34.83900185257586912, -277.7776690860425788, -289.3819767158265677 ) ) ;
#53233 = EDGE_CURVE ( 'NONE', #90307, #93354, #76647, .T. ) ;
#53234 = CARTESIAN_POINT ( 'NONE',  ( -102.1289017722122310, -282.8782940458734174, -304.9620689189410996 ) ) ;
#53235 = CARTESIAN_POINT ( 'NONE',  ( 19.94447813150229365, -286.2215906952047249, -318.7687044986275282 ) ) ;
#53236 = CARTESIAN_POINT ( 'NONE',  ( -95.22116186246697112, -276.0221612431938638, -319.2715726048051010 ) ) ;
#53238 = VECTOR ( 'NONE', #83557, 1000.000000000000000 ) ;
#53237 = CARTESIAN_POINT ( 'NONE',  ( 144.2857639756989272, -299.5541904835127980, -195.3611179825600175 ) ) ;
#53239 = CARTESIAN_POINT ( 'NONE',  ( -88.94218930997929817, -283.3087520617530117, -322.1561914821513142 ) ) ;
#53240=STYLED_ITEM('',(#93745),#58557);
#53241 = CARTESIAN_POINT ( 'NONE',  ( -94.67484783465863529, -280.4490567075629315, -219.5583730451570830 ) ) ;
#53242 = CARTESIAN_POINT ( 'NONE',  ( 27.24033664975637237, -287.1580777940153553, -311.9558621771410571 ) ) ;
#53243 = CARTESIAN_POINT ( 'NONE',  ( 35.84337314420839959, -295.4603078293741305, -281.7368349655928341 ) ) ;
#53244 = CARTESIAN_POINT ( 'NONE',  ( 23.82539689038724617, -276.5416842638102821, -224.9185535801931621 ) ) ;
#53245 = CARTESIAN_POINT ( 'NONE',  ( 36.41469916907177407, -277.1241894832037929, -290.7395866213784075 ) ) ;
#53246 = CARTESIAN_POINT ( 'NONE',  ( -27.02361157036015626, -276.7506197147289413, -342.6282408878328170 ) ) ;
#53247 = CARTESIAN_POINT ( 'NONE',  ( -95.91880397987304718, -275.1704977573533029, -224.0948266738041923 ) ) ;
#53248 = CARTESIAN_POINT ( 'NONE',  ( 34.02960341810776868, -285.2605713031388746, -247.8200497228821177 ) ) ;
#53249 = AXIS2_PLACEMENT_3D ( 'NONE', #48314, #5725, #34600 ) ;
#53250 = CARTESIAN_POINT ( 'NONE',  ( -92.99443189435838519, -291.4342873639084814, -322.4872485198813479 ) ) ;
#53251 = CARTESIAN_POINT ( 'NONE',  ( -7.876631510554272353, -293.5770968422284000, -337.5017639540419054 ) ) ;
#53252 = ORIENTED_EDGE ( 'NONE', *, *, #16816, .F. ) ;
#53253 = CARTESIAN_POINT ( 'NONE',  ( -69.02293574344011517, -291.2904329886188179, -204.5568346340573100 ) ) ;
#53254 = ORIENTED_EDGE ( 'NONE', *, *, #1367, .T. ) ;
#53255 = CARTESIAN_POINT ( 'NONE',  ( -87.17310460768425173, -290.8069482824485590, -328.7260013536424594 ) ) ;
#53256 = CARTESIAN_POINT ( 'NONE',  ( -108.3906952617237778, -279.4302199975909389, -253.1584158969775729 ) ) ;
#53257 = CARTESIAN_POINT ( 'NONE',  ( -112.9017446749930542, -295.3039497443256778, -283.7829506566654345 ) ) ;
#53258 = CARTESIAN_POINT ( 'NONE',  ( 37.92202597641377793, -288.0052802938665764, -254.5276652446351591 ) ) ;
#53259 = EDGE_CURVE ( 'NONE', #3537, #10408, #30274, .T. ) ;
#53260 = CARTESIAN_POINT ( 'NONE',  ( 37.12503845127565683, -288.1296532977685274, -289.8662233899973444 ) ) ;
#53261 = CARTESIAN_POINT ( 'NONE',  ( -108.0501975829110535, -285.1260389607461434, -252.1293908419040122 ) ) ;
#53262 = CARTESIAN_POINT ( 'NONE',  ( 84.36106466651209246, 83.41242399426737109, -302.2512376199425717 ) ) ;
#53263 = CARTESIAN_POINT ( 'NONE',  ( 195.6868322499005046, 284.9009392118488790, -111.2773971726515470 ) ) ;
#53264 = CARTESIAN_POINT ( 'NONE',  ( -108.1557645722374303, -264.0394726077588530, -305.3744954675115650 ) ) ;
#53265 = CARTESIAN_POINT ( 'NONE',  ( -92.85582339289652509, -277.0723915473839156, -318.0138602488598849 ) ) ;
#53266 = CARTESIAN_POINT ( 'NONE',  ( -110.4777982728515013, -277.3972277977297836, -276.0894038606994059 ) ) ;
#53267 = CARTESIAN_POINT ( 'NONE',  ( -101.1886334701071064, -272.7866564770629338, -227.2625840664813666 ) ) ;
#53268 = CARTESIAN_POINT ( 'NONE',  ( -101.2118702128279324, -255.6233436704357018, -324.8885547363302067 ) ) ;
#53269 = CARTESIAN_POINT ( 'NONE',  ( -9.407574802891977228, -275.3793965981718088, -341.5859936591876931 ) ) ;
#53270 = CARTESIAN_POINT ( 'NONE',  ( -104.1013986831535334, -290.6437312344595512, -300.1698877893368262 ) ) ;
#53271 = CARTESIAN_POINT ( 'NONE',  ( 76.08029918769435085, -300.2411797159293769, -193.5075115251480895 ) ) ;
#53272 = CARTESIAN_POINT ( 'NONE',  ( 36.14815395606711945, -286.2460945185633818, -271.0574104906677917 ) ) ;
#53273 = CARTESIAN_POINT ( 'NONE',  ( -3.450481238932981753, -298.9581682151539894, -193.4199041260204410 ) ) ;
#53274 = CARTESIAN_POINT ( 'NONE',  ( -90.40577614855953925, -295.9960482218384072, -320.5657778681049308 ) ) ;
#53275 = ORIENTED_EDGE ( 'NONE', *, *, #39657, .F. ) ;
#53276 = CARTESIAN_POINT ( 'NONE',  ( -59.22417564993066463, -279.2533840340722691, -342.6831164397335101 ) ) ;
#53277 = EDGE_CURVE ( 'NONE', #91480, #3443, #78673, .T. ) ;
#53278 = CARTESIAN_POINT ( 'NONE',  ( 38.36389194211682963, -281.2324255043786252, -284.1525077467491087 ) ) ;
#53279 = B_SPLINE_CURVE_WITH_KNOTS ( 'NONE', 3,
 ( #49104, #64290, #92637, #27330 ),
 .UNSPECIFIED., .F., .F.,
 ( 4, 4 ),
 ( 3.469446951953614189E-18, 0.001032491475659819006 ),
 .UNSPECIFIED. ) ;
#53280 = CARTESIAN_POINT ( 'NONE',  ( -96.66389756162209324, -280.2320419986169782, -227.2902117246974285 ) ) ;
#53281 = CARTESIAN_POINT ( 'NONE',  ( -62.05495501160649496, -279.1291277436454834, -342.2722915213602164 ) ) ;
#53282 = CARTESIAN_POINT ( 'NONE',  ( -90.45870103370764070, -295.8567138240070449, -219.3572883281996724 ) ) ;
#53283 = CYLINDRICAL_SURFACE ( 'NONE', #33639, 5.568361562975243650 ) ;
#53284 = CARTESIAN_POINT ( 'NONE',  ( -96.09174159185934627, -278.1112956120808803, -313.7114205486456626 ) ) ;
#53285 = CARTESIAN_POINT ( 'NONE',  ( -105.4705123126592667, -273.8156153054890183, -234.7126731335976899 ) ) ;
#53286 = CARTESIAN_POINT ( 'NONE',  ( 16.63212666722990463, -276.8195081145228755, -218.2113917777019765 ) ) ;
#53287 = CARTESIAN_POINT ( 'NONE',  ( 25.57133689010938937, -274.7048791307898341, -313.8180464572321853 ) ) ;
#53288 = CARTESIAN_POINT ( 'NONE',  ( 157.7374095173865385, 14.19731191252289015, 13.00000000000000178 ) ) ;
#53289 = CARTESIAN_POINT ( 'NONE',  ( -102.9948276916164076, -289.3128295293842029, -302.6453024626476918 ) ) ;
#53290 = ADVANCED_FACE ( 'NONE', ( #40625 ), #6086, .T. ) ;
#53291 = CARTESIAN_POINT ( 'NONE',  ( -97.49547028825384132, -284.5429643603194449, -222.4566638813180646 ) ) ;
#53292 = CARTESIAN_POINT ( 'NONE',  ( 22.95182841329831902, -279.2006047116560694, -227.4348506080987420 ) ) ;
#53294 = CARTESIAN_POINT ( 'NONE',  ( -40.00135534845858842, -284.0983164198792679, -195.9686423258791024 ) ) ;
#53293 = CARTESIAN_POINT ( 'NONE',  ( 34.51184905986551854, -280.3347945101170353, -286.2495536558953404 ) ) ;
#53295 = CARTESIAN_POINT ( 'NONE',  ( -8.371534899360042914, -290.6730724307741411, -339.5537669755875072 ) ) ;
#53296 = CARTESIAN_POINT ( 'NONE',  ( -46.52125161606375059, -281.1382826988426586, -197.4889545147629804 ) ) ;
#53297 = CARTESIAN_POINT ( 'NONE',  ( -95.79649060784740300, -239.9130894949069273, -341.7038789641651420 ) ) ;
#53298 = CIRCLE ( 'NONE', #76018, 24.00000000000001066 ) ;
#53299 = CARTESIAN_POINT ( 'NONE',  ( -73.91016683735213633, -281.9289795067448381, -337.2719819784207402 ) ) ;
#53300 = CARTESIAN_POINT ( 'NONE',  ( 36.63783524064525920, -295.7116295160258232, -282.7690944289590220 ) ) ;
#53301 = CARTESIAN_POINT ( 'NONE',  ( -86.13662427978462688, -277.6264869320473281, -212.0428378762436239 ) ) ;
#53302 = CARTESIAN_POINT ( 'NONE',  ( -60.63866816184651043, -285.3536961940569654, -341.8807036344308017 ) ) ;
#53303 = AXIS2_PLACEMENT_3D ( 'NONE', #59518, #10219, #39086 ) ;
#53304 = CARTESIAN_POINT ( 'NONE',  ( 197.1513938986460062, -147.7221692137691775, 1.978481845683761620 ) ) ;
#53305 = CARTESIAN_POINT ( 'NONE',  ( -28.05086643719268835, -294.0892237539399048, -195.3218194102945517 ) ) ;
#53306 = CIRCLE ( 'NONE', #1889, 24.00000000000001066 ) ;
#53307 = CARTESIAN_POINT ( 'NONE',  ( 35.45645305944830028, -273.3202936041259363, -252.3214521044563980 ) ) ;
#53308 = CARTESIAN_POINT ( 'NONE',  ( 37.34504015396549192, -286.9762866145327962, -288.4735153254003990 ) ) ;
#53309 = CARTESIAN_POINT ( 'NONE',  ( -105.4334054509244538, -289.3312277487780761, -241.7684228450832506 ) ) ;
#53310 = CARTESIAN_POINT ( 'NONE',  ( -48.18343439339478351, -271.8438693890086029, -432.6084584992419195 ) ) ;
#53311 = CARTESIAN_POINT ( 'NONE',  ( 35.59335598344972595, -274.3607329713705099, -279.8062133709154864 ) ) ;
#53312 = CARTESIAN_POINT ( 'NONE',  ( -20.59213019760519714, -292.9745255301173756, -342.7350333072060380 ) ) ;
#53313 = CARTESIAN_POINT ( 'NONE',  ( -108.5906737121535457, -292.1042083185274691, -252.2869241974576937 ) ) ;
#53314 = LINE ( 'NONE', #31096, #17027 ) ;
#53315 = CARTESIAN_POINT ( 'NONE',  ( -5.802570524182335987, -229.5268262511776527, 25.50000000000000000 ) ) ;
#53316 = CARTESIAN_POINT ( 'NONE',  ( 38.91330782135023014, -292.0674607705779522, -273.1685213399239274 ) ) ;
#53317 = CARTESIAN_POINT ( 'NONE',  ( 35.31282047177651151, -289.3212938334405635, -283.3133785098077624 ) ) ;
#53318 = CARTESIAN_POINT ( 'NONE',  ( 2.627798813909436149, -286.7642557421354468, -335.0480066675617081 ) ) ;
#53319 = CARTESIAN_POINT ( 'NONE',  ( 34.27962083901346091, -288.7555012119815387, -253.4022385556386041 ) ) ;
#53320 = CARTESIAN_POINT ( 'NONE',  ( -83.63170945779074827, -298.0521521680024080, -521.1711561948568487 ) ) ;
#53321 = CARTESIAN_POINT ( 'NONE',  ( 25.08318942048913769, -287.8304560759564197, -232.2070239481237195 ) ) ;
#53322 = CARTESIAN_POINT ( 'NONE',  ( 12.33096567822983936, -296.3449497253816389, -327.0963018696066342 ) ) ;
#53323 = CARTESIAN_POINT ( 'NONE',  ( 11.63197158325052172, -331.8906705383788562, 52.50000000000000711 ) ) ;
#53324 = CARTESIAN_POINT ( 'NONE',  ( -29.51882367111351257, -287.3542226296139575, -194.1586815245778723 ) ) ;
#53325 = CARTESIAN_POINT ( 'NONE',  ( -45.51855283331879320, -275.2347078105296418, -345.5294498129835006 ) ) ;
#53326 = CARTESIAN_POINT ( 'NONE',  ( -112.1536246696261827, -278.6578606600517674, -288.5524745620706426 ) ) ;
#53327 = CARTESIAN_POINT ( 'NONE',  ( -45.26697170667152648, -279.6212228549536576, -193.7383416711709572 ) ) ;
#53328 = CARTESIAN_POINT ( 'NONE',  ( -109.7770570454589460, -298.7652977454988559, -252.2819061632672799 ) ) ;
#53329 = CARTESIAN_POINT ( 'NONE',  ( -42.79480560662226196, -283.9831991590132247, -195.5466472428230134 ) ) ;
#53330 = CARTESIAN_POINT ( 'NONE',  ( 165.0427047786672290, 250.0000000000000568, 23.37680765314704701 ) ) ;
#53331 = CARTESIAN_POINT ( 'NONE',  ( -71.48911177423597962, -277.7357922077416106, -204.4315472810838799 ) ) ;
#53332 = CARTESIAN_POINT ( 'NONE',  ( -87.01645424888360481, -281.7431171264859131, -326.6214025603719051 ) ) ;
#53333 = CARTESIAN_POINT ( 'NONE',  ( -5.802570524182335987, -229.5268262511776527, 22.50000000000000000 ) ) ;
#53334 = CARTESIAN_POINT ( 'NONE',  ( 22.08871162433874957, -274.6795556270596990, -318.2433910655992122 ) ) ;
#53335 = CARTESIAN_POINT ( 'NONE',  ( -104.3570865205281422, -298.4832359403894770, -239.5845805086292444 ) ) ;
#53336 = CIRCLE ( 'NONE', #35248, 4.999999999999990230 ) ;
#53337 = CARTESIAN_POINT ( 'NONE',  ( -41.56591789986394758, -282.0243770713628351, -346.9876977603199180 ) ) ;
#53338 = CARTESIAN_POINT ( 'NONE',  ( -96.29684121857637535, -298.1006036656422111, -226.8922746056790061 ) ) ;
#53339 = CARTESIAN_POINT ( 'NONE',  ( -37.27096458327439166, -299.3681896575296264, -193.8534906611272675 ) ) ;
#53340 = CARTESIAN_POINT ( 'NONE',  ( -48.87459184230568354, -273.5680489240326665, -198.2052845423936276 ) ) ;
#53341 = CARTESIAN_POINT ( 'NONE',  ( 24.98963354731172259, -294.9884647040649384, -228.6501423155503403 ) ) ;
#53342 = CARTESIAN_POINT ( 'NONE',  ( 31.68836297362905086, -288.1585853358938039, -304.5966267694757335 ) ) ;
#53343 = CARTESIAN_POINT ( 'NONE',  ( -25.59488731868887612, -278.2805586575643133, -195.7197984296246318 ) ) ;
#53344 = CARTESIAN_POINT ( 'NONE',  ( -100.0298143814077889, -290.9776920624801733, -225.6486998431002746 ) ) ;
#53345 = EDGE_CURVE ( 'NONE', #11375, #23299, #48438, .T. ) ;
#53346 = CARTESIAN_POINT ( 'NONE',  ( -3.267544394144144437, -287.6496402726385213, -335.2428918257706982 ) ) ;
#53347 = CARTESIAN_POINT ( 'NONE',  ( 35.15604847583838932, -291.3044901863527798, -251.1001245313546519 ) ) ;
#53348 = ORIENTED_EDGE ( 'NONE', *, *, #20584, .T. ) ;
#53349 = FACE_OUTER_BOUND ( 'NONE', #80054, .T. ) ;
#53350 = CARTESIAN_POINT ( 'NONE',  ( 35.02045035014045027, -287.1939285195435900, -280.5371703710089264 ) ) ;
#53351 = CARTESIAN_POINT ( 'NONE',  ( 175.2296996224750103, 161.0000000000000853, 0.000000000000000000 ) ) ;
#53352 = CARTESIAN_POINT ( 'NONE',  ( -95.64572995639733222, -286.1699047810917023, -220.3468183581427695 ) ) ;
#53353 = CARTESIAN_POINT ( 'NONE',  ( 37.83393706612440610, -292.4151704371259370, -254.7581827960663361 ) ) ;
#53354 = CARTESIAN_POINT ( 'NONE',  ( -22.67721911498254528, -281.5511009678966161, -195.2189220750527738 ) ) ;
#53355 = CARTESIAN_POINT ( 'NONE',  ( -26.74487334013010553, -282.7470670097438301, -342.6391941126705660 ) ) ;
#53356 = CARTESIAN_POINT ( 'NONE',  ( -62.84504740938675837, -297.7290993848732228, -197.7072861672377257 ) ) ;
#53357 = CARTESIAN_POINT ( 'NONE',  ( -62.21222647214859336, -275.0369775354597550, -201.2040475043935146 ) ) ;
#53358 = CARTESIAN_POINT ( 'NONE',  ( -25.11539492085915981, -290.2287740458283452, -196.6717721318000827 ) ) ;
#53359 = CARTESIAN_POINT ( 'NONE',  ( -64.70263319476210029, -272.4816827481196810, -202.2409597299379413 ) ) ;
#53360 = ORIENTED_EDGE ( 'NONE', *, *, #52014, .T. ) ;
#53361 = DIRECTION ( 'NONE',  ( -0.8195702660915945570, 1.110223024625169667E-13, 0.5729786897769871823 ) ) ;
#53362 = CARTESIAN_POINT ( 'NONE',  ( -40.05032774112678595, -287.9380037307938096, -195.9704093108784662 ) ) ;
#53363 = CIRCLE ( 'NONE', #38290, 8.000000000000000000 ) ;
#53364 = CARTESIAN_POINT ( 'NONE',  ( -58.75178810823440045, -296.4022886058531867, -344.0581684737222758 ) ) ;
#53365 = CARTESIAN_POINT ( 'NONE',  ( -109.5978189156831348, -285.0532267569257101, -281.7737427951699374 ) ) ;
#53366 = CARTESIAN_POINT ( 'NONE',  ( 39.14504054577020753, -274.6927786480415534, -276.8878869815503663 ) ) ;
#53367 = CARTESIAN_POINT ( 'NONE',  ( 38.25857087792454081, -294.3806283060176838, -284.5004208082049217 ) ) ;
#53368 = CARTESIAN_POINT ( 'NONE',  ( 37.56795767147776388, -285.5463622729420763, -258.9234100637174834 ) ) ;
#53369 = CARTESIAN_POINT ( 'NONE',  ( 32.21273768267857207, -294.3096346340857963, -303.4690914269082782 ) ) ;
#53371 = CARTESIAN_POINT ( 'NONE',  ( -78.18272752374834056, -289.9511686476623709, -330.9537812191658190 ) ) ;
#53370 = AXIS2_PLACEMENT_3D ( 'NONE', #76390, #38973, #83942 ) ;
#53372 = DIRECTION ( 'NONE',  ( -0.9693563597868444237, -0.2456588035076248677, 0.000000000000000000 ) ) ;
#53373 = DIRECTION ( 'NONE',  ( 1.000000000000000000, 0.000000000000000000, 0.000000000000000000 ) ) ;
#53374 = CARTESIAN_POINT ( 'NONE',  ( -76.27077213493787156, -208.3870304207176787, -353.5830081017861062 ) ) ;
#53375 = CARTESIAN_POINT ( 'NONE',  ( -91.42535153035444750, -286.8193444611971472, -216.5311411766099070 ) ) ;
#53376 = CARTESIAN_POINT ( 'NONE',  ( 25.22466315766302358, -272.4094976428775681, -220.5068182859052968 ) ) ;
#53377 = ORIENTED_EDGE ( 'NONE', *, *, #47942, .F. ) ;
#53379 = CARTESIAN_POINT ( 'NONE',  ( -37.55517273856889915, -281.9752483997886543, -343.6824025927108437 ) ) ;
#53378 = AXIS2_PLACEMENT_3D ( 'NONE', #59130, #16961, #30240 ) ;
#53380 = CARTESIAN_POINT ( 'NONE',  ( -107.5585605960603601, -277.8143747117747466, -302.0397986969978774 ) ) ;
#53381 = CARTESIAN_POINT ( 'NONE',  ( 31.70346837328679612, -283.1746699756419048, -241.5029626283152595 ) ) ;
#53382 = CARTESIAN_POINT ( 'NONE',  ( 162.9489142668776935, 218.2876765797497001, -204.1083781671020176 ) ) ;
#53383 = CARTESIAN_POINT ( 'NONE',  ( -3.172738037595201455, -281.1845061363202944, -338.7210183441566755 ) ) ;
#53385 = AXIS2_PLACEMENT_3D ( 'NONE', #38999, #26213, #76420 ) ;
#53384 = CARTESIAN_POINT ( 'NONE',  ( 18.12945107263028888, -284.8727030029602361, -220.3940733625559005 ) ) ;
#53386 = CARTESIAN_POINT ( 'NONE',  ( -72.82762065672925189, -299.3492022156100916, -203.1113437648492095 ) ) ;
#53387 = CARTESIAN_POINT ( 'NONE',  ( -101.5183833719510460, -296.5682730717829827, -305.2801925593935835 ) ) ;
#53388 = ORIENTED_EDGE ( 'NONE', *, *, #65647, .T. ) ;
#53389 = CARTESIAN_POINT ( 'NONE',  ( -41.60480967958189069, -290.6822996497886038, -196.9415307168669642 ) ) ;
#53390 = CARTESIAN_POINT ( 'NONE',  ( -74.04089127183841867, -278.1779915879210989, -337.9518505832722894 ) ) ;
#53391 = CARTESIAN_POINT ( 'NONE',  ( 35.58697269398483343, -275.4964550357007624, -266.1389709784803586 ) ) ;
#53392 = CARTESIAN_POINT ( 'NONE',  ( 20.57773378394159636, -275.1547180929459273, -320.6485899078971897 ) ) ;
#53393 = LINE ( 'NONE', #69474, #74908 ) ;
#53394 = CARTESIAN_POINT ( 'NONE',  ( 2.977554037242769347, -272.5928393528377569, -207.0603478451820365 ) ) ;
#53395 = CARTESIAN_POINT ( 'NONE',  ( -19.40782647434127384, -296.2512398688926396, -344.6919789385186164 ) ) ;
#53396 = CARTESIAN_POINT ( 'NONE',  ( 152.5990036449067588, 20.65770287760360802, 10.64853154254647016 ) ) ;
#53397 = CARTESIAN_POINT ( 'NONE',  ( 195.9765076956177268, 73.46773880466290052, 12.06523745212588494 ) ) ;
#53398 = VECTOR ( 'NONE', #44457, 1000.000000000000000 ) ;
#53399 = CARTESIAN_POINT ( 'NONE',  ( -107.6553532563122388, -285.9072115601640007, -249.4432875828630074 ) ) ;
#53400 = CARTESIAN_POINT ( 'NONE',  ( -87.63385280214104966, -285.5028135864859564, -327.3933905286901336 ) ) ;
#53401 = CARTESIAN_POINT ( 'NONE',  ( -105.3117712919072630, -283.5396761071032188, -297.4054939483576732 ) ) ;
#53402 = CARTESIAN_POINT ( 'NONE',  ( 27.45956058052916759, -274.4301572430983924, -305.7841394545822595 ) ) ;
#53403 = CARTESIAN_POINT ( 'NONE',  ( -6.722722166402029131, -284.5062970015063115, -338.0015672801819733 ) ) ;
#53404 = CARTESIAN_POINT ( 'NONE',  ( -95.83504826728078285, -276.4073625159570611, -315.1856199629881985 ) ) ;
#53405 = CARTESIAN_POINT ( 'NONE',  ( -36.44867144630563871, -278.1204099337319349, -343.6773115128813743 ) ) ;
#53406 = DIRECTION ( 'NONE',  ( -0.000000000000000000, -0.000000000000000000, 1.000000000000000000 ) ) ;
#53407 = CARTESIAN_POINT ( 'NONE',  ( -101.7614368603509689, -279.9072778027917821, -228.3809774570239881 ) ) ;
#53408 = CIRCLE ( 'NONE', #82132, 4.499999999999993783 ) ;
#53409 = CARTESIAN_POINT ( 'NONE',  ( 27.79590931484954197, -281.5067918293200364, -229.3147521019760404 ) ) ;
#53410 = ORIENTED_EDGE ( 'NONE', *, *, #16496, .T. ) ;
#53411 = VERTEX_POINT ( 'NONE', #34963 ) ;
#53412 = CARTESIAN_POINT ( 'NONE',  ( 200.3378311594553622, 16.04715669186298044, -10.05743975622762143 ) ) ;
#53413 = CARTESIAN_POINT ( 'NONE',  ( 0.8777899896498234655, -288.4166783843363078, -204.9275593736371093 ) ) ;
#53414 = CARTESIAN_POINT ( 'NONE',  ( -68.10612323592761186, -296.8347323899274102, -203.9685719074067265 ) ) ;
#53415 = ADVANCED_FACE ( 'NONE', ( #27394 ), #51847, .T. ) ;
#53416 = CARTESIAN_POINT ( 'NONE',  ( -68.02084141694460584, -288.7930953834055003, -340.8742591452510169 ) ) ;
#53417 = CARTESIAN_POINT ( 'NONE',  ( 27.91345556135372874, -286.2628761704095837, -305.3948923158214370 ) ) ;
#53419 = CARTESIAN_POINT ( 'NONE',  ( -106.0621518300596335, -288.4275603878257925, -297.9846536262857057 ) ) ;
#53418 = CARTESIAN_POINT ( 'NONE',  ( 25.46297528865467186, -285.6027102171243541, -232.0081824731794029 ) ) ;
#53420 = CARTESIAN_POINT ( 'NONE',  ( -74.93660346783462955, -286.7444044557256575, -207.3234011161567594 ) ) ;
#53421 = CARTESIAN_POINT ( 'NONE',  ( -50.97472971357520777, -275.2262152481998783, -344.1116512024975691 ) ) ;
#53422 = CARTESIAN_POINT ( 'NONE',  ( -31.90442097226439699, -287.3846355029374990, -346.4188938060080432 ) ) ;
#53423 = CARTESIAN_POINT ( 'NONE',  ( 26.97010465818681624, -289.0344757514233152, -231.6735466715089728 ) ) ;
#53424 = CARTESIAN_POINT ( 'NONE',  ( 22.41972231341030408, -284.9291229476012859, -224.7483309454040636 ) ) ;
#53425 = CARTESIAN_POINT ( 'NONE',  ( 32.45922421033046845, -282.7882833614393121, -292.6902890776049162 ) ) ;
#53426 = CARTESIAN_POINT ( 'NONE',  ( -98.36660046895637777, -291.9561389991337137, -314.2692624980895744 ) ) ;
#53427 = DIRECTION ( 'NONE',  ( 1.000000000000000000, 4.095251346825557639E-15, 0.000000000000000000 ) ) ;
#53428 = CYLINDRICAL_SURFACE ( 'NONE', #27708, 6.000000000000000000 ) ;
#53429 = CARTESIAN_POINT ( 'NONE',  ( -111.1982760520480866, -298.6763485988056459, -254.3469390481135122 ) ) ;
#53430 = CARTESIAN_POINT ( 'NONE',  ( 13.45455668918196501, -279.9822231923999425, -217.6374746305969836 ) ) ;
#53431 = CARTESIAN_POINT ( 'NONE',  ( 33.22803067003570732, -279.8829693749308944, -295.9096774006114288 ) ) ;
#53432 = CARTESIAN_POINT ( 'NONE',  ( 23.89408600486299505, -293.3690069489301209, -316.7759573956556665 ) ) ;
#53433 = CARTESIAN_POINT ( 'NONE',  ( -34.42000716631464030, -296.4891925136792565, -196.5619242977774661 ) ) ;
#53434 = CARTESIAN_POINT ( 'NONE',  ( 34.55109611369488221, -280.0363492217385897, -255.0475872451824557 ) ) ;
#53435 = CARTESIAN_POINT ( 'NONE',  ( 3.912214931269825779, -274.5716672616509868, -332.3242415992071415 ) ) ;
#53436 = CARTESIAN_POINT ( 'NONE',  ( -38.33225214234089151, -296.3800019997042909, -343.8475948761143854 ) ) ;
#53437 = SURFACE_STYLE_USAGE ( .BOTH. , #75680 ) ;
#53438 = CARTESIAN_POINT ( 'NONE',  ( -33.35986328002660883, -296.5810333359765991, -194.0554542064440966 ) ) ;
#53439 = CARTESIAN_POINT ( 'NONE',  ( -14.11340134904579102, -292.9947589978014548, -342.7104106392622498 ) ) ;
#53440 = AXIS2_PLACEMENT_3D ( 'NONE', #68934, #25361, #18262 ) ;
#53441 = CARTESIAN_POINT ( 'NONE',  ( -68.06359474647744889, -293.0659521925886111, -203.4776955545930548 ) ) ;
#53442 = DIRECTION ( 'NONE',  ( -0.000000000000000000, 1.000000000000000000, -0.000000000000000000 ) ) ;
#53443 = CARTESIAN_POINT ( 'NONE',  ( -9.675873773131842270, -293.2257645659203149, -202.5783187618469583 ) ) ;
#53444 = CARTESIAN_POINT ( 'NONE',  ( 194.7272697301369533, 20.94006893973816119, 14.00764870559285136 ) ) ;
#53445 = AXIS2_PLACEMENT_3D ( 'NONE', #37817, #45377, #9403 ) ;
#53447 = CARTESIAN_POINT ( 'NONE',  ( -0.7579505484019695150, -294.5520338759256447, -333.5902389464289399 ) ) ;
#53446 = CARTESIAN_POINT ( 'NONE',  ( -52.60954260745525346, -281.2667711915983091, -344.2067243930109726 ) ) ;
#53448 = CIRCLE ( 'NONE', #12643, 2.500000000000008882 ) ;
#53449 = CARTESIAN_POINT ( 'NONE',  ( -21.72598844115062633, -282.8572997399541578, -345.7610486755697252 ) ) ;
#53450 = CARTESIAN_POINT ( 'NONE',  ( -5.572117537188898240, -282.3869056221775509, -201.8045149171525452 ) ) ;
#53451 = CARTESIAN_POINT ( 'NONE',  ( -83.25986362943622510, -285.1093267773922548, -208.5106178740870462 ) ) ;
#53452 = CARTESIAN_POINT ( 'NONE',  ( -67.27458302244387767, -289.6585701290007933, -201.7750337473001139 ) ) ;
#53453 = CARTESIAN_POINT ( 'NONE',  ( 38.58615182004371036, -280.1342948216435502, -278.4643160311609904 ) ) ;
#53454 = AXIS2_PLACEMENT_3D ( 'NONE', #91144, #84523, #18749 ) ;
#53455 = CARTESIAN_POINT ( 'NONE',  ( -4.358323734616576850, -285.1811774292669952, -204.6850922109212547 ) ) ;
#53456 = CARTESIAN_POINT ( 'NONE',  ( -41.75656071397668256, -288.0268498034554909, -346.9379959245354712 ) ) ;
#53457 = CARTESIAN_POINT ( 'NONE',  ( 207.4428545773736801, 30.38304882718446009, 15.03172026577670550 ) ) ;
#53458 = CARTESIAN_POINT ( 'NONE',  ( -3.956730053986134532, -296.2044205038557720, -336.1923221123482790 ) ) ;
#53459 = CARTESIAN_POINT ( 'NONE',  ( -48.39070713424904824, -278.6152822394276996, -346.0223078551192657 ) ) ;
#53461 = CARTESIAN_POINT ( 'NONE',  ( -103.3871612008927912, -278.6410144359227843, -239.0961044356974412 ) ) ;
#53460 = CARTESIAN_POINT ( 'NONE',  ( -71.35468269079774473, -293.5191821523822000, -337.6033950387694631 ) ) ;
#53462 = CARTESIAN_POINT ( 'NONE',  ( 21.30906725888254272, -293.0459835401329656, -220.4502198836788125 ) ) ;
#53463 = AXIS2_PLACEMENT_3D ( 'NONE', #56010, #48895, #70695 ) ;
#53464 = CARTESIAN_POINT ( 'NONE',  ( -77.73168701141460701, -283.5941221504516534, -206.5021862943189603 ) ) ;
#53465 = CARTESIAN_POINT ( 'NONE',  ( -89.90860393547966112, -279.7940334242371705, -323.9288789606204659 ) ) ;
#53466 = CARTESIAN_POINT ( 'NONE',  ( -67.40271682585334645, -294.5151116790838159, -337.1561821627719269 ) ) ;
#53467 = CARTESIAN_POINT ( 'NONE',  ( 50.67999509495882648, -297.1537971777466396, -195.3911227890569364 ) ) ;
#53468 = ORIENTED_EDGE ( 'NONE', *, *, #4411, .T. ) ;
#53469 = DIRECTION ( 'NONE',  ( 0.000000000000000000, 0.000000000000000000, 1.000000000000000000 ) ) ;
#53470 = AXIS2_PLACEMENT_3D ( 'NONE', #30169, #7011, #57667 ) ;
#53471 = CARTESIAN_POINT ( 'NONE',  ( 36.10835579765513614, -283.7045761038604610, -283.7346042300444537 ) ) ;
#53472 = CARTESIAN_POINT ( 'NONE',  ( 34.96954119037157227, -292.9221476709713556, -259.9173245781427113 ) ) ;
#53473 = FACE_OUTER_BOUND ( 'NONE', #42546, .T. ) ;
#53474 = CARTESIAN_POINT ( 'NONE',  ( 90.38368222445549804, -297.2649936051623740, -200.4191791630918829 ) ) ;
#53475 = CARTESIAN_POINT ( 'NONE',  ( -109.9459350855805582, -272.0671327394398986, -245.2059219683897595 ) ) ;
#53476 = EDGE_CURVE ( 'NONE', #73850, #60939, #46872, .T. ) ;
#53477 = EDGE_CURVE ( 'NONE', #16833, #75053, #33306, .T. ) ;
#53478 = CARTESIAN_POINT ( 'NONE',  ( -2.013457625617498525, -289.9093712104926794, -338.2228417725291933 ) ) ;
#53479 = CARTESIAN_POINT ( 'NONE',  ( -86.73094157181898822, -289.5950122741907649, -324.1856509083503397 ) ) ;
#53480 = CARTESIAN_POINT ( 'NONE',  ( -85.95594508165648051, -280.8839895215666047, -214.9773393255055680 ) ) ;
#53481 = CARTESIAN_POINT ( 'NONE',  ( -82.58097277338399067, -299.1849767516310976, -211.7181474457664763 ) ) ;
#53482 = VECTOR ( 'NONE', #52423, 1000.000000000000000 ) ;
#53483 = CARTESIAN_POINT ( 'NONE',  ( -89.74639259215807385, -278.0876277746680785, -218.8996260977656618 ) ) ;
#53484 = EDGE_LOOP ( 'NONE', ( #78562, #81321, #41270, #84370 ) ) ;
#53485 = CARTESIAN_POINT ( 'NONE',  ( -87.44527960819715418, -297.0423475492891043, -211.8496367412311372 ) ) ;
#53486 = CARTESIAN_POINT ( 'NONE',  ( -38.95278486730700962, -293.9519368886932398, -195.9385501220022263 ) ) ;
#53487 = CARTESIAN_POINT ( 'NONE',  ( 33.71294247884864603, -295.5046525977163583, -297.8870726060117704 ) ) ;
#53488 = CARTESIAN_POINT ( 'NONE',  ( 185.4166944662902665, 214.7015631973135044, 22.87680765314684095 ) ) ;
#53489 = CARTESIAN_POINT ( 'NONE',  ( -110.2235594616041112, -291.1207647228275732, -276.6469173351887321 ) ) ;
#53490 = DIRECTION ( 'NONE',  ( 0.8660254037844405950, -0.4999999999999966693, 0.000000000000000000 ) ) ;
#53491 = ORIENTED_EDGE ( 'NONE', *, *, #37667, .F. ) ;
#53492 = CARTESIAN_POINT ( 'NONE',  ( 36.85714900344527933, -291.4961551925204617, -254.9730681394802900 ) ) ;
#53493 = CARTESIAN_POINT ( 'NONE',  ( -96.11481449953545564, -296.8262765204489142, -227.0063217345130511 ) ) ;
#53494 = DIRECTION ( 'NONE',  ( 0.000000000000000000, 1.000000000000000000, 0.000000000000000000 ) ) ;
#53495 = DIRECTION ( 'NONE',  ( 0.000000000000000000, 1.000000000000000000, 0.000000000000000000 ) ) ;
#53496 = CARTESIAN_POINT ( 'NONE',  ( -110.5722806347883989, -292.3437203761134811, -248.9137444395219916 ) ) ;
#53497 = CARTESIAN_POINT ( 'NONE',  ( -55.56934967048406548, -285.7662352645559736, -350.3683826091709648 ) ) ;
#53498 = CARTESIAN_POINT ( 'NONE',  ( 20.92705608575735710, -288.9044396565371358, -223.3857331067162875 ) ) ;
#53499 = CARTESIAN_POINT ( 'NONE',  ( 14.79167515850976677, -272.7886193602478215, -216.6755556202300852 ) ) ;
#53500 = CARTESIAN_POINT ( 'NONE',  ( 34.99148296292155891, -277.7004603218841225, -287.9996778581713102 ) ) ;
#53501 = CARTESIAN_POINT ( 'NONE',  ( -68.37974481075222855, -289.7210671076290964, -202.6865360694132505 ) ) ;
#53502 = CARTESIAN_POINT ( 'NONE',  ( -9.340007922585357392, -282.2747235136142194, -199.9607577945520802 ) ) ;
#53503 = ORIENTED_EDGE ( 'NONE', *, *, #56386, .F. ) ;
#53504 = CARTESIAN_POINT ( 'NONE',  ( 22.66370920053164895, -281.4818807707252972, -312.1132858258388296 ) ) ;
#53505 = CARTESIAN_POINT ( 'NONE',  ( -113.9226030530051759, -279.5802657903545878, -274.4669450821897385 ) ) ;
#53506 = CARTESIAN_POINT ( 'NONE',  ( -8.993714353747773060, -279.2097266652032204, -199.1965170824571487 ) ) ;
#53507 = CARTESIAN_POINT ( 'NONE',  ( -83.89489645444281507, -218.2138212151350274, -349.1709152291787177 ) ) ;
#53508 = CARTESIAN_POINT ( 'NONE',  ( 24.28379887806177351, -275.8829143854081281, -224.5886580769461318 ) ) ;
#53509 = APPLICATION_PROTOCOL_DEFINITION ( 'draft international standard', 'automotive_design', 1998, #62598 ) ;
#53510 = CARTESIAN_POINT ( 'NONE',  ( -13.29945240308443921, -275.8789925598883883, -197.9409683283515164 ) ) ;
#53511 = CARTESIAN_POINT ( 'NONE',  ( 30.91033621190086578, -278.2662352645559167, -285.9065529553535612 ) ) ;
#53512 = ORIENTED_EDGE ( 'NONE', *, *, #48813, .T. ) ;
#53513 = EDGE_LOOP ( 'NONE', ( #18409, #4163 ) ) ;
#53514 = EDGE_CURVE ( 'NONE', #70776, #87978, #63875, .T. ) ;
#53515 = AXIS2_PLACEMENT_3D ( 'NONE', #92187, #12683, #34909 ) ;
#53516 = CARTESIAN_POINT ( 'NONE',  ( -71.30380130000267513, -290.5912667105385481, -335.3429969690661778 ) ) ;
#53517 = CARTESIAN_POINT ( 'NONE',  ( -73.91959465289349396, -291.2911794191204535, -336.9795121209891704 ) ) ;
#53518 = CARTESIAN_POINT ( 'NONE',  ( -69.05432617537894657, -290.9723524827647338, -204.4822673447438603 ) ) ;
#53519 = CARTESIAN_POINT ( 'NONE',  ( -54.94443600254491145, -285.3393235402896266, -195.4633837525568083 ) ) ;
#53520 = CARTESIAN_POINT ( 'NONE',  ( 150.7108941768076704, 21.00000000000001066, -5.100416763304296275 ) ) ;
#53521 = CARTESIAN_POINT ( 'NONE',  ( -0.8742267934148434394, -280.9591169538946360, -334.5215715681413258 ) ) ;
#53522 = CARTESIAN_POINT ( 'NONE',  ( 35.98294356602544752, -289.5639908884725173, -282.0337551559471763 ) ) ;
#53523 = CARTESIAN_POINT ( 'NONE',  ( -93.96713309904129119, -282.3691525895853829, -317.5232648284304560 ) ) ;
#53524 = CARTESIAN_POINT ( 'NONE',  ( 28.21375808265830187, -282.4179217206897192, -237.0259640415451656 ) ) ;
#53525 = CARTESIAN_POINT ( 'NONE',  ( 34.85528321835723631, -288.8255783650404283, -296.6006222123673979 ) ) ;
#53526 = AXIS2_PLACEMENT_3D ( 'NONE', #43092, #20846, #7116 ) ;
#53527 = CARTESIAN_POINT ( 'NONE',  ( -108.5448247499395364, -278.8279534006231302, -286.7904078305830353 ) ) ;
#53528 = CARTESIAN_POINT ( 'NONE',  ( 35.91178520937113205, -292.0643128753050064, -247.9571985800041318 ) ) ;
#53529 = CARTESIAN_POINT ( 'NONE',  ( 26.99695284087917102, -287.8019280925874455, -228.3528264855224847 ) ) ;
#53530 = CARTESIAN_POINT ( 'NONE',  ( -30.89526345505026583, -286.6238772477501584, -193.6799112136753820 ) ) ;
#53531 = CARTESIAN_POINT ( 'NONE',  ( -92.55773708211756912, -284.0382644706018027, -318.1314672899030143 ) ) ;
#53532 = ORIENTED_EDGE ( 'NONE', *, *, #20809, .T. ) ;
#53533 = DIRECTION ( 'NONE',  ( 0.000000000000000000, 0.000000000000000000, 1.000000000000000000 ) ) ;
#53534 = CARTESIAN_POINT ( 'NONE',  ( -39.20544239675091802, -293.8894398156688226, -194.6064151012685954 ) ) ;
#53535 = CIRCLE ( 'NONE', #24811, 11.60392986742922439 ) ;
#53536 = CARTESIAN_POINT ( 'NONE',  ( -2.208946272988375537, -293.2817535578410570, -338.3242541719755536 ) ) ;
#53537 = AXIS2_PLACEMENT_3D ( 'NONE', #65653, #52792, #23468 ) ;
#53538 = CARTESIAN_POINT ( 'NONE',  ( -4.972844100947378720, -275.6739725832372869, -336.0687780714280848 ) ) ;
#53539 = CARTESIAN_POINT ( 'NONE',  ( -36.17796258691097222, -297.4149543911442493, -193.4631747941452602 ) ) ;
#53540 = CARTESIAN_POINT ( 'NONE',  ( -103.0187801208346912, -289.4830747739144954, -236.8232416528182114 ) ) ;
#53541 = CARTESIAN_POINT ( 'NONE',  ( -31.54504799889173228, -293.2179654760569747, -344.1979205509059625 ) ) ;
#53542 = CARTESIAN_POINT ( 'NONE',  ( -64.23129220876163004, -292.8984199429332875, -202.0534374675834499 ) ) ;
#53543 = CARTESIAN_POINT ( 'NONE',  ( 0.05496061932472129374, -293.6423373684970670, -207.3078402041178947 ) ) ;
#53544 = DIRECTION ( 'NONE',  ( -0.000000000000000000, -0.000000000000000000, -1.000000000000000000 ) ) ;
#53545 = AXIS2_PLACEMENT_3D ( 'NONE', #1947, #89032, #9499 ) ;
#53546 = CARTESIAN_POINT ( 'NONE',  ( -66.24363585937848597, -293.4294178778324067, -339.7630703501282596 ) ) ;
#53547 = CARTESIAN_POINT ( 'NONE',  ( -110.7090265421391848, -298.7529277821208780, -254.7365277776543167 ) ) ;
#53548 = CARTESIAN_POINT ( 'NONE',  ( 8.135397859867781634, -289.3536494916072570, -327.7653164872236857 ) ) ;
#53549 = CARTESIAN_POINT ( 'NONE',  ( 35.65191476376229929, -277.7713883502986505, -289.0784626392904784 ) ) ;
#53550 = CARTESIAN_POINT ( 'NONE',  ( -38.55414350765858700, -275.8619687045352293, -346.9544512512505889 ) ) ;
#53551 = AXIS2_PLACEMENT_3D ( 'NONE', #83866, #47400, #91894 ) ;
#53552 = CARTESIAN_POINT ( 'NONE',  ( -15.79795347058474775, -273.6721948758317922, -196.4872904889921017 ) ) ;
#53553 = CARTESIAN_POINT ( 'NONE',  ( 31.35970305550844017, -279.2549865558309534, -241.7004934963151470 ) ) ;
#53554 = CARTESIAN_POINT ( 'NONE',  ( -69.97707815762707639, -275.8746695921522019, -339.2330318381748384 ) ) ;
#53555 = CARTESIAN_POINT ( 'NONE',  ( -108.9538164803419704, -295.4534563665711175, -253.8399717972104099 ) ) ;
#53556 = CARTESIAN_POINT ( 'NONE',  ( 165.2494399300530290, 8.542400036368780647, 13.00000000000000178 ) ) ;
#53557 = CARTESIAN_POINT ( 'NONE',  ( 9.047129706206952449, -299.4503132403827976, -197.1931170228812391 ) ) ;
#53558 = CARTESIAN_POINT ( 'NONE',  ( 157.4851178187871312, 69.18068689461284748, 10.00000000000000000 ) ) ;
#53560 = CARTESIAN_POINT ( 'NONE',  ( -8.968870243490044913, -274.2670615027375902, -203.0466486310713208 ) ) ;
#53559 = CARTESIAN_POINT ( 'NONE',  ( 21.11292379528279994, -286.2244386629721475, -317.9362664230023370 ) ) ;
#53561 = CARTESIAN_POINT ( 'NONE',  ( 34.04233153705654047, -287.9202441031945909, -299.3704214840180953 ) ) ;
#53562 = CARTESIAN_POINT ( 'NONE',  ( -36.58718554504064713, -300.0414395763572770, -195.0056563871800961 ) ) ;
#53563 = CARTESIAN_POINT ( 'NONE',  ( -105.3749723034196961, -294.9635199266085124, -239.0675551975072892 ) ) ;
#53564 = CARTESIAN_POINT ( 'NONE',  ( -70.40991195299049821, -282.6741159565261228, -339.7344152150485570 ) ) ;
#53565 = CARTESIAN_POINT ( 'NONE',  ( -47.57981157014602758, -281.1820066073696580, -344.7108298921560845 ) ) ;
#53566 = FACE_OUTER_BOUND ( 'NONE', #67944, .T. ) ;
#53567 = CARTESIAN_POINT ( 'NONE',  ( -110.5198391537857106, -289.2645747620837255, -276.6487320007701101 ) ) ;
#53568 = CARTESIAN_POINT ( 'NONE',  ( -53.98933082536719041, -281.4075750347531084, -342.7585545661566471 ) ) ;
#53569 = CARTESIAN_POINT ( 'NONE',  ( 185.4166944662832179, 215.0000000000000568, 23.37680765314684095 ) ) ;
#53570 = DIRECTION ( 'NONE',  ( 0.000000000000000000, 1.000000000000000000, 0.000000000000000000 ) ) ;
#53571 = CARTESIAN_POINT ( 'NONE',  ( -82.92494501057666412, -289.4288575006773385, -210.7373074863700424 ) ) ;
#53572 = CARTESIAN_POINT ( 'NONE',  ( -85.78032882165403805, -274.8875901406511275, -214.7556516067056123 ) ) ;
#53573 = CARTESIAN_POINT ( 'NONE',  ( -35.89124574053997208, -284.2394436499364474, -346.9633628334771629 ) ) ;
#53575 = CARTESIAN_POINT ( 'NONE',  ( -42.93291624435025966, -283.1245427785490847, -343.1967683786787688 ) ) ;
#53574 = CARTESIAN_POINT ( 'NONE',  ( -87.06992988784264753, -271.4462442710271830, -213.4020553476225075 ) ) ;
#53576 = CARTESIAN_POINT ( 'NONE',  ( 28.56624908000236474, -277.4190832319022775, -303.2100869034903781 ) ) ;
#53577 = CARTESIAN_POINT ( 'NONE',  ( 13.85160733464844895, -277.1148272192308468, -322.6987577167236623 ) ) ;
#53578 = CARTESIAN_POINT ( 'NONE',  ( 20.09522755024080709, -284.2189616304831361, -318.5897400956937986 ) ) ;
#53579 = ORIENTED_EDGE ( 'NONE', *, *, #55666, .T. ) ;
#53580 = CIRCLE ( 'NONE', #32369, 0.4999999999999998890 ) ;
#53581 = DIRECTION ( 'NONE',  ( -1.000000000000000000, 0.000000000000000000, 0.000000000000000000 ) ) ;
#53582 = CARTESIAN_POINT ( 'NONE',  ( 39.71162213157823118, -293.3848591304944762, -270.3120772472653357 ) ) ;
#53583 = CARTESIAN_POINT ( 'NONE',  ( 26.34113441162241287, -289.0073260160251607, -231.4208639232660403 ) ) ;
#53584 = CYLINDRICAL_SURFACE ( 'NONE', #20103, 2.000000000000000000 ) ;
#53585 = CARTESIAN_POINT ( 'NONE',  ( -2.602324593224659921, -283.9809262143061233, -198.2974183793908196 ) ) ;
#53586 = CARTESIAN_POINT ( 'NONE',  ( -75.26541960986445190, -276.7415813065929342, -337.1888840775224594 ) ) ;
#53587 = ADVANCED_FACE ( 'NONE', ( #21222 ), #72658, .T. ) ;
#53588 = CARTESIAN_POINT ( 'NONE',  ( -47.61515047640244092, -290.3236410794101516, -194.8036015930892120 ) ) ;
#53589 = CIRCLE ( 'NONE', #91354, 2.939656322713313230 ) ;
#53590 = CARTESIAN_POINT ( 'NONE',  ( -75.09174444536915871, -287.0593998682140864, -207.0709773090904378 ) ) ;
#53591 = CARTESIAN_POINT ( 'NONE',  ( 1.420975651464791989, -278.2871051671716032, -333.4723521498562491 ) ) ;
#53592 = CARTESIAN_POINT ( 'NONE',  ( -0.01998350143177623009, -287.9639790831113260, -203.6701362938990769 ) ) ;
#53593 = CARTESIAN_POINT ( 'NONE',  ( 31.15105857745839302, -283.9542864903835380, -301.0459345715297559 ) ) ;
#53594 = CARTESIAN_POINT ( 'NONE',  ( 34.18504415190763268, -276.0821638689352540, -299.0167176371553523 ) ) ;
#53595 = CARTESIAN_POINT ( 'NONE',  ( -99.65101279177115146, -277.7850142952611350, -315.6223448987266806 ) ) ;
#53596 = CARTESIAN_POINT ( 'NONE',  ( -66.15218053224842265, -299.5922466657734731, -201.7224232228427070 ) ) ;
#53597 = AXIS2_PLACEMENT_3D ( 'NONE', #33716, #62628, #92396 ) ;
#53598 = CARTESIAN_POINT ( 'NONE',  ( 156.3938767642113703, 16.40718364543451813, 10.09124105457537368 ) ) ;
#53599 = CARTESIAN_POINT ( 'NONE',  ( 31.95455697924148097, -283.6233781216988064, -236.9535640164627637 ) ) ;
#53600 = CARTESIAN_POINT ( 'NONE',  ( -45.96538147938693442, -296.0834832649001100, -195.0886954144488925 ) ) ;
#53601 = CARTESIAN_POINT ( 'NONE',  ( -35.09237171215954731, -55.96374926131388605, 21.50000000000000000 ) ) ;
#53602 = B_SPLINE_CURVE_WITH_KNOTS ( 'NONE', 3,
 ( #26672, #90111, #32835, #91983 ),
 .UNSPECIFIED., .F., .F.,
 ( 4, 4 ),
 ( 0.000000000000000000, 0.0008009674008372812039 ),
 .UNSPECIFIED. ) ;
#53603 = CARTESIAN_POINT ( 'NONE',  ( -96.14626180808231481, -277.4523749078908281, -313.7411953049549425 ) ) ;
#53604 = CARTESIAN_POINT ( 'NONE',  ( -92.89483106924163280, -274.4819131641421563, -217.5986463183466242 ) ) ;
#53605 = CARTESIAN_POINT ( 'NONE',  ( 22.69880531111737909, -279.9683447281902886, -222.5076124784726233 ) ) ;
#53606 = CARTESIAN_POINT ( 'NONE',  ( 11.79022208728040866, -288.5053483433746919, -214.9386120569807588 ) ) ;
#53607 = CARTESIAN_POINT ( 'NONE',  ( -53.12674506964882681, -296.7709695311993983, -345.0713127741260564 ) ) ;
#53608 = CARTESIAN_POINT ( 'NONE',  ( -105.5968944431117791, -297.3057655846544662, -305.2520074802090448 ) ) ;
#53609 = CARTESIAN_POINT ( 'NONE',  ( -44.50032219989088134, -293.9616707823158777, -195.8188722004524891 ) ) ;
#53610 = CARTESIAN_POINT ( 'NONE',  ( 36.85386958613226227, -279.4215622442948757, -260.2257207562183225 ) ) ;
#53611 = CARTESIAN_POINT ( 'NONE',  ( 14.31715667453972252, -282.7047712181081351, -216.6919510423215058 ) ) ;
#53612 = CARTESIAN_POINT ( 'NONE',  ( -37.12127030869519473, -296.1347879267162284, -195.9182775452011072 ) ) ;
#53613 = CARTESIAN_POINT ( 'NONE',  ( -91.84712396182010252, -285.4140936960852741, -323.6114624651132772 ) ) ;
#53614 = AXIS2_PLACEMENT_3D ( 'NONE', #79126, #14273, #72038 ) ;
#53615 = CARTESIAN_POINT ( 'NONE',  ( 27.29655540154662319, -286.9432364762299130, -305.0541176609947911 ) ) ;
#53616 = CARTESIAN_POINT ( 'NONE',  ( 19.09100179000933650, -280.1882620950287901, -218.1245126101040341 ) ) ;
#53617 = CARTESIAN_POINT ( 'NONE',  ( -88.39795797536243072, -231.3176004196124893, -347.5402749026013680 ) ) ;
#53618 = ORIENTED_EDGE ( 'NONE', *, *, #93562, .F. ) ;
#53619 = CARTESIAN_POINT ( 'NONE',  ( 20.35997111928813652, -286.5887492913134338, -225.6106473467234821 ) ) ;
#53620 = EDGE_LOOP ( 'NONE', ( #58766, #11807, #38881, #2051 ) ) ;
#53621 = CARTESIAN_POINT ( 'NONE',  ( -74.11562602863301663, -284.6083464732569723, -337.7194813484299516 ) ) ;
#53622 = CARTESIAN_POINT ( 'NONE',  ( 5.185615645001697693, -274.9781837824386912, -210.9394231862558229 ) ) ;
#53623 = CARTESIAN_POINT ( 'NONE',  ( 25.22968011714511150, -285.7590275954245840, -226.1476479710968022 ) ) ;
#53624 = CARTESIAN_POINT ( 'NONE',  ( -56.09981911720402081, -290.7364901304574119, -195.9449417016573989 ) ) ;
#53625 = CARTESIAN_POINT ( 'NONE',  ( 21.78179697170708451, -281.8331784073755557, -221.3995789486758383 ) ) ;
#53626 = CARTESIAN_POINT ( 'NONE',  ( 222.8344101925596306, -44.55766379199612004, 21.50000000000000000 ) ) ;
#53627 = CARTESIAN_POINT ( 'NONE',  ( -33.96549430379967305, -281.6140185880648232, -194.1291759367820475 ) ) ;
#53628 = CARTESIAN_POINT ( 'NONE',  ( 36.57822742821990403, -281.6153989051564963, -248.8292581370362768 ) ) ;
#53629 = CARTESIAN_POINT ( 'NONE',  ( -82.08285599513421005, -288.9094976428775681, -214.2051214447836571 ) ) ;
#53630 = CARTESIAN_POINT ( 'NONE',  ( -21.48569620681853465, -108.6157210391733514, -362.8212015391057434 ) ) ;
#53631 = ORIENTED_EDGE ( 'NONE', *, *, #66872, .F. ) ;
#53632 = CARTESIAN_POINT ( 'NONE',  ( -7.996861572670578511, -278.6670339975016759, -339.2147363236462638 ) ) ;
#53633 = CARTESIAN_POINT ( 'NONE',  ( 184.4162654869148525, 263.6987771649366437, -153.0423760906433870 ) ) ;
#53634 = CARTESIAN_POINT ( 'NONE',  ( 23.12995493623812138, -280.1712441473311515, -314.1440003197535020 ) ) ;
#53635 = CARTESIAN_POINT ( 'NONE',  ( -98.52834922945847040, -296.4554326089141796, -230.2684471384125970 ) ) ;
#53636 = CARTESIAN_POINT ( 'NONE',  ( -16.63714383042016820, -291.8203596798856552, -196.2608598751364184 ) ) ;
#53637 = CARTESIAN_POINT ( 'NONE',  ( -109.4300717440919186, -269.0112169713418098, -295.3470023912256579 ) ) ;
#53639 = CARTESIAN_POINT ( 'NONE',  ( 33.04264522483112643, -285.6605388598512718, -248.1267844340309807 ) ) ;
#53638 = CARTESIAN_POINT ( 'NONE',  ( -33.35434752022145943, -296.6758848936784716, -193.9512867474840334 ) ) ;
#53640 = CARTESIAN_POINT ( 'NONE',  ( 17.08052670803324702, -296.1261134211091530, -320.8495989157309509 ) ) ;
#53641 = CARTESIAN_POINT ( 'NONE',  ( -69.00245828154172045, -286.9420105298405588, -204.0234830594493474 ) ) ;
#53642 = ORIENTED_EDGE ( 'NONE', *, *, #32523, .T. ) ;
#53643 = CARTESIAN_POINT ( 'NONE',  ( -4.715066979952252879, -293.4127470249062526, -200.8749825059219063 ) ) ;
#53644 = CARTESIAN_POINT ( 'NONE',  ( -103.0652842761183763, -284.6114456443505674, -302.3896500212662204 ) ) ;
#53645 = CARTESIAN_POINT ( 'NONE',  ( -100.4149617698935231, -295.9242530994878848, -226.8665603547654541 ) ) ;
#53646 = CARTESIAN_POINT ( 'NONE',  ( -27.87913822265212005, -292.9720822856205018, -194.0539093926565499 ) ) ;
#53647 = CARTESIAN_POINT ( 'NONE',  ( -99.98459185586217757, -291.6366128526522630, -225.6912733521691052 ) ) ;
#53648 = CARTESIAN_POINT ( 'NONE',  ( -74.71407828275975760, -289.7312495634576521, -333.0839009449283594 ) ) ;
#53649 = ORIENTED_EDGE ( 'NONE', *, *, #28009, .T. ) ;
#53650 = DIRECTION ( 'NONE',  ( 1.000000000000000000, 0.000000000000000000, -0.000000000000000000 ) ) ;
#53651 = CARTESIAN_POINT ( 'NONE',  ( -35.53294294358471461, -299.9349756489463061, -194.5957445222843205 ) ) ;
#53652 = CARTESIAN_POINT ( 'NONE',  ( -94.77853345212247405, -272.0369759094540427, -219.6756279791674444 ) ) ;
#53653 = CARTESIAN_POINT ( 'NONE',  ( -26.72045869150398545, -281.9726197832043795, -342.8735899217874135 ) ) ;
#53654 = EDGE_LOOP ( 'NONE', ( #90824, #74321 ) ) ;
#53655 = EDGE_LOOP ( 'NONE', ( #78783, #74471, #52890, #48585 ) ) ;
#53656 = CARTESIAN_POINT ( 'NONE',  ( -72.81788955465673041, -277.0169313983098505, -338.6470847179453472 ) ) ;
#53657 = CARTESIAN_POINT ( 'NONE',  ( -96.91522037678048207, -271.5564133648870211, -226.7166739224035723 ) ) ;
#53658 = CARTESIAN_POINT ( 'NONE',  ( -79.78008251369473669, -281.3319343954994451, -209.4525867362486338 ) ) ;
#53659 = CARTESIAN_POINT ( 'NONE',  ( -40.58301655547638376, -275.2328944556943497, -344.5382005577882296 ) ) ;
#53660 = CARTESIAN_POINT ( 'NONE',  ( -110.6095666347328859, -297.8143495713083553, -266.0079304797559985 ) ) ;
#53661 = CARTESIAN_POINT ( 'NONE',  ( -73.00925116881927579, -298.6472176279314681, -206.3138551465477804 ) ) ;
#53662 = CARTESIAN_POINT ( 'NONE',  ( -93.09151525179012765, -298.8684963103057726, -218.3380175319154830 ) ) ;
#53663 = CARTESIAN_POINT ( 'NONE',  ( -66.86743861542525735, -271.6872685160179799, -201.0311996820545630 ) ) ;
#53664 = CARTESIAN_POINT ( 'NONE',  ( 22.66687361824671143, -293.6222339179165601, -228.5914461338662136 ) ) ;
#53665 = CARTESIAN_POINT ( 'NONE',  ( -49.77052455606787618, -290.4653785447424639, -197.7773230103978221 ) ) ;
#53666 = DIRECTION ( 'NONE',  ( -0.7806247497998081153, 0.000000000000000000, 0.6249999999999895639 ) ) ;
#53667 = CARTESIAN_POINT ( 'NONE',  ( 38.66583559413955129, -275.8940849991554387, -258.3438715168978206 ) ) ;
#53668 = CARTESIAN_POINT ( 'NONE',  ( -83.19223263293157800, -273.5702973329051702, -213.5568164420559754 ) ) ;
#53669 = CARTESIAN_POINT ( 'NONE',  ( 27.87580258256984322, -280.7641343703041343, -310.4611761175884794 ) ) ;
#53670 = CARTESIAN_POINT ( 'NONE',  ( 175.2296996224750103, 154.6894116713782807, 0.000000000000000000 ) ) ;
#53671 = EDGE_CURVE ( 'NONE', #64817, #23459, #42358, .T. ) ;
#53672 = CARTESIAN_POINT ( 'NONE',  ( -110.5520817729917837, -283.7422173350662433, -270.9003088089290259 ) ) ;
#53673 = AXIS2_PLACEMENT_3D ( 'NONE', #89415, #10822, #67222 ) ;
#53674 = CARTESIAN_POINT ( 'NONE',  ( -58.00775052530494236, -281.3182150687318881, -342.6852303894619354 ) ) ;
#53675 = CARTESIAN_POINT ( 'NONE',  ( 35.42702256844754061, -273.9823608123143117, -259.3177322871711681 ) ) ;
#53676 = CARTESIAN_POINT ( 'NONE',  ( -48.54107235922690933, -281.9098679950072892, -196.1503743120290721 ) ) ;
#53677 = CARTESIAN_POINT ( 'NONE',  ( 210.6908326509675362, 1.000000000000000000, 7.166337341072457789 ) ) ;
#53678 = DIRECTION ( 'NONE',  ( -0.000000000000000000, -1.000000000000000000, -0.000000000000000000 ) ) ;
#53679 = CARTESIAN_POINT ( 'NONE',  ( -2.900705312295462690, -272.8994809571926226, -202.3740844392764302 ) ) ;
#53680 = AXIS2_PLACEMENT_3D ( 'NONE', #79609, #45442, #9467 ) ;
#53681 = CARTESIAN_POINT ( 'NONE',  ( -112.3821156058396724, -280.6081071499053223, -266.0062966425177819 ) ) ;
#53682 = CARTESIAN_POINT ( 'NONE',  ( 189.4188515237862589, 293.9636489450775798, 9.103929867429222611 ) ) ;
#53683 = CARTESIAN_POINT ( 'NONE',  ( -91.38637037264089713, -285.7340677702808875, -323.1672522424606200 ) ) ;
#53684 = ORIENTED_EDGE ( 'NONE', *, *, #62476, .T. ) ;
#53685 = LINE ( 'NONE', #76398, #9294 ) ;
#53686 = CARTESIAN_POINT ( 'NONE',  ( -104.3669543607152406, -288.9978052692231927, -236.5926037552136165 ) ) ;
#53687 = VECTOR ( 'NONE', #31628, 1000.000000000000000 ) ;
#53688 = DIRECTION ( 'NONE',  ( -0.000000000000000000, -0.9681751575201845705, 0.2502735790305594676 ) ) ;
#53689 = CARTESIAN_POINT ( 'NONE',  ( -109.7571711225060085, -295.1901049508429651, -282.3248158213936563 ) ) ;
#53690 = CARTESIAN_POINT ( 'NONE',  ( 6.556285905353787413, -286.5883643556964557, -330.2902834661385896 ) ) ;
#53691 = CARTESIAN_POINT ( 'NONE',  ( 157.0521749816625743, 17.25638377770970777, -7.577257116167048778 ) ) ;
#53692 = CARTESIAN_POINT ( 'NONE',  ( -105.5265176478331028, -294.9635199286505554, -238.9979103698759388 ) ) ;
#53693 = CARTESIAN_POINT ( 'NONE',  ( 23.32212481994681141, -285.4090837977557840, -224.0513729359206820 ) ) ;
#53694 = CARTESIAN_POINT ( 'NONE',  ( 35.11584125794944811, -282.9685739567360656, -256.2823163011307770 ) ) ;
#53695 = CARTESIAN_POINT ( 'NONE',  ( -49.94776518472127691, -281.4505837710136689, -345.3479975934111508 ) ) ;
#53696 = CARTESIAN_POINT ( 'NONE',  ( -15.85164981939449547, -288.7664298321241176, -340.1791045327702818 ) ) ;
#53697 = CARTESIAN_POINT ( 'NONE',  ( 34.64616932668712934, -282.5277066901281842, -283.4831276537292410 ) ) ;
#53698 = EDGE_CURVE ( 'NONE', #24267, #45543, #12736, .T. ) ;
#53699 = CARTESIAN_POINT ( 'NONE',  ( -0.07178170301374783846, -290.5391178371183400, -335.9132986364966769 ) ) ;
#53700 = CARTESIAN_POINT ( 'NONE',  ( -75.78174656667668785, -297.7208338461131234, -203.5813900550990354 ) ) ;
#53701 = CARTESIAN_POINT ( 'NONE',  ( -67.53564237597846898, -273.6668407948344566, -199.5280335408201040 ) ) ;
#53702 = CARTESIAN_POINT ( 'NONE',  ( -25.16507031956652085, -294.1879209930351635, -196.6635469330276180 ) ) ;
#53703 = DIRECTION ( 'NONE',  ( 0.000000000000000000, 0.000000000000000000, 1.000000000000000000 ) ) ;
#53704 = CARTESIAN_POINT ( 'NONE',  ( -114.2704648735229114, -287.0519495502703080, -270.3937649182068981 ) ) ;
#53705 = ORIENTED_EDGE ( 'NONE', *, *, #24919, .F. ) ;
#53706 = CARTESIAN_POINT ( 'NONE',  ( 20.30776064926366686, -274.2169863109052699, -318.5956295083899477 ) ) ;
#53707 = CARTESIAN_POINT ( 'NONE',  ( 197.8478357033531267, 68.18663436155952695, 11.29153850601979592 ) ) ;
#53708 = CARTESIAN_POINT ( 'NONE',  ( -112.9782036321411169, -295.0689229741468580, -261.1112665015822927 ) ) ;
#53709 = CARTESIAN_POINT ( 'NONE',  ( -109.9625467149489424, -291.9808278973164306, -283.5008690240114220 ) ) ;
#53710 = CARTESIAN_POINT ( 'NONE',  ( -34.02776938650374916, -273.4435175781427461, -197.3343384325569616 ) ) ;
#53711 = CARTESIAN_POINT ( 'NONE',  ( -110.9983512697878041, -292.0252275883647144, -273.9619563567424052 ) ) ;
#53712 = CARTESIAN_POINT ( 'NONE',  ( -57.73191080878844161, -292.7236976606802727, -199.9685503581490309 ) ) ;
#53713 = CARTESIAN_POINT ( 'NONE',  ( -53.89479585623762148, -285.0275496555290715, -342.5524618780006563 ) ) ;
#53714 = CARTESIAN_POINT ( 'NONE',  ( -97.01487597653033390, -292.6215975127229285, -222.6356700551351082 ) ) ;
#53715 = CARTESIAN_POINT ( 'NONE',  ( -76.92852493151174542, -292.8491664829326737, -204.8310765265192686 ) ) ;
#53716 = CARTESIAN_POINT ( 'NONE',  ( -0.7597893167630116462, -294.3853807310752586, -333.5913030011353158 ) ) ;
#53717 = CARTESIAN_POINT ( 'NONE',  ( 26.64409949748151618, -289.0275910412937037, -231.2354474640682440 ) ) ;
#53718 = CARTESIAN_POINT ( 'NONE',  ( 26.27941828610472541, -281.1457015852035966, -226.8935177391313971 ) ) ;
#53719 = CARTESIAN_POINT ( 'NONE',  ( -71.44638058470263786, -293.5789106112503077, -337.7865210031841343 ) ) ;
#53720 = CARTESIAN_POINT ( 'NONE',  ( -108.2279708245690983, -284.0012034924757245, -300.5663936039224495 ) ) ;
#53721 = CARTESIAN_POINT ( 'NONE',  ( 36.99424976649718388, -277.6195602777492581, -277.1444323805264958 ) ) ;
#53722 = EDGE_CURVE ( 'NONE', #90108, #9328, #43005, .T. ) ;
#53723 = CARTESIAN_POINT ( 'NONE',  ( 4.096446069770744991, -284.6098817895948514, -207.7862039460869141 ) ) ;
#53724 = CARTESIAN_POINT ( 'NONE',  ( -56.63277164091257276, -275.4376916734761949, -343.6830209935733365 ) ) ;
#53725 = CARTESIAN_POINT ( 'NONE',  ( 205.2786681169002350, 32.98517505407394168, 14.49999999999999822 ) ) ;
#53726 = CARTESIAN_POINT ( 'NONE',  ( -29.44422744186875462, -282.4572117539385090, -343.0451161892349319 ) ) ;
#53727 = CARTESIAN_POINT ( 'NONE',  ( -95.61379339938980593, -280.4315221119219927, -220.6180146963801860 ) ) ;
#53728 = CARTESIAN_POINT ( 'NONE',  ( 18.18959880444806032, -285.8832565510972472, -217.2835471050289584 ) ) ;
#53729 = CARTESIAN_POINT ( 'NONE',  ( 31.53671491733354415, -295.6712145854739902, -297.5890486515670545 ) ) ;
#53730 = CARTESIAN_POINT ( 'NONE',  ( 36.81805767896555892, -277.3742741319258016, -287.9322581230598530 ) ) ;
#53731 = CARTESIAN_POINT ( 'NONE',  ( 33.73238483501313567, -277.2304729315533223, -298.8196200745537681 ) ) ;
#53732 = CARTESIAN_POINT ( 'NONE',  ( -103.1319309202313264, -277.9561026858974628, -302.1110714914964888 ) ) ;
#53733 = CARTESIAN_POINT ( 'NONE',  ( -102.1582459998145112, -275.0293437238689762, -233.2346628275964235 ) ) ;
#53734 = CARTESIAN_POINT ( 'NONE',  ( 19.17715791613656862, -284.8699592250636101, -221.3137213729414725 ) ) ;
#53735 = CARTESIAN_POINT ( 'NONE',  ( -34.85957701735164704, -294.6884888296338545, -347.2999466483493620 ) ) ;
#53736 = CARTESIAN_POINT ( 'NONE',  ( -91.02035993566803995, -291.3987747300134288, -324.5189800521484926 ) ) ;
#53737 = CARTESIAN_POINT ( 'NONE',  ( 22.06323377204606473, -291.8738325072574185, -227.3830450239286165 ) ) ;
#53738 = VERTEX_POINT ( 'NONE', #70501 ) ;
#53739 = CARTESIAN_POINT ( 'NONE',  ( -28.09946630545501023, -291.8392725812647086, -197.8764635893611796 ) ) ;
#53740 = ORIENTED_EDGE ( 'NONE', *, *, #13993, .T. ) ;
#53741 = CARTESIAN_POINT ( 'NONE',  ( -84.96193311972864137, -290.7710090362177766, -330.5438033894057526 ) ) ;
#53742 = CARTESIAN_POINT ( 'NONE',  ( -59.77278706339543390, -280.4053062131053480, -200.7323170001139374 ) ) ;
#53743 = CARTESIAN_POINT ( 'NONE',  ( -89.38839166277168147, -296.2602100345200142, -213.9630494963244018 ) ) ;
#53744 = CARTESIAN_POINT ( 'NONE',  ( 26.26837592287659362, -287.6328268496965848, -227.1279820120310546 ) ) ;
#53745 = CARTESIAN_POINT ( 'NONE',  ( 37.69806526446761552, -287.6699898611338426, -253.1335338145305798 ) ) ;
#53746 = CARTESIAN_POINT ( 'NONE',  ( -106.5537135154276172, -285.1964224836257813, -246.9264936854656014 ) ) ;
#53747 = CARTESIAN_POINT ( 'NONE',  ( 193.7935517605804989, 279.2504548556453869, -125.8485263907484750 ) ) ;
#53748 = CARTESIAN_POINT ( 'NONE',  ( 183.4698700144519989, 263.1936897402629825, -152.3596953817753672 ) ) ;
#53749 = CARTESIAN_POINT ( 'NONE',  ( -12.93242418913286329, -92.20420405495083571, -356.2274306187722459 ) ) ;
#53750 = CARTESIAN_POINT ( 'NONE',  ( 15.70794271834726530, -275.4740003981351606, -320.7430306185804056 ) ) ;
#53751 = CARTESIAN_POINT ( 'NONE',  ( 17.65807200446980474, -275.1618888144814150, -318.8491255472634407 ) ) ;
#53752 = CARTESIAN_POINT ( 'NONE',  ( -108.0563970603190000, -272.6079619551429118, -239.8096252077025952 ) ) ;
#53753 = CARTESIAN_POINT ( 'NONE',  ( 46.50877722536523606, 10.63732441549002949, -329.0452962795232565 ) ) ;
#53754 = CARTESIAN_POINT ( 'NONE',  ( -54.04003407429214434, -275.9469056853669144, -345.0777433922604018 ) ) ;
#53755 = ORIENTED_EDGE ( 'NONE', *, *, #14909, .F. ) ;
#53756 = CARTESIAN_POINT ( 'NONE',  ( -37.26166180947142692, -289.5434718961854514, -343.4226128738837929 ) ) ;
#53757 = CARTESIAN_POINT ( 'NONE',  ( -108.7423483825970720, -297.7175025026989488, -241.8260749796072275 ) ) ;
#53758 = CARTESIAN_POINT ( 'NONE',  ( -51.79520661962206418, -298.3644645993396693, -194.7381567659673181 ) ) ;
#53759 = CARTESIAN_POINT ( 'NONE',  ( -26.20531350542740512, -295.0731009240769254, -342.5066715356343821 ) ) ;
#53760 = ORIENTED_EDGE ( 'NONE', *, *, #19908, .F. ) ;
#53761 = CARTESIAN_POINT ( 'NONE',  ( -103.6990812841965663, -279.9957073324142698, -306.4999082441668179 ) ) ;
#53762 = CARTESIAN_POINT ( 'NONE',  ( 39.55810021491750916, -281.0903305709754818, -272.7998902695285324 ) ) ;
#53763 = CARTESIAN_POINT ( 'NONE',  ( -103.6553095478218296, -280.0537396808990707, -238.9890532526910931 ) ) ;
#53764 = CARTESIAN_POINT ( 'NONE',  ( -56.64468163391967437, -279.0576661757560260, -343.9094473348219481 ) ) ;
#53765 = CARTESIAN_POINT ( 'NONE',  ( -88.52261674738612385, -295.8923777569148683, -217.4138278520737515 ) ) ;
#53766 = DIRECTION ( 'NONE',  ( -1.000000000000000000, 0.000000000000000000, 0.000000000000000000 ) ) ;
#53767 = CARTESIAN_POINT ( 'NONE',  ( -97.99479180768965136, -279.2841262416791324, -229.6486716486747355 ) ) ;
#53768 = CARTESIAN_POINT ( 'NONE',  ( -63.51172613709964310, -274.5224141247678062, -198.1164741741325486 ) ) ;
#53769 = CARTESIAN_POINT ( 'NONE',  ( 37.33987683817696990, -286.4468324700234234, -287.0329228604045397 ) ) ;
#53770 = CARTESIAN_POINT ( 'NONE',  ( -8.484289576188103865, -276.4298878468243288, -201.0799179885277681 ) ) ;
#53771 = CARTESIAN_POINT ( 'NONE',  ( 27.14175265579480367, -274.6694386990668590, -311.4532224839380774 ) ) ;
#53772 = FACE_OUTER_BOUND ( 'NONE', #39966, .T. ) ;
#53773 = CARTESIAN_POINT ( 'NONE',  ( -107.8842409054083618, -289.4913365489192074, -289.9476935304697349 ) ) ;
#53774 = CARTESIAN_POINT ( 'NONE',  ( -99.71067791559507043, -283.3025203649021933, -315.4325958904153140 ) ) ;
#53775 = CARTESIAN_POINT ( 'NONE',  ( 36.71648401343644252, -279.8048610585829579, -271.3493513211785171 ) ) ;
#53777 = CARTESIAN_POINT ( 'NONE',  ( -84.54243050674024573, -283.4765621198396843, -212.7319753606611528 ) ) ;
#53776 = CARTESIAN_POINT ( 'NONE',  ( 13.75720791185352709, -279.3598837390550216, -217.3346685025056786 ) ) ;
#53778 = CARTESIAN_POINT ( 'NONE',  ( -36.66223718241194263, -291.0438312036703792, -345.3706420096863781 ) ) ;
#53779 = CARTESIAN_POINT ( 'NONE',  ( -110.5558063710717960, -279.8251882676347009, -265.1818177385400759 ) ) ;
#53780 = CARTESIAN_POINT ( 'NONE',  ( 29.33919985515026596, -285.8906705383787994, 27.50000000000000000 ) ) ;
#53781 = CARTESIAN_POINT ( 'NONE',  ( 31.65922809037965990, -280.3717877619147885, -302.8166510391656630 ) ) ;
#53782 = CARTESIAN_POINT ( 'NONE',  ( 37.71021853838445281, -295.5513509988829242, -270.2858652379441082 ) ) ;
#53783 = CARTESIAN_POINT ( 'NONE',  ( -99.40817597146521223, -277.3798445903617562, -226.5236158756072200 ) ) ;
#53784 = CARTESIAN_POINT ( 'NONE',  ( -109.3443127197655116, -286.2743845897448978, -291.9847375159998819 ) ) ;
#53785 = CARTESIAN_POINT ( 'NONE',  ( -33.63493029267698375, -294.0186186291767285, -194.8920908453042102 ) ) ;
#53786 = CARTESIAN_POINT ( 'NONE',  ( 36.62618604559104085, -287.0111598253804459, -291.2158518810209102 ) ) ;
#53787 = CARTESIAN_POINT ( 'NONE',  ( -69.34629960582535091, -290.0237909574971695, -203.8479467414003352 ) ) ;
#53788 = CARTESIAN_POINT ( 'NONE',  ( -43.38969887572877582, -264.0939091915531662, -436.2267584252900292 ) ) ;
#53789 = CARTESIAN_POINT ( 'NONE',  ( -35.11939097372280116, -275.7084878438100759, -343.8206634563861712 ) ) ;
#53790 = CARTESIAN_POINT ( 'NONE',  ( 13.17842440672503912, -292.4769948278054699, -324.8244048322745812 ) ) ;
#53791 = CARTESIAN_POINT ( 'NONE',  ( 221.8344101925596306, 1.000000000000000222, 7.000000000000000000 ) ) ;
#53792 = DIRECTION ( 'NONE',  ( 1.000000000000000000, 0.000000000000000000, 0.000000000000000000 ) ) ;
#53793 = CARTESIAN_POINT ( 'NONE',  ( -8.752855232501968175, -290.8993879231106803, -199.6123674590418489 ) ) ;
#53794 = CARTESIAN_POINT ( 'NONE',  ( -111.0283494357677085, -286.2166081833692601, -265.4318532408312876 ) ) ;
#53795 = CARTESIAN_POINT ( 'NONE',  ( -6.064349368327516032, -286.8865769038594635, -339.6121204724365725 ) ) ;
#53796 = CARTESIAN_POINT ( 'NONE',  ( 20.79508455461865424, -288.3470181421716916, -225.2447220087632331 ) ) ;
#53797 = CARTESIAN_POINT ( 'NONE',  ( 152.9410204041312795, 20.82809642979767872, -8.928152258827880772 ) ) ;
#53798 = CARTESIAN_POINT ( 'NONE',  ( 20.46196134679606971, -287.7246791635639624, -225.5131698956544994 ) ) ;
#53799 = EDGE_CURVE ( 'NONE', #23700, #68064, #90722, .T. ) ;
#53800 = CARTESIAN_POINT ( 'NONE',  ( 25.11519868815494050, -294.9632919028105675, -228.1084572948894902 ) ) ;
#53801 = DIRECTION ( 'NONE',  ( -0.000000000000000000, 1.000000000000000000, 0.000000000000000000 ) ) ;
#53802 = CARTESIAN_POINT ( 'NONE',  ( 37.89728070803992921, -288.5763091559493887, -255.9699928602805414 ) ) ;
#53803 = CARTESIAN_POINT ( 'NONE',  ( -112.7718771662168535, -276.6884237887530844, -265.9336370287980458 ) ) ;
#53804 = CARTESIAN_POINT ( 'NONE',  ( -48.48673000920530285, -277.5234669723861884, -346.5827895998542658 ) ) ;
#53805 = CARTESIAN_POINT ( 'NONE',  ( 23.66651032813422972, -291.0289028029738461, -225.7818351594687272 ) ) ;
#53806 = CARTESIAN_POINT ( 'NONE',  ( -72.50681190168280921, -279.5997139831050617, -201.8452629067262762 ) ) ;
#53807 = CARTESIAN_POINT ( 'NONE',  ( -71.23645610329641897, -299.5823714154043955, -203.8413098687840943 ) ) ;
#53808 = CARTESIAN_POINT ( 'NONE',  ( -48.18343439336388201, -280.8035638491393229, -507.6172057986060508 ) ) ;
#53809 = CARTESIAN_POINT ( 'NONE',  ( -69.61304295716904278, -283.6272128507254706, -202.6449514173468742 ) ) ;
#53810 = FACE_OUTER_BOUND ( 'NONE', #29440, .T. ) ;
#53811 = CARTESIAN_POINT ( 'NONE',  ( -74.65427059269417498, -275.6939540864842115, -334.5377302799010977 ) ) ;
#53812 = CARTESIAN_POINT ( 'NONE',  ( 36.82107716984844359, -279.4041693617803617, -258.8484257117196989 ) ) ;
#53813 = DIRECTION ( 'NONE',  ( -0.000000000000000000, -0.000000000000000000, -1.000000000000000000 ) ) ;
#53814 = CARTESIAN_POINT ( 'NONE',  ( -5.591075499922819603, -275.1219582218917594, -339.7484769946556185 ) ) ;
#53815 = CARTESIAN_POINT ( 'NONE',  ( -108.1307173254744072, -298.3406660664528545, -249.8764213167940227 ) ) ;
#53816 = CARTESIAN_POINT ( 'NONE',  ( -34.50422900785937941, -281.9376023956479003, -346.9994978463583379 ) ) ;
#53817 = CARTESIAN_POINT ( 'NONE',  ( -109.9711776147204034, -297.6220607304188093, -260.5771500789070387 ) ) ;
#53818 = CARTESIAN_POINT ( 'NONE',  ( -80.36165112878053662, -298.7981143427669508, -207.0314493906307973 ) ) ;
#53819 = CARTESIAN_POINT ( 'NONE',  ( 2.945142243337858456, -274.2758474914076032, -209.3986512255144703 ) ) ;
#53820 = CARTESIAN_POINT ( 'NONE',  ( 24.21528019205082316, -294.9707634460075383, -227.4929773961752062 ) ) ;
#53821 = CARTESIAN_POINT ( 'NONE',  ( 35.94840406658695997, -288.0157726787018646, -293.9738398002437521 ) ) ;
#53822 = CARTESIAN_POINT ( 'NONE',  ( -111.5767603299888435, -276.8124289874544957, -256.2040983486289178 ) ) ;
#53823 = CARTESIAN_POINT ( 'NONE',  ( -113.1716504514178752, -290.5527120497221745, -256.9888093382853071 ) ) ;
#53824 = ADVANCED_FACE ( 'NONE', ( #35900 ), #26983, .T. ) ;
#53825 = EDGE_CURVE ( 'NONE', #14772, #1176, #80367, .T. ) ;
#53826 = CARTESIAN_POINT ( 'NONE',  ( 12.30653773662580619, -287.3995751320486534, -324.2673733040364823 ) ) ;
#53827 = CARTESIAN_POINT ( 'NONE',  ( -58.35332334956310518, -289.7803841320211404, -198.3645046191483630 ) ) ;
#53828 = ORIENTED_EDGE ( 'NONE', *, *, #56142, .F. ) ;
#53829 = CARTESIAN_POINT ( 'NONE',  ( 198.8657840505796628, 68.63430910526400908, 9.310452007619588244 ) ) ;
#53830 = CARTESIAN_POINT ( 'NONE',  ( 25.74602580085518966, -287.5663775226341841, -307.3111863164332931 ) ) ;
#53831 = CARTESIAN_POINT ( 'NONE',  ( 154.5625123364532101, 275.5000000000000568, -13.15740740740742787 ) ) ;
#53832 = CARTESIAN_POINT ( 'NONE',  ( -109.9981041180819687, -285.1802630859983196, -295.1374609723259823 ) ) ;
#53833 = CARTESIAN_POINT ( 'NONE',  ( -33.53899619861093129, -291.1576748410219579, -193.6906565508614904 ) ) ;
#53834 = CARTESIAN_POINT ( 'NONE',  ( 38.82084841480964599, -283.1824693470330203, -272.7499697835081065 ) ) ;
#53835 = CARTESIAN_POINT ( 'NONE',  ( 38.91880072476695318, -282.7901069841477693, -264.2264393889763596 ) ) ;
#53836 = CARTESIAN_POINT ( 'NONE',  ( -73.79863336783540717, -283.3836797457146872, -333.6634221105994129 ) ) ;
#53837 = CARTESIAN_POINT ( 'NONE',  ( -103.8498035772478119, -297.0582403171705437, -231.4530491659762106 ) ) ;
#53838 = CARTESIAN_POINT ( 'NONE',  ( -59.64111142486407857, -275.0725195057470955, -200.2794134251790581 ) ) ;
#53839 = CARTESIAN_POINT ( 'NONE',  ( -49.94211009299280590, -289.9108479331492276, -196.7350255217619122 ) ) ;
#53840 = CARTESIAN_POINT ( 'NONE',  ( 9.188972840122552554, -297.5684187788447730, -197.0607906701177399 ) ) ;
#53841 = ORIENTED_EDGE ( 'NONE', *, *, #87763, .F. ) ;
#53842 = DIRECTION ( 'NONE',  ( -0.000000000000000000, -0.000000000000000000, 1.000000000000000000 ) ) ;
#53843 = CARTESIAN_POINT ( 'NONE',  ( -81.46030306723940839, -285.5772743999670524, -330.3824123368046344 ) ) ;
#53844 = CARTESIAN_POINT ( 'NONE',  ( -44.75201475458462852, -296.2233916136306107, -346.7463458733362813 ) ) ;
#53845 = CARTESIAN_POINT ( 'NONE',  ( -102.3327996906839275, -285.6578850998902794, -236.8939752081201107 ) ) ;
#53846 = CARTESIAN_POINT ( 'NONE',  ( 36.26442877219990635, -274.8856837442878600, -292.2010015832324257 ) ) ;
#53847 = CARTESIAN_POINT ( 'NONE',  ( 1.641261442547662597, -293.2100757234092612, -204.0157188802905068 ) ) ;
#53848 = CARTESIAN_POINT ( 'NONE',  ( 37.45167714776628287, -285.8494989561767170, -282.7731150850767676 ) ) ;
#53849 = CARTESIAN_POINT ( 'NONE',  ( -40.63576438945634806, -292.3450972463186304, -193.4395950645307778 ) ) ;
#53850 = CARTESIAN_POINT ( 'NONE',  ( -109.2983355038224005, -291.0530753999199192, -257.6493587272869945 ) ) ;
#53851 = FACE_OUTER_BOUND ( 'NONE', #10517, .T. ) ;
#53852 = CARTESIAN_POINT ( 'NONE',  ( 222.8344101925596306, 0.000000000000000000, 10.00000000000000000 ) ) ;
#53853 = CARTESIAN_POINT ( 'NONE',  ( -105.0131974969233823, -260.5199095907283322, -315.5713868923170935 ) ) ;
#53854 = CARTESIAN_POINT ( 'NONE',  ( -70.78002839939547641, -287.1391802593108196, -201.7711335959585028 ) ) ;
#53855 = CARTESIAN_POINT ( 'NONE',  ( -117.3381139276884966, -270.1608578419545665, -261.3154543817420290 ) ) ;
#53856 = CARTESIAN_POINT ( 'NONE',  ( -78.56173964086521266, -282.5421560468634539, -330.9840048780154689 ) ) ;
#53857 = CARTESIAN_POINT ( 'NONE',  ( -71.56526471940529177, -277.1586416372951476, -339.3139418428858676 ) ) ;
#53858 = CARTESIAN_POINT ( 'NONE',  ( -49.46334835737528834, -281.8974109390292142, -196.5160499806509335 ) ) ;
#53859 = CARTESIAN_POINT ( 'NONE',  ( 66.72872018252358828, 46.00066320285807819, -316.9038945764073674 ) ) ;
#53860 = CARTESIAN_POINT ( 'NONE',  ( 13.27676825419560203, -280.9355929817181163, -327.6711764478134228 ) ) ;
#53861 = CARTESIAN_POINT ( 'NONE',  ( -8.842590557091856596, -284.4469001550755252, -201.3571043685095674 ) ) ;
#53862 = CARTESIAN_POINT ( 'NONE',  ( -113.1073802691691839, -274.4481303064853250, -267.5632856924480052 ) ) ;
#53863 = CARTESIAN_POINT ( 'NONE',  ( -26.19183625367893598, -295.3987156376396683, -342.5668585929998926 ) ) ;
#53864 = ORIENTED_EDGE ( 'NONE', *, *, #76674, .T. ) ;
#53865 = CARTESIAN_POINT ( 'NONE',  ( 35.69506761312781151, -292.3499711950225901, -278.9849237609527677 ) ) ;
#53866 = CARTESIAN_POINT ( 'NONE',  ( 34.09265066667622790, -276.5668189960217660, -298.9730580085625888 ) ) ;
#53867 = CARTESIAN_POINT ( 'NONE',  ( 33.83376145477104302, -275.3375332777842459, -254.0863006109598246 ) ) ;
#53868 = CARTESIAN_POINT ( 'NONE',  ( 28.24535536162866833, -273.9504234910574496, -230.5124837694347661 ) ) ;
#53869 = DIRECTION ( 'NONE',  ( 0.000000000000000000, 1.000000000000000000, 0.000000000000000000 ) ) ;
#53870 = CARTESIAN_POINT ( 'NONE',  ( -69.71002884953006173, -271.6259365963096570, -202.6914973942407698 ) ) ;
#53871 = CARTESIAN_POINT ( 'NONE',  ( 17.15414218000039526, -295.7190632345941594, -323.9976620302848005 ) ) ;
#53872 = DIRECTION ( 'NONE',  ( 0.000000000000000000, -1.000000000000000000, 0.000000000000000000 ) ) ;
#53873 = CARTESIAN_POINT ( 'NONE',  ( 200.1063562619108609, 64.94916223746493245, 5.267193185414368095 ) ) ;
#53874 = CARTESIAN_POINT ( 'NONE',  ( -94.51749362711206004, -284.9859424490852007, -316.2630472235535990 ) ) ;
#53875 = CARTESIAN_POINT ( 'NONE',  ( 36.56804806138858766, -283.5365524708048497, -288.0610409790464814 ) ) ;
#53876 = CARTESIAN_POINT ( 'NONE',  ( -108.4627552590530968, -284.1240525449600227, -253.4049209915497727 ) ) ;
#53877 = CARTESIAN_POINT ( 'NONE',  ( -21.50095326729297085, -275.2456558486217659, -342.4935709810504818 ) ) ;
#53878 = CARTESIAN_POINT ( 'NONE',  ( -32.03413807419986625, -284.8448989782980334, -344.4063424466788774 ) ) ;
#53879 = CARTESIAN_POINT ( 'NONE',  ( -69.57196504867188480, -275.9641099762362728, -336.6466336187812658 ) ) ;
#53880 = CARTESIAN_POINT ( 'NONE',  ( -16.56617244506084674, -275.4065258706298209, -200.0045375989336094 ) ) ;
#53881 = CARTESIAN_POINT ( 'NONE',  ( 194.2984252800551417, 39.76179767010464161, 14.57344116787098720 ) ) ;
#53882 = CARTESIAN_POINT ( 'NONE',  ( -100.1229642933790984, -279.9424045037632709, -226.0590673475633992 ) ) ;
#53883 = ORIENTED_EDGE ( 'NONE', *, *, #15423, .T. ) ;
#53884 = LINE ( 'NONE', #86015, #79223 ) ;
#53885 = CARTESIAN_POINT ( 'NONE',  ( -60.16083807697842190, -287.6200072634221669, -198.0596803194119673 ) ) ;
#53886 = ADVANCED_FACE ( 'NONE', ( #59551, #1304, #50572 ), #59074, .T. ) ;
#53887 = CARTESIAN_POINT ( 'NONE',  ( -4.272798959704450894, -293.8018483010718001, -335.6365400018029845 ) ) ;
#53888 = CARTESIAN_POINT ( 'NONE',  ( -98.08419835199266856, -289.2701675944013573, -317.5168355214228768 ) ) ;
#53889 = CARTESIAN_POINT ( 'NONE',  ( 36.69463280298963070, -285.7652689710423033, -268.3063860241469456 ) ) ;
#53891 = CARTESIAN_POINT ( 'NONE',  ( -84.45710032901575914, -289.6329138788665318, -213.2812347063773757 ) ) ;
#53890 = CARTESIAN_POINT ( 'NONE',  ( 13.56012671391319024, -285.3563272338353158, -217.1459111527044286 ) ) ;
#53892 = CARTESIAN_POINT ( 'NONE',  ( -40.00360392058113490, -287.2230409904963722, -197.0123294858813665 ) ) ;
#53893 = CARTESIAN_POINT ( 'NONE',  ( -98.04636780952390041, -275.9518301111650658, -314.4277605498646153 ) ) ;
#53894 = CARTESIAN_POINT ( 'NONE',  ( -36.12031628919270787, -287.4369904482509241, -346.5643059251794398 ) ) ;
#53895 = CARTESIAN_POINT ( 'NONE',  ( -43.52739389118366375, -287.9742998346473541, -195.5647578969625897 ) ) ;
#53896 = CARTESIAN_POINT ( 'NONE',  ( 34.19495515066807201, -285.8492817030654010, -293.4378460432636757 ) ) ;
#53897 = CARTESIAN_POINT ( 'NONE',  ( 1.235408126949466112, -283.4648075695793636, -332.6715656782942574 ) ) ;
#53898 = CARTESIAN_POINT ( 'NONE',  ( -45.79370798446272062, -291.1590929129508254, -345.1029515984594127 ) ) ;
#53899 = FACE_OUTER_BOUND ( 'NONE', #12750, .T. ) ;
#53900 = CARTESIAN_POINT ( 'NONE',  ( 156.4851178187871312, 15.00000000000000000, 7.000000000000000000 ) ) ;
#53901 = CARTESIAN_POINT ( 'NONE',  ( -112.5081904911771318, -298.3741531467688901, -278.0626063502048737 ) ) ;
#53902 = CARTESIAN_POINT ( 'NONE',  ( 25.36843145603753769, -278.9957808249042728, -229.1281386727530958 ) ) ;
#53903 = CARTESIAN_POINT ( 'NONE',  ( -64.32250657930283921, -290.9061701429879463, -198.3592885442645866 ) ) ;
#53904 = CARTESIAN_POINT ( 'NONE',  ( -89.07704497911473140, -294.1939058613223210, -323.0627430589873939 ) ) ;
#53905 = CARTESIAN_POINT ( 'NONE',  ( 14.25908599712159486, -280.9936110619752867, -322.7644116494458899 ) ) ;
#53906 = CARTESIAN_POINT ( 'NONE',  ( 25.01281134039493637, -273.0795079742320581, -229.7011979500600489 ) ) ;
#53907 = CARTESIAN_POINT ( 'NONE',  ( -41.04744583537010527, -296.4149053782379610, -343.7734359737297609 ) ) ;
#53908 = CARTESIAN_POINT ( 'NONE',  ( 154.7659666677267580, 19.56018909072085066, 12.94946946941272437 ) ) ;
#53909 = CARTESIAN_POINT ( 'NONE',  ( -100.7096567525790078, -271.6948415323470840, -227.5690797961061946 ) ) ;
#53910 = CARTESIAN_POINT ( 'NONE',  ( -47.51833934386024794, -293.4196790688521332, -345.6632429621491269 ) ) ;
#53911 = CARTESIAN_POINT ( 'NONE',  ( 22.27145705071026782, -294.3783714648906766, -227.1928959682260825 ) ) ;
#53912 = DIRECTION ( 'NONE',  ( 0.5068419345592570791, -1.196319445165339194E-14, 0.8620390091940327570 ) ) ;
#53913 = CARTESIAN_POINT ( 'NONE',  ( 31.95068112580397468, -294.0418635494150976, -246.7265200021890621 ) ) ;
#53914 = CARTESIAN_POINT ( 'NONE',  ( 152.4536156746142410, 276.0000000000000568, -11.99999999999999112 ) ) ;
#53916 = CARTESIAN_POINT ( 'NONE',  ( -6.764908165342906621, -294.6392031248318517, -336.6488226740592609 ) ) ;
#53915 = CARTESIAN_POINT ( 'NONE',  ( -38.72811899457374807, -281.0895736199433941, -345.7035671683970577 ) ) ;
#53917 = CARTESIAN_POINT ( 'NONE',  ( -58.48674883771838751, -283.3180535985534902, -344.4563821424607113 ) ) ;
#53918 = CARTESIAN_POINT ( 'NONE',  ( -28.41976538749815973, -282.0845130842482718, -195.2770821648892081 ) ) ;
#53919 = CARTESIAN_POINT ( 'NONE',  ( -73.59930161816321004, -285.2514998133198674, -202.3967750621636128 ) ) ;
#53920 = CARTESIAN_POINT ( 'NONE',  ( -110.7418340484448862, -288.3635819211841635, -285.0023944294387661 ) ) ;
#53921 = CARTESIAN_POINT ( 'NONE',  ( 175.2296996224750103, 249.5000000000000568, 0.000000000000000000 ) ) ;
#53922 = CARTESIAN_POINT ( 'NONE',  ( 37.31044519307619822, -279.8318005328021059, -254.4945804494235801 ) ) ;
#53923 = CARTESIAN_POINT ( 'NONE',  ( 37.20070123609671242, -286.6994925912204053, -288.4421709853007201 ) ) ;
#53924 = CARTESIAN_POINT ( 'NONE',  ( 207.3682846056400990, 30.42003702808571930, 14.46447120960799992 ) ) ;
#53925 = CARTESIAN_POINT ( 'NONE',  ( -80.60749199442902579, -297.2501251212485158, -330.1483379166115242 ) ) ;
#53926 = CARTESIAN_POINT ( 'NONE',  ( -34.29627077004398927, -278.4398304005497948, -346.7111779306290487 ) ) ;
#53927 = CARTESIAN_POINT ( 'NONE',  ( -27.55133941464711711, -279.8465300468889154, -197.9480688981650474 ) ) ;
#53928 = CARTESIAN_POINT ( 'NONE',  ( 38.35764393178612153, -293.8959734726582838, -284.5252533351341526 ) ) ;
#53929 = CARTESIAN_POINT ( 'NONE',  ( -110.8245891400314207, -282.4070642323220000, -288.0108250370809060 ) ) ;
#53930 = CARTESIAN_POINT ( 'NONE',  ( -97.19162719896338842, -279.9340384990928783, -315.5815996233719147 ) ) ;
#53931 = CARTESIAN_POINT ( 'NONE',  ( 34.29523675194236176, -292.8117810432837018, -285.6382455006382770 ) ) ;
#53932 = CARTESIAN_POINT ( 'NONE',  ( -106.3832319209072210, -270.9413509134250830, -240.5093051803292497 ) ) ;
#53933 = ORIENTED_EDGE ( 'NONE', *, *, #41260, .F. ) ;
#53934 = CARTESIAN_POINT ( 'NONE',  ( 152.4536156746142410, 249.5000000000000568, 12.00000000000000000 ) ) ;
#53935 = CARTESIAN_POINT ( 'NONE',  ( 24.47598140093117891, -293.5984367773336885, -309.3992091009642991 ) ) ;
#53936 = LINE ( 'NONE', #82805, #39868 ) ;
#53937 = CARTESIAN_POINT ( 'NONE',  ( -105.5937364680635966, -287.8380690714489560, -285.9065529553535612 ) ) ;
#53938 = CARTESIAN_POINT ( 'NONE',  ( -95.89798262376837101, -272.4216309774337219, -220.5882690116843037 ) ) ;
#53939 = CARTESIAN_POINT ( 'NONE',  ( 19.90652774611973541, -288.1746318800582571, -219.5292287197438554 ) ) ;
#53940 = CARTESIAN_POINT ( 'NONE',  ( 17.82413554364205410, -288.0675005545263048, -318.2461139030481831 ) ) ;
#53941 = CARTESIAN_POINT ( 'NONE',  ( -81.21680477907024454, -279.1809913658900086, -329.5699259632511371 ) ) ;
#53942 = CARTESIAN_POINT ( 'NONE',  ( -97.72222600681112681, -298.9017730806181703, -227.5573084651370834 ) ) ;
#53943 = EDGE_CURVE ( 'NONE', #80622, #53974, #18336, .T. ) ;
#53944 = CARTESIAN_POINT ( 'NONE',  ( -103.7224464993235244, -277.7693601481302039, -238.9251503143225648 ) ) ;
#53945 = EDGE_LOOP ( 'NONE', ( #41645, #91946 ) ) ;
#53946 = CARTESIAN_POINT ( 'NONE',  ( -93.64438738855700706, -296.9353986855291510, -217.7881165983977780 ) ) ;
#53947 = CARTESIAN_POINT ( 'NONE',  ( -110.3462528574607262, -292.2832624770505277, -284.9743890083857991 ) ) ;
#53948 = CARTESIAN_POINT ( 'NONE',  ( 36.64029018806093063, -294.9215564576508086, -252.1099392021816072 ) ) ;
#53949 = DIRECTION ( 'NONE',  ( 0.000000000000000000, 0.000000000000000000, 1.000000000000000000 ) ) ;
#53950 = EDGE_CURVE ( 'NONE', #11243, #4576, #9316, .T. ) ;
#53951 = CARTESIAN_POINT ( 'NONE',  ( -95.84491834727843695, -290.5889011061078122, -314.2142549186395399 ) ) ;
#53952 = CARTESIAN_POINT ( 'NONE',  ( -48.18343439338273981, -255.8486676696398376, -444.0454921972241209 ) ) ;
#53953 = CARTESIAN_POINT ( 'NONE',  ( -14.22049088873750478, -290.4883110271226769, -198.1553928893376337 ) ) ;
#53954 = CARTESIAN_POINT ( 'NONE',  ( -3.426341716943643867, -298.7991852461717599, -193.3803966899450870 ) ) ;
#53955 = CARTESIAN_POINT ( 'NONE',  ( -104.4337324863256526, -272.4496981626587058, -241.3080712163742021 ) ) ;
#53956 = DIRECTION ( 'NONE',  ( 1.000000000000000000, 0.000000000000000000, 0.000000000000000000 ) ) ;
#53957 = CYLINDRICAL_SURFACE ( 'NONE', #55250, 2.395975569037589459 ) ;
#53958 = CARTESIAN_POINT ( 'NONE',  ( -112.4474098728420017, -291.9011607344708636, -283.9196297246145946 ) ) ;
#53959 = CARTESIAN_POINT ( 'NONE',  ( -19.05039376806008633, -297.3376638359844719, -350.3538533559490702 ) ) ;
#53960 = CARTESIAN_POINT ( 'NONE',  ( -46.98576043290659499, -287.9296857604794013, -196.0997641079692642 ) ) ;
#53961 = CARTESIAN_POINT ( 'NONE',  ( 6.265240006256610705, -272.6451177045447594, -209.4820650045920445 ) ) ;
#53962 = CARTESIAN_POINT ( 'NONE',  ( 31.49732882592432759, -277.0983745798826021, -241.8974049203969514 ) ) ;
#53963 = CARTESIAN_POINT ( 'NONE',  ( 0.6648867880497250082, -290.6429958369953397, -206.3547624477920124 ) ) ;
#53964 = CARTESIAN_POINT ( 'NONE',  ( -73.48638747381571079, -279.3867989933838203, -336.9631661669442906 ) ) ;
#53965 = ORIENTED_EDGE ( 'NONE', *, *, #70607, .F. ) ;
#53966 = CARTESIAN_POINT ( 'NONE',  ( 18.56696251739005277, -281.5690458506816185, -317.4774054465676159 ) ) ;
#53967 = CARTESIAN_POINT ( 'NONE',  ( -111.5249209800548584, -279.3867733321280298, -289.8637042524648564 ) ) ;
#53968 = CARTESIAN_POINT ( 'NONE',  ( 36.60574977127839702, -280.0948240150589186, -250.3167529644021556 ) ) ;
#53969 = CARTESIAN_POINT ( 'NONE',  ( -71.72385729004520272, -195.2026553322960751, -357.3366892497529079 ) ) ;
#53970 = CARTESIAN_POINT ( 'NONE',  ( 15.85532545509639846, -275.7251389392940837, -215.0176749958938274 ) ) ;
#53971 = SHAPE_DEFINITION_REPRESENTATION ( #12657, #71246 ) ;
#53972 = CARTESIAN_POINT ( 'NONE',  ( -71.11352178364819565, -275.1346028521467701, -201.9347209012333622 ) ) ;
#53973 = CARTESIAN_POINT ( 'NONE',  ( -114.2704648735229114, -299.0519495502701943, -270.3937649182068981 ) ) ;
#53974 = VERTEX_POINT ( 'NONE', #66640 ) ;
#53975 = ORIENTED_EDGE ( 'NONE', *, *, #12686, .T. ) ;
#53976 = CARTESIAN_POINT ( 'NONE',  ( 11.63197158325052172, -285.8906705383787994, 47.50000000000000711 ) ) ;
#53977 = CARTESIAN_POINT ( 'NONE',  ( -48.09278901894641223, -290.2716825594848729, -342.9288371990923565 ) ) ;
#53978 = CARTESIAN_POINT ( 'NONE',  ( -71.43150295606771749, -291.2563136431152770, -338.2717898981143776 ) ) ;
#53979 = CARTESIAN_POINT ( 'NONE',  ( -100.3960693493331036, -289.3923899523622936, -307.4478506293191344 ) ) ;
#53980 = CARTESIAN_POINT ( 'NONE',  ( -43.65496042878422855, -285.4821942428148986, -193.6288974966489604 ) ) ;
#53981 = CARTESIAN_POINT ( 'NONE',  ( 208.4306832106270804, -147.7221692137691775, 0.000000000000000000 ) ) ;
#53982 = CARTESIAN_POINT ( 'NONE',  ( 36.22472651994197435, -280.0365765040768906, -276.8414469592522664 ) ) ;
#53983 = CARTESIAN_POINT ( 'NONE',  ( 33.44437681840988574, -289.1205248519243582, -247.9535251638666011 ) ) ;
#53984 = CARTESIAN_POINT ( 'NONE',  ( -5.753147139932202059, -281.1090146610890770, -336.9548073770945962 ) ) ;
#53985 = CARTESIAN_POINT ( 'NONE',  ( -106.7242638539525927, -279.5452974409242870, -294.7496976920084535 ) ) ;
#53986 = CARTESIAN_POINT ( 'NONE',  ( 23.10960723032857800, -289.1279196965655842, -317.6946500689371078 ) ) ;
#53987 = CARTESIAN_POINT ( 'NONE',  ( -79.09516679938916184, -279.9640859369499708, -210.4058307892098867 ) ) ;
#53988 = CARTESIAN_POINT ( 'NONE',  ( -86.24767197844842315, -290.1862100530678958, -211.3328232904735557 ) ) ;
#53989 = CARTESIAN_POINT ( 'NONE',  ( -106.5381401926974689, -285.7844977389461292, -236.9543596486820434 ) ) ;
#53990 = CARTESIAN_POINT ( 'NONE',  ( 18.30265299723423311, -287.3166245345396987, -217.1501875626344429 ) ) ;
#53991 = CARTESIAN_POINT ( 'NONE',  ( -110.2283714244402972, -284.7833906097777685, -265.4673190576978641 ) ) ;
#53992 = EDGE_LOOP ( 'NONE', ( #43852, #41746, #82360, #83006, #45421 ) ) ;
#53993 = CARTESIAN_POINT ( 'NONE',  ( 204.5044540939250055, -147.7221692137691775, 10.75739200365177695 ) ) ;
#53994 = CARTESIAN_POINT ( 'NONE',  ( -66.56131965836367215, -293.5339097416036225, -200.4574748994489539 ) ) ;
#53995 = CARTESIAN_POINT ( 'NONE',  ( 20.98078239598116213, -292.9087710980380734, -319.8766337963498358 ) ) ;
#53996 = CARTESIAN_POINT ( 'NONE',  ( 34.39262373772408665, -274.8048640757493786, -285.1122273752473575 ) ) ;
#53997 = CARTESIAN_POINT ( 'NONE',  ( -113.1049059125042362, -295.7321387567311604, -283.8246259857402265 ) ) ;
#53998 = CARTESIAN_POINT ( 'NONE',  ( -101.7200378557766385, -289.5190440767757991, -234.3935975212878873 ) ) ;
#53999 = CARTESIAN_POINT ( 'NONE',  ( -73.82110537864811306, -293.7835279315664252, -334.7600854182182957 ) ) ;
#54000 = CARTESIAN_POINT ( 'NONE',  ( -60.39818083590582631, -292.9516190491950169, -200.6261575995077919 ) ) ;
#54001 = CARTESIAN_POINT ( 'NONE',  ( 208.3342852401368930, 35.82745088358564800, 14.32871520589203485 ) ) ;
#54002 = CARTESIAN_POINT ( 'NONE',  ( 7.771451739761555011, -290.6659425388409090, -210.1726681005685862 ) ) ;
#54003 = CARTESIAN_POINT ( 'NONE',  ( 34.37138275451705738, -295.2687153460863101, -248.3578371875492223 ) ) ;
#54004 = CARTESIAN_POINT ( 'NONE',  ( 33.93283969678166301, -288.7147595850378252, -287.1940743976730914 ) ) ;
#54005 = EDGE_CURVE ( 'NONE', #70302, #51305, #87696, .T. ) ;
#54006 = EDGE_CURVE ( 'NONE', #25330, #1451, #30651, .T. ) ;
#54007 = CARTESIAN_POINT ( 'NONE',  ( -28.76270564614470970, -278.9239159720255543, -345.2788136133865464 ) ) ;
#54008 = CARTESIAN_POINT ( 'NONE',  ( -95.85586566241099149, -276.6773954718863138, -319.8192204087628738 ) ) ;
#54009 = CARTESIAN_POINT ( 'NONE',  ( -30.49217837075662629, -297.3330341154982648, -193.5234988838759875 ) ) ;
#54010 = CARTESIAN_POINT ( 'NONE',  ( -75.21782698397862532, -277.6234137888233704, -206.2182377461876115 ) ) ;
#54011 = CARTESIAN_POINT ( 'NONE',  ( -82.09308442490045366, -276.0510868019468376, -332.0356995951354406 ) ) ;
#54012 = CARTESIAN_POINT ( 'NONE',  ( -103.2175812133921795, -294.7969091626975455, -303.0585572695978840 ) ) ;
#54013 = CARTESIAN_POINT ( 'NONE',  ( 199.8839601302323388, 66.89258700486192311, 4.790067391029672272 ) ) ;
#54014 = CARTESIAN_POINT ( 'NONE',  ( -44.59524583593257319, -298.7609995928901867, -197.5096093526454126 ) ) ;
#54015 = DIRECTION ( 'NONE',  ( 0.8526555397811738102, 0.000000000000000000, -0.5224734734706395489 ) ) ;
#54017 = CARTESIAN_POINT ( 'NONE',  ( -2.911783122493571963, -274.3539869446985335, -205.9904661332122089 ) ) ;
#54016 = CARTESIAN_POINT ( 'NONE',  ( -43.08268294367599793, -287.1444101556076021, -345.4973137837422996 ) ) ;
#54018 = CARTESIAN_POINT ( 'NONE',  ( 28.90374401279980532, -288.0635153542899047, -309.6108457596720314 ) ) ;
#54019 = CARTESIAN_POINT ( 'NONE',  ( -102.6495905338611152, -275.0486224168494687, -233.0422515417800753 ) ) ;
#54020 = CARTESIAN_POINT ( 'NONE',  ( -111.6275497342932965, -294.4303608835563182, -279.8127487419566819 ) ) ;
#54021 = CARTESIAN_POINT ( 'NONE',  ( -71.67578070230914022, -282.6914594827607630, -339.1021518149162262 ) ) ;
#54022 = DIRECTION ( 'NONE',  ( -1.000000000000000000, 0.000000000000000000, 0.000000000000000000 ) ) ;
#54023 = CARTESIAN_POINT ( 'NONE',  ( -108.6974721796673009, -276.8521163581933138, -247.1011516359438929 ) ) ;
#54024 = LINE ( 'NONE', #84296, #26299 ) ;
#54025 = CARTESIAN_POINT ( 'NONE',  ( -110.1854662083769796, -289.2290494336387496, -279.3564638845061836 ) ) ;
#54026 = CARTESIAN_POINT ( 'NONE',  ( 199.7979780134897396, 41.13815025368441525, 10.63455718547532314 ) ) ;
#54027 = DIRECTION ( 'NONE',  ( 0.000000000000000000, 1.000000000000000000, 0.000000000000000000 ) ) ;
#54028 = CARTESIAN_POINT ( 'NONE',  ( -108.9024742553985874, -288.8421187518065381, -247.8667052473525132 ) ) ;
#54029 = CARTESIAN_POINT ( 'NONE',  ( 9.914998316094164821, -276.2366864732580325, -213.7477589742381383 ) ) ;
#54030 = CARTESIAN_POINT ( 'NONE',  ( 39.03144406008818379, -283.0076414011805355, -272.7588540303314062 ) ) ;
#54032 = CARTESIAN_POINT ( 'NONE',  ( -61.53472301329966854, -283.3752504545788042, -339.2888606260656843 ) ) ;
#54031 = CARTESIAN_POINT ( 'NONE',  ( -35.49620289696337494, -296.0952583471702724, -195.0065285614429911 ) ) ;
#54033 = CARTESIAN_POINT ( 'NONE',  ( -57.03663203377729474, -275.2185029534903720, -199.4032152805806390 ) ) ;
#54034 = CARTESIAN_POINT ( 'NONE',  ( 34.05308873701784478, -276.5660847958113777, -286.3989159558601045 ) ) ;
#54035 = CARTESIAN_POINT ( 'NONE',  ( -19.37223705524605677, -284.8212877209050475, -343.2301662594349523 ) ) ;
#54036 = ORIENTED_EDGE ( 'NONE', *, *, #45976, .F. ) ;
#54037 = DIRECTION ( 'NONE',  ( 0.000000000000000000, 0.000000000000000000, 1.000000000000000000 ) ) ;
#54038 = CARTESIAN_POINT ( 'NONE',  ( 24.88502695502878836, -293.9876565002855955, -315.7356637823843357 ) ) ;
#54039 = CARTESIAN_POINT ( 'NONE',  ( -104.4813085449890622, -286.0987512858225159, -303.1005911705772178 ) ) ;
#54040 = CARTESIAN_POINT ( 'NONE',  ( 175.2296996224750103, 133.0000000000000000, 0.000000000000000000 ) ) ;
#54041 = CARTESIAN_POINT ( 'NONE',  ( -111.2869819898779866, -281.6237833571633473, -305.9350535429201159 ) ) ;
#54042 = CARTESIAN_POINT ( 'NONE',  ( -37.13768075069169328, -276.2467958809954780, -347.2124025583008233 ) ) ;
#54043 = CARTESIAN_POINT ( 'NONE',  ( -113.4532250340788693, -288.9056318710334494, -274.0321110462006118 ) ) ;
#54044 = CARTESIAN_POINT ( 'NONE',  ( -5.718016765509383426, -284.1487660287102130, -336.9381312271985394 ) ) ;
#54045 = CARTESIAN_POINT ( 'NONE',  ( -85.75133073334696121, -279.4928756592313448, -326.4154309696538121 ) ) ;
#54046 = CARTESIAN_POINT ( 'NONE',  ( 7.185722172988596057, -288.0705758170323065, -208.1999471684363527 ) ) ;
#54047 = CARTESIAN_POINT ( 'NONE',  ( -16.38666980254915728, -282.3231646714657472, -198.3480125763209969 ) ) ;
#54048 = CARTESIAN_POINT ( 'NONE',  ( 38.72727800654578800, -275.5684704136840537, -258.3383640673652621 ) ) ;
#54049 = CARTESIAN_POINT ( 'NONE',  ( -77.81670765481877083, -277.4128324662781893, -335.9270777748633350 ) ) ;
#54050 = CARTESIAN_POINT ( 'NONE',  ( -98.07140855564131243, -299.0617600786443404, -227.3121143527116317 ) ) ;
#54051 = CARTESIAN_POINT ( 'NONE',  ( 159.4572718888341285, 15.48129629386906281, 10.01740370621924292 ) ) ;
#54052 = CARTESIAN_POINT ( 'NONE',  ( 21.27581636871892101, -283.4090924074130839, -223.5744983911110353 ) ) ;
#54053 = CARTESIAN_POINT ( 'NONE',  ( -75.14274473285500733, -295.6940649792166482, -204.6397676035028894 ) ) ;
#54054 = DIRECTION ( 'NONE',  ( -1.000000000000000000, 0.000000000000000000, 0.000000000000000000 ) ) ;
#54055 = CARTESIAN_POINT ( 'NONE',  ( -51.29877536669942373, -276.7430977463810677, -342.0771447286907119 ) ) ;
#54056 = CARTESIAN_POINT ( 'NONE',  ( 23.30900661503532589, -276.1292450733118926, -223.5476736826244064 ) ) ;
#54057 = CARTESIAN_POINT ( 'NONE',  ( -24.99453589156636824, -287.9717748042413632, -197.3329386761267870 ) ) ;
#54058 = CARTESIAN_POINT ( 'NONE',  ( -112.7078449822472521, -298.2240461152812259, -258.3345120083503730 ) ) ;
#54059 = CARTESIAN_POINT ( 'NONE',  ( -81.62956339276007611, -296.8449640314987619, -332.9286472458695130 ) ) ;
#54060 = CARTESIAN_POINT ( 'NONE',  ( -34.82039927017625303, -294.0840653045207773, -195.5702664614639730 ) ) ;
#54061 = CARTESIAN_POINT ( 'NONE',  ( -93.56953765346997898, -277.2397834047061451, -220.9608803310800340 ) ) ;
#54062 = CARTESIAN_POINT ( 'NONE',  ( -35.65419579538057349, -281.9936081159942773, -195.9275958805040432 ) ) ;
#54063 = CARTESIAN_POINT ( 'NONE',  ( -87.04394116810205162, -295.4334165023100809, -214.9445010610481859 ) ) ;
#54064 = CARTESIAN_POINT ( 'NONE',  ( -87.48600437731853674, -285.6030721609664056, -327.2277537317200427 ) ) ;
#54065 = EDGE_CURVE ( 'NONE', #85072, #57747, #31131, .T. ) ;
#54066 = CARTESIAN_POINT ( 'NONE',  ( 32.57251878286696467, -286.1809118724847849, -248.2684866787102180 ) ) ;
#54067 = CARTESIAN_POINT ( 'NONE',  ( -97.80750439109840499, -248.8887263784241668, -333.8114341845347326 ) ) ;
#54068 = ORIENTED_EDGE ( 'NONE', *, *, #71679, .T. ) ;
#54069 = CARTESIAN_POINT ( 'NONE',  ( 33.73187304974455714, -286.9972326927515951, -253.5549114796776848 ) ) ;
#54070 = ORIENTED_EDGE ( 'NONE', *, *, #6030, .T. ) ;
#54071 = CARTESIAN_POINT ( 'NONE',  ( -90.21503184404798503, -284.8582719452872425, -325.9848275579730057 ) ) ;
#54072 = CARTESIAN_POINT ( 'NONE',  ( -2.907435594079280428, -274.8538673597004163, -205.9688132184403457 ) ) ;
#54073 = CARTESIAN_POINT ( 'NONE',  ( -23.84072744710957537, -285.0157497171977639, -194.9033828854142030 ) ) ;
#54074 = CARTESIAN_POINT ( 'NONE',  ( -11.24545392176759862, -291.3045843531622268, -198.1909580222750265 ) ) ;
#54075 = CARTESIAN_POINT ( 'NONE',  ( 39.38500731920789377, -282.5236990018889855, -272.7761907766800391 ) ) ;
#54076 = CARTESIAN_POINT ( 'NONE',  ( -107.8791836013111549, -280.4455523805548296, -241.2549128642503149 ) ) ;
#54077 = CARTESIAN_POINT ( 'NONE',  ( 36.15425854676276174, -281.5977567520299658, -247.4681419858337676 ) ) ;
#54078 = CARTESIAN_POINT ( 'NONE',  ( 17.36665895637873192, -285.6952119285918457, -314.0302885647153062 ) ) ;
#54079 = CARTESIAN_POINT ( 'NONE',  ( -89.67988014755925974, -230.8544109942510545, -347.9892254545792412 ) ) ;
#54080 = ORIENTED_EDGE ( 'NONE', *, *, #73503, .T. ) ;
#54081 = CARTESIAN_POINT ( 'NONE',  ( -15.83008848003553481, -278.7735471720542364, -342.0902782102641595 ) ) ;
#54082 = CARTESIAN_POINT ( 'NONE',  ( 44.27645291422682305, 12.81384402874245332, -331.5602518763756734 ) ) ;
#54083 = CARTESIAN_POINT ( 'NONE',  ( 36.09929062543904621, -279.7454315888630845, -283.7843006428992112 ) ) ;
#54084 = CARTESIAN_POINT ( 'NONE',  ( -6.192328742830734534, -296.4085921700738595, -339.6697803456366955 ) ) ;
#54085 = CARTESIAN_POINT ( 'NONE',  ( -98.82352221797420100, -295.3531143395752565, -309.9997652490462201 ) ) ;
#54086 = CARTESIAN_POINT ( 'NONE',  ( -61.66317845459105484, -291.2521894909195339, -197.3119079829695295 ) ) ;
#54087 = DIRECTION ( 'NONE',  ( 1.000000000000000000, -0.000000000000000000, -0.000000000000000000 ) ) ;
#54089 = CARTESIAN_POINT ( 'NONE',  ( -5.465133247984220510, -287.0254846115550436, -336.9218038393461825 ) ) ;
#54088 = CARTESIAN_POINT ( 'NONE',  ( -105.9760417171177096, -295.5614950743363920, -236.7763975591273606 ) ) ;
#54090 = CARTESIAN_POINT ( 'NONE',  ( 36.94415581737101206, -295.4175296656277396, -270.7430259030278421 ) ) ;
#54091 = CARTESIAN_POINT ( 'NONE',  ( 30.40993689606916206, -288.4862012691365294, -241.7520533262001550 ) ) ;
#54092 = ORIENTED_EDGE ( 'NONE', *, *, #32585, .T. ) ;
#54093 = CARTESIAN_POINT ( 'NONE',  ( 33.20508585027005921, -294.8815766906969316, -300.7604272105157861 ) ) ;
#54094 = CARTESIAN_POINT ( 'NONE',  ( -95.16129769550697404, -284.4159489726229140, -315.0456464905165035 ) ) ;
#54095 = CARTESIAN_POINT ( 'NONE',  ( -105.6108339533654998, -294.8960019698889141, -305.2247252189152391 ) ) ;
#54096 = CARTESIAN_POINT ( 'NONE',  ( -113.5074846170469698, -291.4870196487693761, -259.8256539460477370 ) ) ;
#54097 = CARTESIAN_POINT ( 'NONE',  ( -112.2587832337740963, -291.2637922075107326, -252.8409135743088143 ) ) ;
#54098 = CARTESIAN_POINT ( 'NONE',  ( -71.17087407533799137, -289.6784229638754482, -335.0636241075252428 ) ) ;
#54099 = ORIENTED_EDGE ( 'NONE', *, *, #15644, .T. ) ;
#54100 = CARTESIAN_POINT ( 'NONE',  ( 157.4851178187871312, 15.19241473665912778, 8.999999999997330136 ) ) ;
#54101 = CARTESIAN_POINT ( 'NONE',  ( -100.5327758358061772, -298.9715923473462453, -228.5380401843699758 ) ) ;
#54102 = CARTESIAN_POINT ( 'NONE',  ( -35.51777851591091917, -272.8694600128239358, -193.7668436873507574 ) ) ;
#54103 = CARTESIAN_POINT ( 'NONE',  ( 10.05186962290427921, -281.4390921062220059, -326.2602082448455576 ) ) ;
#54104 = EDGE_LOOP ( 'NONE', ( #46696, #28563, #76477, #41475 ) ) ;
#54105 = EDGE_LOOP ( 'NONE', ( #76295, #76555, #10779, #18577 ) ) ;
#54106 = CARTESIAN_POINT ( 'NONE',  ( 39.64574763058467255, -275.0700209352943375, -271.1772532756260148 ) ) ;
#54107 = CARTESIAN_POINT ( 'NONE',  ( -108.9775298495964506, -294.8053684692861225, -287.7064578780840520 ) ) ;
#54108 = CARTESIAN_POINT ( 'NONE',  ( 14.61244068419422426, -278.1722401832040532, -323.4575643368825695 ) ) ;
#54109 = CARTESIAN_POINT ( 'NONE',  ( 0.09679817608398202933, -272.6957045914627429, -206.2430459753439322 ) ) ;
#54110 = CARTESIAN_POINT ( 'NONE',  ( -108.3498474304395245, -297.5127431717701256, -288.9842317282793829 ) ) ;
#54111 = CARTESIAN_POINT ( 'NONE',  ( -110.6932029985250523, -297.6171126579783959, -271.4815037568844787 ) ) ;
#54112 = DIRECTION ( 'NONE',  ( -1.000000000000000000, 0.000000000000000000, 0.000000000000000000 ) ) ;
#54113 = CARTESIAN_POINT ( 'NONE',  ( -111.8229346153797223, -298.3563747867192433, -254.2070924821041444 ) ) ;
#54114 = CARTESIAN_POINT ( 'NONE',  ( -101.3092036791678794, -271.1047608426662237, -230.5294058557962842 ) ) ;
#54115 = CARTESIAN_POINT ( 'NONE',  ( 18.91684969054837495, -294.8646757181084013, -317.0394667196880505 ) ) ;
#54116 = CARTESIAN_POINT ( 'NONE',  ( -65.53606030848951036, -290.2508619757775818, -202.3735825817680336 ) ) ;
#54117 = CARTESIAN_POINT ( 'NONE',  ( 207.7039919494849869, 30.29338434242846390, 15.02863188060213773 ) ) ;
#54118 = CARTESIAN_POINT ( 'NONE',  ( 26.87574231574916439, -275.4868107776628676, -227.9860428891059883 ) ) ;
#54119 = EDGE_CURVE ( 'NONE', #75846, #90412, #58160, .T. ) ;
#54120 = CARTESIAN_POINT ( 'NONE',  ( -104.3805482693073543, -273.1086193435667155, -241.3402251240709688 ) ) ;
#54121 = EDGE_CURVE ( 'NONE', #73562, #75506, #60113, .T. ) ;
#54122 = CARTESIAN_POINT ( 'NONE',  ( -31.73300502818941027, -284.9616076511811116, -345.5202890343200579 ) ) ;
#54123 = CARTESIAN_POINT ( 'NONE',  ( -63.75755852931569478, -282.0743193041981272, -342.1629334006395311 ) ) ;
#54124 = CARTESIAN_POINT ( 'NONE',  ( 206.1705337702867382, 1.000000000000000222, -7.166337341072456901 ) ) ;
#54125 = CARTESIAN_POINT ( 'NONE',  ( -101.9185556427580224, -283.2804724647268699, -304.8554705005352616 ) ) ;
#54126 = CARTESIAN_POINT ( 'NONE',  ( -49.81497601744149506, -281.2106031423585932, -344.5382415850646112 ) ) ;
#54127 = CARTESIAN_POINT ( 'NONE',  ( 36.17667299571633066, -274.0714121579113680, -266.1229832589045827 ) ) ;
#54128 = CARTESIAN_POINT ( 'NONE',  ( 4.212006058458619862, -282.6119890591320996, -207.8635962137862236 ) ) ;
#54129 = CARTESIAN_POINT ( 'NONE',  ( 208.4306832106270519, 1.063508326895939771, 7.500000000000014211 ) ) ;
#54130 = AXIS2_PLACEMENT_3D ( 'NONE', #63746, #48082, #54724 ) ;
#54131 = DIRECTION ( 'NONE',  ( 0.000000000000000000, 0.000000000000000000, 1.000000000000000000 ) ) ;
#54132 = CARTESIAN_POINT ( 'NONE',  ( -65.90820487019962570, -272.0844762455563455, -199.7043674272825342 ) ) ;
#54133 = CARTESIAN_POINT ( 'NONE',  ( -76.82958269729145684, -279.5793236916941851, -334.3804507435912683 ) ) ;
#54134 = APPLICATION_CONTEXT ( 'automotive_design' ) ;
#54135 = LINE ( 'NONE', #39907, #64999 ) ;
#54136 = CARTESIAN_POINT ( 'NONE',  ( -105.6924460988564931, -286.0518421878123831, -302.5712052283816433 ) ) ;
#54137 = ORIENTED_EDGE ( 'NONE', *, *, #34673, .F. ) ;
#54138 = CARTESIAN_POINT ( 'NONE',  ( 156.5008572375018332, 15.54442400203453190, -9.984260581291959369 ) ) ;
#54139 = CARTESIAN_POINT ( 'NONE',  ( -21.61033311015171066, -286.8504457223311306, -343.7452474685937887 ) ) ;
#54140 = CARTESIAN_POINT ( 'NONE',  ( 209.7064572754725873, 36.40703279031890816, 14.69807322781363546 ) ) ;
#54141 = CARTESIAN_POINT ( 'NONE',  ( -93.90982623053319855, -296.0066882905446164, -223.5742998329805573 ) ) ;
#54142 = CARTESIAN_POINT ( 'NONE',  ( -83.32970995497004196, -287.8296703210663736, -328.6360562458374375 ) ) ;
#54143 = CARTESIAN_POINT ( 'NONE',  ( 180.5468918863934960, 256.3577768311903355, -167.2605672291198857 ) ) ;
#54144 = CARTESIAN_POINT ( 'NONE',  ( -107.8765914782961630, -294.2197028893193078, -296.0057290955219287 ) ) ;
#54145 = CARTESIAN_POINT ( 'NONE',  ( 21.56737458551660680, -285.3744988849808237, -221.8592760431354236 ) ) ;
#54146 = CARTESIAN_POINT ( 'NONE',  ( 34.22644608494959328, -282.9165391619682168, -252.2975909449990297 ) ) ;
#54147 = CARTESIAN_POINT ( 'NONE',  ( 8.578378750397638086, -280.6725419322424955, -330.9030073413592277 ) ) ;
#54148 = CARTESIAN_POINT ( 'NONE',  ( -21.12933984521924557, -288.8382949273853910, -341.5380761506264662 ) ) ;
#54149 = CARTESIAN_POINT ( 'NONE',  ( -67.56474743446976561, -281.0729772658729644, -203.2508849506107538 ) ) ;
#54150 = CARTESIAN_POINT ( 'NONE',  ( -43.77545601388165153, -280.7717445389827162, -197.4327343074002954 ) ) ;
#54151 = CARTESIAN_POINT ( 'NONE',  ( 24.51627414453345466, -290.1141541016406222, -313.4855948307017002 ) ) ;
#54152 = CARTESIAN_POINT ( 'NONE',  ( -74.60450101871616368, -295.7001477204482853, -337.8039411495329318 ) ) ;
#54153 = ORIENTED_EDGE ( 'NONE', *, *, #56330, .F. ) ;
#54154 = CARTESIAN_POINT ( 'NONE',  ( -108.0775012092738905, -272.9411894920630175, -239.8051244167468781 ) ) ;
#54155 = CARTESIAN_POINT ( 'NONE',  ( -38.95791226330022283, -294.0116653546011776, -195.7338128963984332 ) ) ;
#54156 = CYLINDRICAL_SURFACE ( 'NONE', #16754, 4.999999999999990230 ) ;
#54157 = CARTESIAN_POINT ( 'NONE',  ( 21.27581636871892101, -277.4090924074130839, -223.5744983911110353 ) ) ;
#54158 = EDGE_LOOP ( 'NONE', ( #52673, #10083 ) ) ;
#54159 = CARTESIAN_POINT ( 'NONE',  ( 36.69098792003511988, -273.3844072212879723, -257.2801438398193454 ) ) ;
#54160 = FACE_OUTER_BOUND ( 'NONE', #56942, .T. ) ;
#54161 = CARTESIAN_POINT ( 'NONE',  ( -113.4362467417314377, -294.8900214476975066, -275.2673441416986861 ) ) ;
#54162 = CARTESIAN_POINT ( 'NONE',  ( 9.556821120296728367, -274.0655007057300168, -214.2196831090664659 ) ) ;
#54163 = CARTESIAN_POINT ( 'NONE',  ( -110.8122372985201594, -291.9893335689440619, -276.7087138429859010 ) ) ;
#54164 = B_SPLINE_SURFACE_WITH_KNOTS ( 'NONE', 3, 3, ( 
 ( #68811, #84854, #70683, #54578, #18604, #47469, #18371, #19773, #41534, #77544, #47712, #56240, #83693, #55309, #76141, #25932, #4633, #48643, #11275, #54815, #20252, #70460, #42000, #18854, #76612, #33507, #70914, #12204, #11735, #78024, #13164, #92664, #33047, #62413, #34919, #49128, #40128, #40588, #84162, #69045, #54352, #5587, #69975, #19310, #34459, #63367, #4174, #90773, #41048, #91255, #61937, #6047, #69502, #26419, #92197, #63832, #48172, #83226, #12694, #85102, #77073, #5115, #33993, #62896, #91732, #26885, #55772, #84625, #27353, #21175, #72764, #36776, #57638, #7886, #22561, #66145, #79423, #43415, #27836, #86026, #29217, #35855, #50983, #79868, #71384, #56725, #15008, #80324, #87414, #15464, #78940, #78484, #85571, #65227, #42473, #71861, #50044, #51435, #20718, #42955, #13620, #43867, #86961, #49588, #72310, #810, #86482, #6517, #35395, #28755, #14090, #64315, #93140, #6982, #21647, #93597, #332, #64772, #50525, #65696, #7431, #58116, #28295, #29690, #58574, #57185, #14558, #36311, #44336, #22114, #73247, #8358, #37241, #67532, #82649, #39532, #74152, #8809, #9755, #38147, #67063, #87874, #60890, #38629, #75553, #23956, #89269, #30143, #59971, #46192, #31083, #52831, #89740, #16396, #31541, #2662, #88809, #15943, #9269, #60429, #59027, #75097, #24419, #81709, #66596, #23024, #37690, #2199, #45247, #45714, #73700, #16858, #59504, #53300, #82185, #10677, #24902, #74626, #53782, #1717, #17341, #30601, #46651, #10206, #3114, #81249, #51902, #39075, #67988, #88355, #31997, #17798, #1261, #80795, #23506, #44797, #52374, #4515, #48526, #63253, #13056, #26298, #84050, #68454, #32931, #69856, #76496, #91618, #26773, #18258, #3588, #55658, #27239, #34346, #56127, #25816, #25357, #32478, #12088, #83106, #18732, #61823, #92084, #61375, #83571, #54237, #84511, #33876, #90208, #19196, #41417, #33392, #47111, #76019, #69383, #90655, #11151, #40013, #54696, #62291, #40465, #40936, #47593, #91128, #77427, #48056, #4991, #68930, #19657, #5476, #4061, #55192, #11620, #12567, #62785, #76960, #70350, #84980, #20132, #49016, #77914, #5938, #70803, #34810, #63723, #92548, #41892, #6163, #77663, #20832, #63012, #34572, #69151, #5239, #85222, #70098, #91843, #35033, #55419, #70572, #12815, #34110, #54931, #19423, #41655, #4279, #20373, #5697, #26998, #11845, #33157, #47817, #41161, #84272, #84739, #18964, #48285, #4743, #63481, #27466, #49701, #63947, #19887, #92786, #40695, #55886, #69614, #56358, #85685, #33623, #92311, #42114, #26531, #62048, #77188, #48758, #62532, #49244, #71030, #27954, #78139, #91373, #13277, #56844, #78597, #40236, #90882, #26045, #83811, #76719, #12317, #71980, #15121, #21774, #36898, #65814, #57302, #13739, #924, #66258, #73359, #1373, #64890, #64431, #52027, #51097, #28411, #57758, #7099, #37351, #71504, #28870, #93257, #29804, #72881, #6637, #58234, #80437, #72430, #42589, #35517, #14677, #35970, #86144, #21294, #82458, #43533, #79538, #79984, #86604, #7547, #22676, #87078, #43983, #50167, #58685, #44453, #79064, #36431, #50650, #51548, #8006, #14216, #43076, #65347, #15582, #30255, #454, #29341, #22227, #8471, #59146, #87991, #23144, #46766, #24539, #61487, #9868, #75211, #16057, #45843, #32121, #16978, #38743, #75667, #2321, #17457, #53423, #74748, #1839, #60087, #82307, #44910, #61017, #46307, #67648, #52488, #73813, #88474, #81827, #31202, #31655, #59627, #88926, #45364, #10326, #68105, #90319, #10791, #60546, #39652, #81363, #2774, #16513, #3230, #32597, #74267, #25473, #37804, #8926, #89384, #39193, #17915, #89863, #25023, #66710, #53895, #68575, #30726, #24074, #3712, #80912, #82763, #23621, #9390, #38274, #67187, #52950, #58376, #66852, #609, #65956, #86757, #36577, #15268, #30402, #29016, #65491, #30879, #52173, #52626, #29493, #87219, #44127, #81506, #22827, #22366, #88614, #23760, #9539, #43674, #73032, #45507, #59772, #21919, #51240, #1067, #57903, #65033, #81054, #80584, #29946, #16199, #73950, #50793, #7691, #51696, #8159, #14819, #16653, #80128, #79677, #66400, #72570, #37044, #58831, #1516, #87676, #15738, #74409, #134, #59294, #44599, #73504, #8614, #37490, #88141, #23298, #45049, #9065, #37943, #1987, #60228, #10469, #18515, #46911, #38880, #10936, #74898, #54971, #46452, #61624, #25161, #11418, #24695, #81971, #90917, #39803, #67334, #47853, #82903, #45993, #68725, #2465, #67788, #39334, #47380, #76756, #68253, #75811, #54035, #32735, #19000, #4315, #3376, #83848, #83366, #2913, #38424, #33193, #90456, #24217, #31342, #17601, #69186, #18058, #82453, #31798, #62084, #89068, #53578, #53092, #25614, #3855, #17127, #54496, #40270, #32264, #10010, #60691, #61170, #89531, #75353, #90006, #76293, #26083, #77702, #78175, #63048, #41689, #20868, #56400, #49279, #62570, #92827, #42626, #48322, #70606, #70138, #56882, #13312, #40733, #19456, #33660, #42151, #93297, #50203, #84773, #77223, #20410, #48793, #12851, #4779, #71545, #71069, #86182, #34608, #6201, #69650, #5734, #85722, #63519, #92346, #6679, #27032, #35067, #63987, #27501, #26566, #19922, #27990, #91411, #49738, #78637, #85261, #12351, #55454, #41201, #13777, #55921, #35556, #84305, #64469, #5275, #28447, #57341, #21334, #11882, #34143, #91878, #50687, #80023, #79573, #1409, #30768, #14716, #59668, #73398, #80950, #65383, #72020, #497, #36941, #43569, #58724, #16096, #44947, #59184, #72466, #30296, #88028, #15164, #23186, #73847, #23658, #65854, #962, #79107, #7583, #80473, #87115, #8508, #37387, #28908, #14256, #66297, #37842, #8963, #66748, #36469, #36010, #43114, #22713, #29, #57796, #29380, #58274, #15623, #52068, #88511, #1874, #87568, #7137, #22265, #44022, #51140, #64927, #86646, #72920, #21812, #8047, #29841, #51588, #44494, #45883, #24576, #24110, #46346, #75704, #10828, #82799, #52991, #53930, #17950, #31693, #46801, #68614, #54386, #53465, #82345, #52525, #81865, #68146, #67684, #61058, #89900, #67230, #81400, #39688, #61521, #3749, #90352, #74790, #38315, #16548, #3266, #31238, #2811, #9907, #25509, #74303, #38780, #2360, #32631, #25058, #9427, #10362, #45404, #32156, #60124, #88964, #17014, #60587, #75247, #89422, #17493, #39227, #15451, #15931, #797, #73234, #52361, #87861, #80782, #319, #30587, #74138, #79855, #8345, #7872, #88342, #44785, #72296, #50971, #65215, #73686, #31070, #81696, #22548, #14994, #51889, #80312, #44322, #36298, #9256, #8796, #23944, #66133, #37675, #7416, #37228, #23493, #1248, #30130, #38133, #58560, #66584, #1704, #59014, #58103, #51422, #59489, #29203, #81236, #16383, #23010, #43853, #86949, #72751, #45233, #87401, #67048, #2185, #59958, #88797, #29677, #52816, #43401, #22102, #36762, #65683, #4051, #47583, #53286, #75540, #75084, #61811, #18249, #45700, #24407, #38616, #83094, #4503, #55182, #89726, #82172, #25345, #53770, #82636, #9741, #76487, #54226, #91116, #39520, #11139, #74612, #10665, #90644, #46639, #68441, #11610, #31985, #47101, #76008, #3574, #31529, #24890, #40002, #67520, #25806, #68919, #32464, #17329, #2650, #46179, #17786, #60878, #61363, #89256, #90197, #10194, #32921, #54686, #26286, #40455, #83560, #69373, #39063, #18720, #67976, #33382, #62281, #3102, #16844, #60416, #85909, #70341, #76951, #5467, #41883, #19648, #63714, #21061, #49928, #64193, #77417, #35265, #93025, #20120, #28182 ),
 ( #34337, #40926, #13505, #49475, #48046, #34799, #57071, #49005, #28639, #84041, #84971, #48517, #4980, #19186, #41406, #77903, #12556, #78825, #85458, #12078, #91609, #69847, #56604, #71744, #33866, #63244, #26764, #92539, #27229, #56118, #62776, #13970, #27706, #64658, #13046, #78366, #55649, #70794, #42828, #5929, #20605, #6872, #92075, #42353, #71266, #6394, #84502, #35744, #93486, #86373, #37577, #1150, #80215, #29099, #50402, #65116, #58459, #72653, #8248, #36197, #7775, #22005, #87760, #44687, #66940, #52260, #37130, #81140, #57992, #87303, #86846, #73588, #9153, #50875, #38032, #51784, #59383, #43754, #79308, #36660, #15354, #79757, #66037, #88234, #23392, #66488, #14898, #8697, #1604, #22450, #30488, #16284, #2079, #44214, #73121, #57528, #65580, #58914, #695, #80673, #15829, #7319, #21524, #45135, #74036, #14449, #43306, #29579, #72201, #219, #30032, #51322, #22914, #24306, #55890, #88699, #46080, #81594, #55423, #91377, #23847, #76723, #5243, #90886, #70576, #30969, #31887, #89157, #45599, #59858, #82063, #60778, #3001, #4747, #17219, #26049, #41165, #11849, #69619, #16743, #19427, #63016, #67423, #27002, #2551, #54935, #31430, #48289, #77667, #60319, #12819, #26535, #34114, #74988, #52713, #10099, #83815, #53184, #40699, #91847, #84744, #12321, #38966, #77192, #70102, #18968, #19891, #48762, #74500, #47821, #33627, #9631, #67878, #62536, #84276, #41659, #38518, #49248, #5701, #86608, #58238, #65351, #87082, #56848, #56363, #43988, #43080, #20377, #49705, #92790, #29345, #63485, #20836, #85226, #28875, #64894, #92316, #50171, #72434, #64435, #34576, #27470, #6641, #63951, #78143, #13281, #85689, #35521, #71508, #71985, #78601, #93261, #14681, #79068, #7103, #42118, #21778, #36436, #71034, #28415, #27958, #50654, #35974, #6168, #35037, #13744, #21998, #22231, #42593, #57306, #86148, #14220, #21299, #57762, #79542, #458, #43537, #79988, #7551, #51101, #15125, #37807, #24077, #8929, #30729, #67651, #87994, #9393, #45367, #66714, #87531, #52030, #74270, #8010, #52953, #16516, #1842, #44456, #65819, #80440, #73816, #23147, #23624, #51552, #80915, #37354, #38277, #60090, #82310, #2777, #52491, #45846, #59630, #17460, #72885, #88477, #66261, #22679, #36902, #30258, #81366, #44913, #67190, #59150, #2325, #81831, #31205, #88929, #29807, #16981, #9871, #15585, #74751, #1376, #38747, #31658, #927, #73362, #58688, #60549, #89388, #8474, #16060, #24542, #53426, #83229, #18375, #39196, #12207, #83696, #26888, #69048, #40591, #75215, #11278, #91258, #76144, #4177, #41052, #61490, #76615, #18857, #40131, #61020, #25476, #47715, #10329, #26422, #11738, #33050, #17919, #68108, #53898, #47233, #90322, #90777, #25026, #54356, #10795, #69505, #33510, #55775, #69978, #25936, #5119, #46769, #61940, #75670, #62416, #91735, #39655, #84628, #4636, #48175, #32600, #3233, #54818, #55313, #68579, #84165, #77076, #33996, #19313, #3715, #62899, #46310, #32124, #89866, #82766, #58118, #71388, #35398, #19776, #78027, #21178, #27839, #42958, #71864, #63370, #48647, #6985, #72313, #14561, #7434, #70917, #70463, #77547, #86029, #34462, #63836, #13167, #43418, #12698, #34922, #5590, #35858, #78944, #41538, #64318, #36315, #92200, #92667, #27356, #64775, #14094, #56244, #93143, #86486, #78487, #85105, #20255, #20721, #42003, #49131, #6050, #56728, #49591, #85574, #50047, #13623, #42476, #28758, #28298, #93600, #6520, #57641, #50528, #21651, #65230, #335, #29220, #88357, #22116, #812, #15010, #59507, #74629, #31543, #66146, #29692, #1719, #30145, #59028, #79870, #52835, #30604, #67535, #15945, #81251, #50985, #51905, #38151, #23026, #44798, #81711, #8360, #23507, #52376, #80797, #7889, #1263, #16398, #43869, #67067, #45249, #73702, #58576, #72766, #87416, #87875, #37243, #37691, #65698, #8811, #51437, #74154, #9270, #2664, #16861, #66597, #45718, #22563, #2202, #80326, #31086, #38632, #15467, #86963, #59974, #88812, #73249, #36779, #23959, #9757, #44339, #40016, #91132, #26302, #40469, #53784, #11623, #69386, #90211, #4519, #55195, #4995, #18261, #76023, #60433, #24905, #61826, #68458, #83574, #18736, #10208, #89271, #47597, #19199, #84052, #48059, #17800, #17343, #24421, #4064, #75099, #10679, #82651, #61378, #82189, #31999, #39535, #25819, #53302, #60894, #76963, #76499, #12092, #46653, #89744, #3592, #40939, #47114, #75557, #69859, #46194, #39077, #67991, #32481, #3117, #25360, #54240, #83110, #11155, #68933, #32934, #33395, #90659, #54699, #62294, #42841, #26776, #70353, #20616, #13059, #77430, #79321, #56130, #48529, #35278, #19661, #63256, #84983, #64206, #63726, #92087, #93496, #28649, #93036, #27720, #50416, #34349, #27243, #42365, #12572, #34813, #20136, #28192, #71277, #55662, #5941, #13981, #6404, #49020, #57081, #5479, #14459, #41895, #85920, #49486, #6882, #77917, #41421, #86383, #21071, #62788, #43316, #78376, #70807, #49941, #91621, #92551, #56618, #71757, #72212, #85469, #78835, #13515, #35755, #33880, #57540, #64668, #84514, #21534, #36670, #23857, #66951, #59393, #86860, #229, #80226, #38043, #51793, #58005, #65127, #80684, #1159, #2091, #22923, #88246, #29109, #15839, #30981, #22015, #15362, #59869, #52723, #30042, #87772, #50885, #66497, #23404, #30499, #705, #9165, #65592, #45609, #44696, #79766, #51332, #29589, #88709, #14908, #22459, #43764, #52271, #1615, #72665, #73597, #74046, #66047, #7328, #36208, #8258, #58468, #7784, #87312, #44223, #37139, #73132, #8708, #58923, #37586, #16294, #81150, #45147, #81606, #16755, #11517, #17229, #39434, #38976, #25710, #75912, #9643, #82072, #2560, #47009, #62185, #19098, #53681, #46091, #83003, #17698, #46550, #67433, #40364, #18155, #55077, #3478, #68827, #38530, #68350, #54593, #10569, #32370, #69281, #89627, #11037, #39906, #61270, #89166, #82548, #3956, #31439, #83464, #32829, #90105, #74997, #60329, #10109, #75451, #24796, #25256, #53194, #54133, #67888, #61719, #90551, #83946, #4410, #18620, #33289, #3011, #47485, #31897, #76394, #26185, #60789, #74511, #91017, #24317, #34240, #40828, #63146, #5830, #77322, #27604, #78726, #13869, #28086, #41303, #92924, #56973, #77800, #85811, #42721, #86271, #34703, #63616, #47951, #12455, #49377, #56013, #71166, #6294, #91509, #76854, #35163, #6770, #71638, #35645, #5373, #4879, #70240, #91977, #27130, #64562, #92441, #19552, #93386, #28539, #11980, #26665, #84870, #57430, #69748, #33763, #20020, #48898, #62675, #55555, #64085, #56501, #12950, #20962, #49829, #84403, #48418, #85360, #41788, #70699, #20509, #78270, #13409, #42252, #7223, #50775, #72552, #22808, #51221, #79660, #81036, #16180, #80566, #15250, #37926, #21902, #14801, #29929, #36097, #22349, #43657, #15720, #58814, #43205, #87201, #1499, #87657, #7674, #51677, #57884, #66832, #29473, #44581, #8142, #88122, #36558, #65017, #73932, #73484, #50297, #30861, #65939, #28998, #8596, #79203, #65473, #80111, #30383, #59755, #44110, #37473, #37025, #66383, #1969, #45032, #73013, #21423, #59276, #591, #14346, #9048, #23280, #117, #72106, #58361, #52154, #1050, #86740, #52607, #39318, #82434, #25597, #10452, #46894, #16636, #68236, #54480, #81489, #2897, #83349, #40254, #17584, #75336, #45490, #54019, #75795, #18042, #81953, #90440, #24199, #89512, #74391, #60211, #38864, #82886, #9519, #89050, #18497, #10918 ),
 ( #61606, #74881, #38407, #47361, #61154, #23744, #4297, #3357, #2446, #89989, #67316, #53076, #24677, #3839, #33177, #60674, #32247, #25143, #39786, #69170, #76276, #53562, #88595, #68709, #17110, #11402, #31324, #32721, #45974, #9991, #67770, #31780, #46433, #18985, #26065, #12836, #55906, #92811, #77685, #20394, #83831, #41674, #27976, #54954, #70122, #56866, #13764, #84758, #48779, #47837, #27487, #49265, #85247, #55439, #63970, #91396, #63032, #76739, #33644, #12336, #56381, #11866, #62554, #85708, #78160, #49724, #26551, #84291, #41182, #78621, #19906, #19441, #20853, #42612, #6663, #40717, #5259, #71529, #62066, #69635, #48307, #91863, #4763, #90900, #13298, #70592, #27017, #42136, #71054, #77206, #34128, #5719, #34594, #63503, #92332, #6186, #35053, #38172, #21318, #64912, #86629, #67087, #66615, #15, #14241, #51923, #28893, #2220, #23979, #46213, #31561, #16416, #60453, #7123, #37709, #35993, #52853, #82207, #57782, #17362, #31104, #38649, #23045, #28432, #80813, #88375, #15962, #45269, #67553, #2682, #16879, #44816, #81731, #45738, #1738, #74649, #89288, #75117, #23525, #52394, #35539, #73719, #59991, #8830, #88830, #9775, #79089, #64454, #24441, #53322, #93280, #57325, #30625, #86167, #50189, #74172, #43099, #59526, #81271, #72004, #9289, #25376, #60915, #33412, #69404, #68007, #54715, #76979, #68950, #48545, #10227, #11173, #68475, #24923, #39094, #61395, #40034, #76044, #76517, #90227, #4081, #19217, #83593, #47614, #89761, #91152, #40954, #46669, #32952, #3611, #55213, #11640, #3136, #17816, #32016, #40487, #91638, #53800, #83126, #75573, #18756, #47131, #61844, #82668, #69875, #4536, #84528, #90676, #62311, #10695, #25836, #84067, #26318, #48075, #5014, #54256, #12109, #33896, #62803, #39552, #18277, #26792, #32497, #55678, #19676, #6418, #49034, #70368, #84998, #78390, #92565, #28207, #57551, #85935, #77930, #49956, #20153, #242, #85483, #6895, #64221, #50433, #63739, #27258, #36221, #78848, #12590, #86875, #57095, #13073, #13995, #41436, #41909, #13530, #86396, #22029, #49500, #21085, #93051, #71772, #58020, #43330, #42379, #29123, #28664, #70822, #77445, #72227, #35769, #63271, #5493, #56633, #14472, #42857, #34366, #92103, #64682, #71292, #7341, #93508, #21548, #56145, #79337, #65141, #5954, #20630, #34827, #27737, #35294, #37601, #14924, #16310, #38060, #74061, #44239, #52739, #80240, #51809, #72679, #22476, #1174, #45162, #43777, #51348, #16770, #66968, #38546, #15377, #73150, #30056, #67449, #8724, #8274, #74528, #9662, #89181, #29605, #58938, #31455, #45624, #7798, #37154, #80703, #36683, #50898, #2108, #66511, #15854, #30998, #59885, #65606, #87327, #1632, #87788, #719, #2577, #66062, #58483, #52286, #22938, #44712, #73613, #81166, #30513, #59409, #60344, #79782, #9181, #88264, #23421, #88725, #23873, #81621, #10125, #25274, #53699, #83481, #32847, #46109, #90123, #67904, #76873, #90568, #53210, #33783, #68844, #31913, #25726, #82089, #24815, #54151, #33305, #62698, #83020, #61736, #39925, #18638, #4898, #83966, #18172, #69767, #69299, #82566, #40848, #19114, #76412, #38991, #17249, #3495, #55098, #3972, #75013, #3027, #54610, #47025, #47969, #47506, #11534, #60805, #40381, #12000, #89644, #32388, #24333, #17714, #75928, #11055, #46567, #4427, #62203, #91033, #75466, #26203, #10587, #39450, #68367, #61288, #41806, #56991, #55574, #91995, #57448, #78744, #79221, #56034, #27148, #70717, #14364, #49397, #63165, #21443, #50316, #36116, #70259, #5849, #72124, #86289, #19570, #84889, #92459, #84422, #91528, #13887, #13426, #27623, #42741, #6790, #48437, #34258, #78288, #34720, #41322, #43224, #20039, #12474, #92944, #77340, #48917, #77818, #28104, #56520, #12967, #7240, #26685, #85829, #85379, #5393, #63634, #20528, #6313, #42273, #71184, #35181, #20980, #64105, #49847, #71656, #35665, #64580, #93405, #28557, #34910, #14998, #6507, #21637, #78930, #65218, #78474, #42945, #6038, #93587, #56230, #92655, #93130, #7420, #7876, #64305, #35845, #14080, #86472, #72755, #58107, #28285, #43857, #43405, #27826, #36766, #86953, #50516, #78015, #85092, #71374, #29207, #71852, #49118, #20241, #6972, #86016, #22105, #64762, #79414, #13155, #28746, #50975, #41991, #35386, #79859, #92188, #21166, #57629, #70904, #14549, #72300, #36302, #85561, #323, #56715, #57176, #63821, #20709, #42464, #27343, #49579, #13611, #50035, #54122, #54581, #30134, #1252, #15935, #83453, #23497, #37232, #90540, #25699, #11505, #44326, #44789, #47472, #32817, #87405, #59018, #66587, #58564, #65687, #82993, #81240, #1708, #18143, #75900, #22552, #8349, #52365, #73690, #15455, #18607, #87865, #80315, #67052, #51426, #23014, #51893, #3464, #30591, #80786, #61707, #76379, #32359, #59493, #801, #66137, #8800, #74142, #73238, #88346, #37679, #61259, #9260, #16387, #45237, #46997, #38137, #90094, #25246, #11024, #29681, #39893, #68814, #3944, #13394, #26652, #83934, #92911, #12936, #69271, #49816, #41776, #34228, #55065, #19540, #70686, #4400, #20495, #77788, #63134, #11970, #33279, #47940, #41292, #55542, #84857, #19086, #84391, #4869, #5816, #27592, #78713, #35150, #20009, #64071, #40818, #70227, #69737, #56488, #85797, #33751, #20948, #34690, #42237, #48406, #62174, #77309, #91963, #62663, #48887, #71150, #6279, #49362, #91497, #85347, #78256, #5362, #28073, #56960, #40354, #27118, #56002, #91006, #12444, #63604, #92428, #26174, #76843, #57419, #13855, #1039, #66370, #73471, #1488, #65004, #64550, #52144, #51209, #28524, #57873, #7212, #37461, #71626, #28985, #93374, #37013, #73001, #6759, #58348, #80552, #72540, #42710, #35633, #14789, #72095, #86258, #21409, #106, #43644, #79647, #80100, #86727, #7659, #22796, #87189, #15239, #50284, #29917, #44568, #79190, #36544, #36085, #58801, #44095, #14334, #43194, #21891, #8129, #30371, #50763, #65460, #576, #22338, #29460, #65927, #87646, #8583, #51663, #88110, #15707, #59262, #23266, #45962, #32233, #17096, #38850, #75783, #2432, #17572, #82874, #67304, #73920, #31312, #67758, #16625, #60661, #18027, #46881, #61141, #74378, #89977, #25131, #74869, #54007, #10903, #25582, #2884, #31769, #81024, #45479, #82422, #89036, #10439, #39305, #30849, #16168, #68222, #39771, #68695, #3826, #38394, #37915, #45020, #24663, #1956, #60198, #9506, #32707, #9037, #24186, #66819, #3342, #46421, #59742, #89498, #61593, #9979, #88584, #23732, #81939, #53064, #52595, #81476, #53549, #75322, #90426, #27003, #11850, #84277, #63488, #5244, #91849, #11388, #41661, #85230, #90887, #19428, #18969, #5703, #55891, #83335, #62052, #76260, #84745, #42121, #92794, #33628, #26050, #63017, #91379, #26536, #47344, #20380, #19892, #35040, #77193, #48763, #18481, #48290, #34579, #12322, #41166, #49251, #69620, #77669, #12821, #70104, #69155, #62538, #70578, #40240, #92319, #27473, #34115, #54937, #4283, #83816, #55424, #4748, #56366, #33161, #78146, #47822, #13284, #71038, #63954, #6172, #54465, #76724, #40700, #28878, #28418, #43991, #73365, #57309, #8478, #22234, #21782, #42596, #7106, #461, #56851, #8012, #65354, #50657, #93264, #20838, #35524, #57766, #43083, #72436, #6645, #71988, #86151, #58241, #15128, #37357, #22682, #7554, #51555, #21302, #86612, #50175, #72888, #66264, #79071, #27961, #51105, #29810, #14223, #49708, #35977, #79544, #64897, #36439 ),
 ( #78604, #85692, #29350, #71511, #14442, #14684, #80443, #13748, #43539, #64438, #79991, #87085, #36906, #65823, #931, #58691, #87534, #15588, #44461, #59634, #16063, #30261, #52493, #31208, #67193, #67654, #81370, #60093, #10332, #45849, #38750, #52034, #82313, #32127, #37810, #88932, #88480, #46313, #2780, #59153, #8932, #23150, #31661, #82769, #39659, #74273, #66717, #9874, #38280, #2328, #87997, #61023, #60553, #75673, #24081, #89391, #80918, #52956, #75218, #81834, #16984, #89869, #16519, #24545, #53429, #74755, #39199, #25029, #1379, #17463, #68111, #44917, #23627, #3237, #9396, #53901, #17921, #73819, #1845, #46772, #10798, #30732, #45370, #25939, #25479, #13170, #12210, #83232, #18861, #61943, #92203, #32603, #83699, #54358, #91739, #33999, #61493, #19316, #41541, #33513, #68582, #3718, #69508, #33053, #18378, #90325, #54821, #4639, #40594, #41055, #47718, #62419, #77550, #48178, #69981, #47236, #55778, #5593, #11281, #91261, #90780, #19779, #5122, #76148, #40134, #69051, #62902, #56247, #4180, #76618, #11741, #77079, #26425, #55317, #84168, #34467, #26891, #49134, #84631, #48650, #12701, #70465, #63373, #27359, #85108, #20258, #78030, #72316, #14564, #35861, #56731, #21181, #43421, #70922, #22119, #79428, #64778, #13628, #34925, #49594, #42961, #57191, #86491, #20724, #86032, #6523, #7437, #29225, #51440, #36782, #21654, #65703, #42479, #71867, #71391, #58121, #87418, #35401, #22566, #36319, #43872, #28301, #63839, #50052, #93603, #64321, #50531, #72769, #7893, #50988, #93146, #86966, #79873, #78947, #65233, #78490, #14097, #6988, #338, #15013, #80328, #815, #29695, #58579, #28761, #57644, #42006, #6053, #92670, #27842, #85576, #9759, #17345, #1721, #8364, #30607, #67069, #44802, #88815, #46196, #75101, #89273, #8812, #60437, #24423, #45251, #53305, #10211, #53785, #2204, #31088, #15470, #73703, #16863, #23509, #38634, #67537, #59030, #44341, #2666, #67993, #39079, #3121, #66599, #66148, #73252, #52837, #30147, #59509, #37693, #32001, #37245, #88359, #1265, #31545, #74631, #87877, #59976, #82191, #74156, #23028, #51907, #16400, #52378, #80799, #15947, #81255, #9272, #38154, #81713, #23963, #45721, #60897, #89746, #24907, #39539, #69861, #19663, #25362, #47599, #47116, #33881, #84054, #17802, #90213, #10681, #55199, #70355, #27245, #61828, #54242, #91136, #25821, #54701, #75559, #48531, #26304, #63258, #11625, #76965, #46655, #76501, #62790, #18740, #40471, #77432, #4066, #19201, #48061, #69388, #3594, #90661, #12094, #68460, #91625, #40941, #4521, #83112, #32483, #18263, #83577, #12575, #4998, #61380, #76028, #33397, #41423, #62296, #11157, #40018, #26778, #55664, #5481, #84516, #34353, #68935, #92089, #82653, #32936, #64208, #86862, #7786, #49944, #42843, #20139, #21536, #43318, #79323, #49488, #58007, #85471, #57083, #77919, #27722, #6406, #50418, #49022, #56620, #22017, #72214, #43766, #20618, #78378, #35280, #72667, #13983, #13519, #79768, #14911, #707, #34815, #93038, #36672, #50887, #13061, #42367, #85922, #41897, #56132, #7330, #71759, #21073, #36210, #65129, #70811, #92553, #6884, #28194, #5943, #65593, #71279, #63728, #57542, #78837, #35757, #64670, #86385, #93498, #28651, #84985, #14461, #231, #29111, #46094, #30044, #58925, #38045, #15364, #30501, #87775, #88711, #66954, #51335, #1617, #9646, #2093, #22925, #30983, #66049, #74999, #37588, #52725, #16296, #2562, #15841, #73134, #82074, #59871, #58470, #38978, #74048, #37141, #23859, #87314, #51795, #59395, #38532, #67890, #88248, #81608, #45149, #16757, #10111, #89168, #23406, #29591, #74513, #80686, #22461, #24319, #44698, #45611, #67435, #52273, #44225, #8710, #31441, #80228, #60331, #53196, #81152, #1161, #8260, #73599, #9167, #66499, #17232, #75453, #18157, #61272, #33291, #83949, #12458, #91512, #76396, #26668, #68352, #3958, #3480, #19101, #48420, #32372, #77326, #91018, #4882, #83005, #89629, #47011, #54595, #90107, #11519, #33766, #62678, #76857, #25259, #47954, #11983, #32831, #40832, #55558, #41306, #83466, #18622, #3013, #54136, #4413, #11039, #26187, #55080, #46552, #31899, #69751, #84406, #19555, #60791, #75914, #53683, #24798, #40366, #17700, #39908, #68829, #82551, #10572, #61722, #39436, #90553, #62188, #25712, #47487, #69283, #35166, #16081, #70243, #71169, #34706, #84873, #5376, #27607, #6297, #42255, #44007, #56505, #64088, #80459, #22251, #15146, #27133, #58708, #8494, #12953, #92928, #63619, #22698, #72905, #34243, #77803, #91980, #8029, #59169, #63149, #49380, #41791, #80007, #13412, #28089, #56016, #37372, #36926, #52053, #58258, #65840, #20024, #87101, #51573, #51121, #948, #48901, #70702, #5833, #29826, #88015, #92444, #78273, #85363, #87551, #15607, #44479, #20512, #66282, #73384, #80936, #1395, #30279, #23170, #52976, #46332, #24097, #17001, #61043, #38299, #60573, #2797, #81851, #1861, #2347, #31679, #73835, #75235, #89409, #45869, #52511, #8949, #88498, #88950, #67214, #9892, #59654, #31225, #45388, #24563, #82331, #17938, #89886, #38767, #32144, #81387, #74775, #16535, #17481, #82786, #74289, #46789, #53450, #68130, #60110, #37828, #67671, #10349, #9413, #39215, #3254, #25046, #53918, #44934, #66734, #30752, #23645, #15922, #30579, #74126, #87393, #51412, #35831, #310, #37218, #43841, #59004, #87853, #79400, #64746, #23001, #88331, #1696, #23484, #86940, #86458, #93573, #73223, #50501, #79845, #29191, #59475, #28730, #50962, #21617, #51878, #1239, #57615, #80304, #8788, #785, #14536, #43391, #36750, #58089, #72285, #7406, #22092, #65673, #7863, #8337, #14985, #29668, #44777, #15444, #66125, #36287, #80772, #66574, #65206, #58548, #72742, #73677, #30121, #52351, #22540, #81227, #37666, #44311, #16373, #45224, #61354, #88788, #2174, #82160, #39991, #53761, #59948, #67037, #82627, #3091, #68907, #24880, #90188, #31061, #17775, #4039, #23936, #17318, #32911, #54675, #31976, #89713, #52808, #68432, #25336, #32452, #2642, #11125, #38608, #10185, #81686, #74601, #53276, #3563, #16835, #9731, #61800, #54215, #90631, #67512, #31520, #46170, #25793, #60869, #60408, #83548, #18707, #47571, #45692, #75073, #9247, #38125, #89246, #24399, #39054, #67966, #46630, #83084, #75530, #10654, #18239, #47091, #39511, #75995, #63230, #55637, #26272, #28169, #4969, #91104, #77890, #62269, #12066, #33853, #13035, #12542, #40913, #42340, #71252, #41870, #70326, #93011, #76938, #69833, #84958, #55167, #77405, #62763, #70783, #20109, #4492, #48505, #56590, #48989, #91596, #5916, #19175, #57059, #84488, #34786, #92062, #49463, #26751, #84030, #35253, #63701, #11596, #85895, #27216, #48033, #92527, #40444, #19636, #41392, #85444, #21047, #5456, #27693, #56103, #20593, #76476, #78351, #13493, #69361, #6381, #34324, #33368, #64178, #79290, #66470, #15812, #8233, #35730, #42813, #29084, #80657, #677, #6855, #13956, #29561, #43738, #44670, #65564, #37111, #71728, #58442, #73571, #64643, #57975, #8680, #1587, #72638, #36643, #93471, #15338, #66020, #73105, #43289, #51767, #14432, #50860, #28624, #21509, #201, #44199, #57513, #50387, #37558, #1132, #30469, #72186, #7302, #86828, #59365, #7758, #36182, #88217, #49915, #78810, #86358, #21986, #65101, #79742, #14884, #87288, #22434, #51307, #80199, #30014, #58898, #87744, #22896, #32340, #16266, #59839, #10080, #2532, #66923 ),
 ( #3445, #31868, #23829, #89598, #88680, #39874, #31410, #46522, #38948, #90076, #9612, #2061, #75880, #24769, #52241, #32800, #67858, #30951, #53651, #81123, #52692, #24287, #61241, #61689, #89136, #60757, #82521, #45116, #25228, #17669, #46062, #81573, #74018, #16721, #53162, #38499, #2983, #45576, #67404, #74481, #75423, #10540, #23373, #18126, #39406, #46979, #60299, #82044, #17201, #68321, #68794, #74967, #3924, #54101, #82973, #11005, #9135, #38012, #48388, #26153, #70210, #27570, #56467, #70668, #83915, #41756, #5797, #26633, #63585, #20477, #35130, #77291, #12421, #90520, #55047, #91943, #4848, #19987, #48864, #40337, #54563, #77769, #49344, #78238, #13376, #47922, #47453, #83431, #34210, #11487, #40800, #19067, #42218, #18587, #11951, #76361, #12917, #55984, #69253, #41272, #92410, #55523, #4381, #33259, #91482, #76825, #62156, #90985, #69717, #84372, #62644, #63115, #33732, #19521, #71132, #5343, #27097, #84838, #6261, #1025, #6743, #28970, #28507, #15225, #65444, #92895, #71608, #85781, #36528, #51650, #8569, #43177, #35616, #72524, #7195, #36070, #56944, #29903, #7644, #44555, #86709, #58332, #28054, #57855, #44081, #90, #21874, #58787, #79170, #559, #29443, #50748, #78697, #72079, #64987, #87175, #22324, #13838, #64052, #51195, #22781, #87631, #80536, #21392, #20931, #49800, #80082, #42689, #14317, #57399, #15690, #64531, #79632, #93356, #72983, #8113, #86241, #14774, #37000, #43627, #50262, #65912, #73458, #1938, #52130, #66357, #88572, #67291, #9490, #9967, #23720, #2420, #46409, #81927, #74855, #88093, #24646, #68211, #73908, #31300, #30833, #82410, #38839, #1472, #45006, #59247, #67746, #25120, #75772, #16612, #9024, #45947, #74367, #38377, #30358, #3330, #2872, #18015, #60186, #31756, #23251, #89024, #17557, #24171, #53052, #32220, #52583, #60648, #89486, #17079, #81011, #45467, #53534, #16155, #75309, #10428, #39292, #37903, #66808, #59730, #61127, #81463, #89966, #53994, #82863, #46868, #37448, #91834, #20363, #5689, #84264, #34563, #76245, #11836, #11377, #26988, #56350, #40227, #85212, #5229, #12805, #90873, #3815, #26037, #62521, #69143, #19414, #41647, #63472, #84730, #4271, #55878, #19879, #40687, #48750, #92301, #49235, #91362, #26523, #10892, #33149, #12309, #62039, #27458, #68681, #54920, #61582, #34102, #70086, #32696, #55411, #77654, #69605, #39755, #90414, #4735, #83800, #25571, #54451, #18955, #33613, #76710, #77179, #47809, #48277, #83324, #41153, #63004, #18470, #47329, #15113, #20824, #43067, #42581, #29331, #79530, #13269, #85676, #6153, #50640, #65805, #22667, #57294, #49694, #86595, #21285, #50158, #71021, #43972, #21765, #58676, #7090, #72422, #42106, #71972, #58224, #14207, #35962, #72873, #93249, #14669, #43524, #64881, #92777, #86136, #7538, #35025, #87069, #36423, #93707, #78589, #63939, #13728, #79056, #28402, #28862, #56836, #57749, #71496, #65340, #445, #87521, #7997, #22217, #36890, #6627, #51087, #35507, #79975, #29796, #64423, #78131, #917, #27945, #37795, #44445, #66702, #9382, #80902, #31194, #82297, #17447, #31647, #44901, #2765, #60537, #81354, #89375, #46297, #89853, #38264, #67177, #51540, #16049, #52942, #59615, #74738, #9859, #1364, #80429, #38733, #10316, #75201, #39184, #8918, #8463, #15575, #88916, #66249, #1830, #24531, #16504, #73351, #37343, #52480, #73804, #30247, #59137, #30717, #45356, #23613, #24066, #88466, #74258, #53413, #2310, #81819, #87981, #67639, #68096, #23133, #60079, #16968, #3221, #45834, #52016, #32111, #61008, #91246, #12684, #63357, #4165, #32588, #33496, #61927, #90764, #17904, #84615, #62404, #5578, #47703, #19301, #53885, #83684, #69965, #54806, #76602, #19764, #40119, #55300, #26410, #18845, #39643, #33037, #84153, #82752, #5106, #48161, #11725, #90309, #46758, #61479, #25923, #69035, #69492, #3703, #40578, #83217, #77064, #12194, #34449, #48632, #4623, #77534, #25462, #41037, #54342, #33984, #70451, #18362, #25014, #62887, #26875, #11266, #75658, #91722, #55762, #47222, #41525, #10782, #68567, #76132, #18546, #70171, #34175, #55007, #5305, #19953, #63547, #76788, #40763, #25191, #83396, #26596, #33222, #48352, #77255, #68757, #54064, #12385, #77731, #84803, #12881, #76323, #75843, #82935, #62603, #39834, #69216, #47414, #48824, #18087, #40301, #10966, #41231, #84335, #46941, #69681, #90486, #3888, #32765, #26113, #4345, #4811, #61653, #62118, #11449, #55486, #63077, #34637, #41719, #33692, #70635, #25644, #83879, #54527, #91907, #5763, #90949, #19030, #19486, #27061, #47884, #11914, #91445, #55948, #28019, #72049, #29411, #58301, #72495, #85750, #43599, #7611, #28476, #36499, #87145, #36969, #50233, #14285, #92376, #56910, #58, #6710, #21841, #50717, #42182, #27535, #79603, #51166, #22295, #80053, #49769, #49308, #56428, #36040, #13341, #42657, #20897, #15193, #85290, #13805, #78202, #14744, #57825, #20439, #43145, #65416, #57369, #71095, #6228, #93324, #78664, #35098, #64016, #71574, #86211, #64498, #64957, #35583, #21363, #526, #7165, #28939, #92856, #44053, #72954, #79136, #86676, #8081, #17050, #67259, #991, #73429, #87599, #38346, #53502, #10397, #44977, #8539, #74337, #8996, #37874, #58757, #31727, #9460, #46378, #88542, #60156, #29873, #30800, #45916, #1910, #23691, #60618, #80983, #2391, #31269, #59699, #80507, #73878, #88995, #22745, #74822, #24142, #52555, #89456, #16126, #53020, #81898, #81431, #15655, #66780, #9937, #51620, #38811, #67715, #16580, #37418, #44525, #66329, #45436, #2845, #24616, #1442, #82378, #30327, #17528, #75278, #65882, #59217, #88062, #23219, #52099, #40198, #39725, #55383, #84704, #68649, #19851, #33583, #41126, #25542, #32189, #54423, #90844, #3783, #18925, #70057, #5199, #19385, #32666, #84235, #48249, #69115, #77151, #34072, #77625, #26006, #54890, #39262, #61553, #40657, #47298, #62491, #91331, #82831, #68177, #26493, #91808, #62974, #26960, #90387, #89934, #3299, #76681, #53964, #83294, #18441, #55851, #61095, #76215, #25090, #12281, #4705, #17984, #83769, #48723, #4240, #46836, #75738, #33120, #11344, #10863, #62009, #47779, #11806, #69576, #79025, #63913, #42551, #21736, #57264, #50126, #63443, #93678, #43496, #49204, #71468, #70993, #57720, #14178, #41616, #20334, #34535, #43040, #415, #51058, #85647, #78100, #21256, #49666, #78561, #5660, #72392, #71942, #87040, #35477, #7063, #70537, #6599, #86567, #64394, #93220, #86107, #7509, #36394, #50612, #6125, #79502, #14638, #28373, #65307, #29301, #12774, #35933, #64851, #92274, #34996, #28836, #20795, #58196, #22190, #56321, #27430, #85185, #13241, #42077, #92747, #27918, #56805, #13699, #23587, #887, #30219, #73325, #9834, #43944, #1337, #36862, #9351, #45331, #72841, #30688, #52914, #44874, #24504, #79946, #80876, #44417, #29770, #15084, #37315, #16023, #51986, #52454, #66223, #73776, #88890, #59587, #81328, #65778, #67149, #16941, #22640, #8891, #8436, #31166, #16475, #7969, #87490, #58648, #74232, #67614, #51512, #59110, #80400, #88438, #23105, #37769, #15546, #45804, #38236, #60513, #66674, #2283, #87952, #1802, #60052, #24038, #81793, #74713, #38707, #2742, #31622, #89348, #68071, #32564, #25897, #82270, #33472, #90739, #76108, #24989, #46272, #60981, #54316, #68539, #4142, #32080, #3678, #17880, #83657, #40552, #62865, #48137, #33013, #77040, #53862, #83191 ),
 ( #54779, #33961, #11240, #47677, #17423, #18339, #4599, #47194, #40095, #12171, #61456, #18820, #76578, #69011, #3196, #90287, #11701, #75176, #62375, #69467, #61904, #82728, #10289, #89828, #91219, #25438, #26386, #46732, #55274, #75635, #84129, #19279, #91698, #41014, #69937, #5080, #10758, #53386, #39615, #39159, #72278, #56207, #7397, #21144, #28722, #13134, #19740, #41970, #78453, #85066, #6482, #57607, #86450, #6950, #20218, #71831, #35823, #56693, #64737, #21608, #65199, #13589, #42441, #26850, #49095, #28265, #34889, #50014, #78907, #70430, #55738, #14054, #79391, #50490, #14528, #77994, #77508, #84590, #64281, #41501, #70883, #6014, #43383, #48608, #63800, #12656, #42918, #85994, #5556, #71351, #93565, #85540, #34426, #63333, #27801, #92629, #92164, #27321, #20688, #49558, #35360, #93110, #57154, #36279, #9239, #44769, #37658, #50954, #81220, #32322, #36742, #58996, #58541, #45217, #1688, #59467, #16366, #23476, #87386, #2165, #29661, #1231, #22084, #65664, #44302, #88321, #58079, #777, #61224, #74119, #82954, #22533, #51405, #73211, #18109, #51869, #80297, #25211, #54084, #39856, #72735, #8328, #75863, #90058, #79837, #15436, #30113, #86931, #302, #38118, #15913, #87844, #67028, #46961, #14977, #37210, #80762, #66117, #43833, #10986, #22994, #7855, #30569, #73669, #8780, #66566, #52343, #29182, #33242, #34653, #63567, #34193, #62625, #85310, #69235, #4364, #77274, #54546, #69700, #62137, #63097, #12403, #90504, #40782, #48844, #41251, #90968, #70192, #11469, #20458, #76807, #91925, #55506, #41738, #55029, #18568, #27553, #5325, #3907, #78220, #19504, #76343, #27080, #32784, #26134, #4829, #77749, #13359, #33713, #55967, #84355, #84820, #49326, #92393, #91464, #68778, #19969, #83898, #61672, #56448, #12900, #83414, #25665, #47905, #5779, #48372, #47434, #40320, #70651, #26615, #19049, #11933, #541, #64033, #21857, #72966, #6244, #50246, #8095, #87612, #36053, #28952, #35113, #78680, #7178, #6726, #87158, #43611, #71114, #49783, #92875, #14757, #29886, #80519, #21376, #13820, #50731, #79152, #14300, #28037, #36982, #79615, #22762, #64971, #36512, #56926, #74, #22307, #72061, #57838, #65894, #57383, #72507, #7627, #86692, #85764, #43160, #65427, #20914, #51178, #29424, #58314, #42672, #71589, #35598, #80065, #86226, #15208, #64513, #44065, #93339, #1006, #58770, #51633, #42200, #28490, #10412, #80996, #16595, #16138, #31739, #61110, #44990, #89949, #9951, #17541, #1922, #8552, #30816, #67274, #73891, #89008, #46393, #75293, #89469, #9008, #60632, #24630, #45451, #53517, #39276, #53978, #2404, #31284, #15672, #37887, #17063, #23704, #38823, #67730, #59231, #44539, #2857, #68194, #3314, #32203, #66792, #66341, #73442, #53035, #30341, #59713, #88556, #25104, #37432, #52567, #1455, #82393, #74838, #88077, #60170, #23233, #74351, #52113, #81447, #9474, #38360, #24155, #81911, #45930, #18938, #54905, #55396, #40212, #47793, #91820, #33598, #26506, #39739, #70072, #19865, #76695, #83784, #84248, #69128, #11821, #26973, #62506, #19399, #68663, #5213, #48735, #25556, #40672, #47313, #34086, #48262, #17999, #90399, #10876, #77164, #70550, #27443, #62024, #54436, #91346, #26022, #69590, #75755, #77639, #12294, #63456, #4720, #41139, #46852, #62989, #55864, #84716, #12790, #41630, #4256, #5673, #34548, #92286, #3799, #90858, #82847, #32680, #61566, #83309, #18454, #76229, #11359, #33134, #57279, #71480, #7075, #35009, #6612, #20808, #86580, #43510, #65792, #51074, #35948, #79962, #27929, #86121, #56819, #72408, #7983, #85661, #36877, #50626, #58210, #42564, #49219, #35492, #14192, #49679, #64867, #87055, #22204, #36409, #78574, #7524, #65324, #21270, #429, #15099, #902, #43053, #71957, #56335, #13712, #57735, #64407, #79516, #14654, #6137, #85197, #29317, #43959, #72858, #20347, #93234, #13254, #78115, #93693, #71006, #28387, #50142, #42091, #63924, #79040, #92762, #28849, #21750, #87507, #74245, #2754, #88452, #68084, #29784, #30703, #87968, #44432, #58663, #80888, #22654, #23119, #31180, #37782, #52927, #81806, #73338, #51527, #16955, #82285, #89361, #17436, #16036, #80416, #15561, #67164, #8449, #73789, #52002, #53400, #37328, #44887, #66236, #45820, #88903, #1351, #9367, #31635, #23599, #30234, #59124, #59602, #8905, #66689, #1817, #52467, #81341, #16489, #2297, #45344, #38251, #38720, #60065, #24053, #74726, #9847, #60525, #67626, #24519, #46286, #75190, #10303, #39173, #10771, #25004, #69480, #84603, #41515, #76121, #39631, #11713, #40108, #69023, #89842, #62876, #40566, #77521, #25910, #91234, #32095, #61916, #48149, #33025, #54793, #91710, #18352, #33485, #4611, #90752, #17894, #11253, #62391, #60997, #77053, #26399, #83672, #68555, #53875, #3692, #4155, #47210, #47689, #75648, #18834, #61470, #55287, #84141, #12673, #26862, #76591, #55750, #32577, #19290, #90300, #12182, #48620, #25452, #3209, #41025, #5093, #83205, #82741, #69951, #33972, #54331, #19753, #46747, #7409, #50504, #63811, #21622, #79402, #6494, #14538, #65208, #14987, #28276, #86006, #70441, #49569, #78005, #78918, #13600, #42452, #63345, #36289, #14067, #50964, #93120, #64750, #5568, #35375, #43393, #64294, #57166, #312, #85552, #6961, #42932, #21155, #85080, #78464, #71841, #34439, #72287, #35834, #50025, #41981, #92177, #13145, #71364, #20699, #93576, #49108, #28734, #34900, #57618, #86461, #79847, #29195, #58092, #86942, #70894, #22094, #6026, #27333, #56220, #92643, #20231, #27815, #56705, #30124, #36754, #59007, #1698, #73227, #23487, #74606, #9735, #23939, #37220, #88791, #52811, #73679, #81690, #38612, #82165, #30581, #59482, #43845, #8339, #45227, #51882, #67041, #2178, #87395, #72744, #31064, #2645, #67515, #31523, #1242, #788, #7865, #81230, #58551, #87855, #66127, #60411, #65676, #23004, #29670, #59952, #9250, #22542, #88335, #16839, #8790, #51415, #80307, #44779, #80775, #15446, #44315, #15925, #37669, #66577, #16377, #52354, #74131, #45695, #38128, #89250, #24402, #53281, #48038, #53764, #75999, #75534, #62273, #18712, #46173, #24883, #39057, #83553, #4972, #69838, #47575, #75077, #26756, #61804, #82630, #76480, #10188, #17779, #18242, #26277, #55641, #83088, #54679, #32914, #11603, #91600, #76943, #47094, #62768, #91108, #46633, #33858, #12070, #69366, #3095, #67969, #90191, #40917, #90636, #31979, #60872, #25798, #11130, #17322, #40448, #4496, #89719, #33374, #10658, #39514, #25339, #68435, #3567, #39994, #4044, #32457, #55172, #84033, #19178, #61357, #54219, #68913, #85449, #12547, #56108, #34791, #49920, #48508, #84962, #50394, #71735, #72193, #48995, #20113, #63706, #7310, #42346, #77894, #14439, #43296, #29091, #63236, #92531, #65108, #79299, #41397, #13038, #20597, #77409, #84494, #6861, #6386, #49467, #35736, #93478, #70331, #27221, #71257, #27697, #34330, #36189, #41875, #5460, #85901, #92067, #70786, #5921, #21053, #78357, #56595, #210, #19640, #78816, #13497, #35257, #64183, #93015, #28173, #57063, #13962, #42820, #64649, #28631, #57520, #86364, #21516, #66479, #58450, #30478, #686, #74491, #66029, #81132, #44678, #30961, #44206, #7766, #1141, #16276, #73580, #59849, #73113, #36651, #16733, #59374, #86837, #67414, #8689, #65572, #88226, #21994, #87295, #58906, #66932, #2543, #30023, #1596, #37568, #52251, #38510, #23838, #87752, #9623, #9145 ),
 ( #50867, #23382, #45127, #74028, #51314, #88690, #22441, #22904, #79749, #29570, #8240, #38022, #14891, #80206, #52704, #2070, #45587, #15345, #37120, #51776, #57984, #15821, #80665, #81585, #43745, #72645, #10090, #75434, #11963, #90997, #53175, #24779, #32352, #24298, #69728, #18599, #46990, #61251, #47465, #40347, #82054, #67870, #18136, #10552, #74978, #76836, #53662, #46072, #32810, #17211, #60768, #82531, #61700, #90087, #89609, #26166, #55058, #90532, #25239, #47933, #31879, #17680, #39886, #38958, #54113, #46532, #25692, #68807, #2993, #3457, #11498, #3936, #39417, #54574, #68334, #40811, #83927, #31422, #82986, #75891, #60311, #19079, #11016, #83445, #76372, #69264, #89149, #4393, #33270, #62167, #42229, #35140, #62656, #77302, #34682, #55994, #84384, #43974, #34220, #19533, #85337, #55535, #41283, #63126, #20488, #77780, #70219, #58226, #87071, #49354, #41768, #15115, #12433, #5354, #27581, #48399, #48876, #91955, #78248, #56478, #91490, #12927, #6272, #13386, #27110, #71143, #84849, #72875, #19998, #64063, #5808, #92904, #70678, #63596, #51089, #28064, #33743, #7999, #92420, #22219, #79977, #26645, #4860, #90371, #4687, #6457, #61539, #33102, #11329, #83753, #70034, #55364, #25527, #41104, #40639, #25075, #12260, #84216, #47764, #75265, #82363, #68633, #26475, #40180, #46364, #53487, #69099, #83279, #19364, #4226, #76662, #17512, #61992, #48228, #10380, #3766, #77130, #35332, #18423, #76200, #39247, #54872, #11789, #18909, #82816, #91313, #53948, #54406, #68163, #61077, #39709, #69558, #3283, #89919, #89440, #33561, #24598, #17967, #46820, #32651, #32176, #47283, #75722, #10845, #62471, #90827, #25987, #1211, #28242, #72259, #30093, #15893, #58058, #50933, #57129, #29641, #51385, #87364, #57585, #66099, #93541, #65177, #85971, #35801, #14507, #58520, #21121, #64714, #58976, #80276, #51848, #28700, #86429, #43363, #80742, #22065, #21586, #87825, #22976, #8761, #42892, #7376, #44750, #73651, #49989, #50467, #282, #78884, #64258, #15415, #79817, #29161, #44282, #73190, #14031, #6928, #14958, #36257, #71806, #93088, #79370, #86910, #65642, #43813, #72713, #7836, #756, #36723, #22514, #8309, #37192, #3065, #31493, #54187, #38100, #67009, #46145, #23457, #38581, #2145, #31950, #75049, #59448, #9700, #17749, #10160, #31034, #39029, #74100, #83057, #45664, #60843, #24371, #10626, #23909, #81201, #90161, #67942, #66547, #47061, #82131, #45197, #89685, #1668, #59924, #67484, #46602, #75966, #2615, #24852, #53250, #53736, #18211, #3534, #60381, #37639, #82602, #88763, #30551, #32424, #75504, #52324, #88300, #16807, #68406, #17288, #16347, #9219, #39484, #89220, #61323, #25309, #52780, #81659, #74571, #19148, #34293, #91564, #77855, #91073, #54646, #63671, #77375, #39961, #20562, #55608, #18676, #12513, #68877, #11567, #12038, #20078, #49434, #76908, #48475, #26721, #5428, #85414, #70752, #40885, #56560, #56073, #40415, #27663, #5886, #63201, #90603, #4007, #84000, #41841, #84457, #61770, #32882, #19607, #4939, #34756, #41363, #92031, #25764, #70297, #92494, #83520, #48004, #11095, #47542, #33824, #27186, #76446, #84926, #48957, #13005, #4464, #69333, #33341, #69803, #62238, #26243, #55136, #62734, #42312, #78781, #44162, #65527, #65987, #42780, #13922, #28593, #1098, #36149, #49883, #8197, #37078, #22860, #57027, #57483, #58863, #73068, #6348, #71696, #79258, #71221, #78322, #644, #169, #14399, #29528, #87254, #35221, #21016, #65070, #86324, #28138, #29979, #6825, #92980, #79711, #64147, #35699, #64613, #14853, #43258, #93439, #87710, #13461, #43706, #72156, #85865, #21476, #50354, #86795, #7272, #29048, #57941, #72605, #21954, #50827, #7727, #58408, #36608, #22400, #51272, #80165, #15303, #51726, #52657, #16231, #66431, #80619, #9099, #81537, #23793, #24251, #37976, #16685, #60722, #31373, #89099, #8644, #38911, #82484, #88177, #45540, #73982, #2945, #53125, #15774, #59325, #73535, #82005, #39368, #90039, #30914, #23336, #60262, #88645, #74441, #44633, #17631, #17162, #32298, #9573, #46027, #37521, #38460, #31831, #67366, #74930, #46483, #66884, #10041, #67820, #89561, #1551, #59804, #24731, #30434, #53613, #75386, #10499, #52205, #81087, #2022, #68284, #3406, #61203, #14267, #50698, #40, #65865, #22725, #44960, #30309, #15175, #59197, #7147, #36480, #36022, #51600, #80964, #64939, #16108, #29854, #37400, #21823, #28458, #79586, #87127, #28920, #44033, #66310, #1425, #15636, #57808, #80488, #44505, #65397, #73411, #88045, #73860, #22278, #51150, #35567, #86659, #36952, #43580, #58738, #87581, #79120, #64481, #8521, #23201, #52081, #93308, #14727, #86193, #21345, #72935, #50216, #72478, #7594, #43127, #72032, #510, #29392, #58284, #973, #80034, #8061, #8978, #68507, #11671, #18308, #33442, #62345, #53834, #39128, #91185, #62836, #69907, #91669, #61426, #60945, #48578, #47646, #24958, #54286, #3642, #33927, #68040, #25407, #89794, #26353, #69438, #3166, #54747, #77012, #68981, #32051, #82700, #11205, #32533, #17851, #46702, #90258, #40063, #76074, #76548, #83156, #4111, #19250, #83625, #40520, #75604, #55244, #40986, #10728, #32983, #47165, #84101, #4568, #39584, #61874, #90705, #48108, #26822, #25866, #18787, #12140, #5046, #55709, #84560, #19707, #43357, #21115, #58052, #6451, #71799, #12621, #42410, #28693, #13560, #35326, #72253, #92599, #14025, #49983, #71321, #92134, #56663, #78877, #41467, #57579, #42886, #64252, #49064, #70398, #85034, #78422, #27769, #28236, #56176, #85512, #41941, #6921, #64708, #86903, #7370, #57123, #36251, #77961, #93081, #13103, #93535, #29155, #70853, #22058, #35795, #79364, #63770, #5526, #20658, #85964, #5985, #86424, #14500, #65169, #21579, #34857, #50461, #275, #77478, #34396, #63303, #27289, #20184, #49528, #74095, #16342, #14952, #1663, #23904, #15887, #89215, #50927, #51841, #15408, #65637, #79811, #8303, #80734, #22969, #23450, #37185, #44743, #59916, #30545, #88295, #7827, #38094, #81654, #87358, #73645, #44274, #2140, #52318, #43807, #58513, #72707, #81196, #38576, #36717, #30087, #22508, #59444, #87819, #8755, #750, #16802, #45192, #31488, #37634, #9214, #29634, #66542, #31029, #67004, #88758, #45658, #66093, #52775, #74566, #9695, #51379, #58971, #67479, #80270, #2608, #60376, #73184, #1205, #17283, #31945, #25303, #39478, #68871, #3060, #68398, #82596, #54638, #11561, #33814, #19141, #4001, #47996, #89680, #54181, #24847, #40409, #69795, #53730, #4928, #18670, #26236, #10620, #46140, #3528, #75958, #17743, #32876, #55129, #83994, #4456, #46597, #69327, #33334, #83051, #62231, #76900, #62726, #11089, #39955, #24366, #75496, #25757, #32418, #47536, #76440, #67937, #53244, #91062, #12030, #40877, #82126, #61317, #75043, #10155, #61764, #39022, #90155, #18203, #60836, #47055, #90597, #83512, #42770, #27178, #14393, #57477, #49876, #77367, #84449, #70744, #28585, #42305, #48467, #55601, #71214, #85407, #86318, #13454, #78774, #19599, #6341, #21470, #12503, #5878, #50346, #43252, #20555, #78315, #41355, #57020, #13915, #21009, #84918, #93433, #56065, #92486, #70287, #63193, #41833, #85856, #5420, #92023, #79252, #71689, #72150, #20068, #48949, #34748, #7266, #49425, #77847, #36143, #91556, #26713, #34285, #63663, #12995, #27653, #56552, #35212, #64140, #92973, #28131, #6819, #35693, #64607, #52199, #73976 ),
 ( #639, #30428, #73530, #86789, #37073, #45076, #8639, #65520, #37516, #7719, #81531, #73062, #88170, #51721, #37970, #51267, #14847, #23787, #66426, #163, #74435, #15769, #72599, #1545, #29042, #29523, #65982, #9093, #9566, #1093, #59319, #80611, #23329, #45534, #30908, #29974, #16679, #36603, #81081, #57933, #58403, #58858, #66878, #65062, #87704, #16225, #44628, #2015, #21948, #59798, #22855, #50821, #88639, #87249, #79705, #52651, #43700, #22395, #80160, #44155, #15298, #8192, #89093, #2490, #82929, #32291, #69210, #54058, #90480, #60256, #18081, #4339, #31367, #46476, #33216, #83873, #61196, #25185, #24245, #3881, #25638, #61647, #31825, #40294, #67814, #39362, #53119, #10035, #82478, #32759, #81999, #38905, #62112, #54521, #26107, #2939, #60716, #17625, #55000, #90033, #89555, #90943, #19024, #76781, #17155, #75380, #47878, #38454, #46021, #24723, #68278, #74924, #67360, #83390, #46935, #3400, #18540, #47407, #53607, #10493, #75837, #10960, #39827, #68751, #76317, #11443, #13335, #91439, #41225, #63071, #42176, #41713, #70164, #71567, #6703, #71089, #5756, #28470, #12378, #5299, #20433, #26590, #12875, #34169, #6222, #49301, #33686, #77724, #85744, #78196, #91901, #35091, #48346, #57363, #19947, #64010, #92368, #78658, #27055, #55480, #64492, #92849, #40757, #21356, #56422, #28013, #70629, #55941, #35577, #93318, #56904, #34630, #86205, #84797, #48818, #20891, #84329, #63541, #27529, #49763, #13799, #62595, #85283, #42650, #50226, #11908, #69675, #77249, #4806, #19479, #8532, #65875, #52093, #65409, #28932, #37868, #51612, #14277, #88536, #29865, #86669, #80500, #43138, #79596, #80046, #88056, #23685, #51159, #22738, #984, #73422, #59693, #44971, #15186, #30794, #30320, #14737, #1904, #73872, #37411, #64950, #72042, #58294, #16120, #58750, #36033, #7158, #87592, #72947, #8989, #15648, #66320, #51, #44518, #66773, #57818, #87137, #79130, #21834, #8074, #1435, #50709, #59210, #23213, #80977, #72488, #43592, #7604, #44046, #36492, #519, #29403, #22288, #36962, #53014, #18434, #39719, #40190, #17044, #81891, #2839, #69109, #10391, #24136, #76209, #11338, #90837, #31263, #31721, #33114, #47291, #74330, #45910, #53496, #45429, #52549, #68643, #68171, #82372, #3775, #61548, #9454, #88989, #39256, #60612, #2385, #4234, #74816, #67253, #53958, #38340, #9931, #38805, #16574, #3292, #46372, #83288, #32183, #10856, #60150, #61087, #62002, #67709, #89450, #81425, #24608, #75272, #89928, #17522, #17978, #32660, #75732, #25084, #54417, #82825, #46830, #90381, #25536, #70048, #85178, #83762, #26485, #85640, #13235, #13692, #84227, #55375, #5190, #42544, #77616, #91323, #49660, #78555, #64388, #4697, #34064, #6593, #20788, #47772, #19374, #26951, #18918, #25998, #42071, #41607, #55840, #70986, #34988, #76672, #62483, #12765, #62966, #69569, #71457, #48240, #40650, #27423, #11799, #77142, #12273, #56313, #84695, #41116, #35470, #54883, #20328, #19842, #33574, #91800, #48712, #34529, #70529, #5654, #63437, #49198, #92266, #78093, #6118, #63905, #92740, #27911, #56798, #35927, #16013, #7502, #22632, #79939, #66213, #79495, #43033, #51977, #65771, #28366, #8880, #43937, #7057, #880, #57257, #93672, #406, #8428, #37760, #65300, #36855, #15077, #87482, #73768, #59102, #29294, #44865, #44409, #28830, #93214, #87943, #51504, #79016, #86101, #72385, #30211, #72834, #50119, #14631, #71935, #80866, #29760, #21250, #14169, #7960, #64845, #58640, #57713, #86558, #58189, #37307, #21728, #87031, #80392, #15536, #73316, #50603, #23094, #22183, #43489, #1329, #36387, #51051, #32555, #24980, #52445, #59578, #45793, #3667, #17414, #23578, #30678, #46263, #60504, #61447, #82261, #53854, #88429, #75167, #90278, #81319, #74704, #25429, #18330, #89339, #53375, #16466, #32071, #82719, #89819, #60043, #68530, #2274, #67605, #45320, #38227, #16932, #60968, #74223, #67140, #54307, #17871, #83182, #31157, #88881, #9825, #47186, #24494, #24029, #76098, #11231, #66665, #9342, #38698, #1793, #52905, #81782, #2733, #31613, #10280, #39150, #46723, #68062, #3187, #75626, #10749, #39606, #76569, #26841, #19270, #83647, #86808, #62366, #54770, #41491, #25888, #69458, #91209, #70421, #69928, #4590, #6005, #34880, #5547, #33952, #57953, #40543, #33463, #48599, #18811, #41005, #26377, #34417, #77499, #61895, #12162, #20208, #12646, #55265, #63324, #11692, #21966, #48128, #92155, #55729, #13125, #27312, #47668, #40085, #56198, #180, #63791, #29061, #84120, #90729, #79722, #85057, #77031, #5070, #62856, #50839, #4133, #91689, #84581, #49086, #77984, #33004, #19731, #41961, #70874, #69002, #14864, #15786, #73080, #29540, #43717, #65998, #44645, #80630, #81099, #1110, #73546, #23805, #59337, #52216, #65541, #2035, #45552, #51283, #8655, #8211, #59815, #16242, #72616, #22412, #36619, #45092, #2506, #53137, #87721, #80176, #23348, #51737, #37533, #7738, #74452, #73994, #89110, #66443, #9111, #656, #1562, #88656, #30445, #88189, #9585, #29991, #37987, #66895, #30925, #58420, #22872, #52668, #87266, #81548, #16697, #38473, #15314, #44173, #37089, #67377, #58874, #31384, #60274, #24262, #46496, #18558, #69227, #91456, #76799, #61664, #11925, #53627, #82946, #82497, #4356, #33704, #17645, #62616, #76335, #83890, #68297, #74944, #3418, #39847, #75399, #90496, #19041, #47897, #62129, #10512, #33232, #90960, #18099, #26124, #40774, #26607, #68770, #3899, #82017, #39382, #83406, #90050, #11461, #69692, #32313, #38924, #17175, #25655, #2958, #61216, #25203, #4821, #46039, #54076, #67833, #40312, #47425, #10054, #32776, #55020, #46953, #31844, #60733, #75855, #10977, #89573, #24745, #54538, #85301, #27545, #28030, #12892, #20450, #64507, #6238, #92867, #12395, #42666, #86219, #91917, #49317, #19962, #6719, #56919, #84347, #63089, #77266, #85758, #43154, #66, #34646, #27072, #64026, #92385, #56437, #48362, #21370, #20908, #36047, #78212, #49777, #19496, #13351, #35592, #42192, #71104, #50240, #70644, #78672, #13814, #35107, #70183, #63557, #71582, #41241, #93333, #28484, #57378, #55958, #5317, #84812, #79145, #5772, #14294, #34185, #72056, #48835, #7173, #64965, #55498, #77741, #41730, #23697, #534, #29880, #29419, #44984, #74344, #58309, #9468, #23226, #30808, #15200, #21850, #44060, #80513, #87152, #8545, #59707, #88550, #9002, #22302, #73885, #37880, #58764, #66786, #52561, #67267, #15664, #44532, #28946, #51173, #30333, #36977, #52107, #80990, #72502, #57832, #16132, #81440, #16588, #80060, #1916, #45443, #87606, #38353, #86684, #50725, #73435, #37425, #79610, #72961, #59224, #65889, #14751, #43606, #7620, #36507, #65422, #8089, #1001, #22752, #51627, #66335, #1448, #88070, #17058, #46387, #89464, #26017, #60163, #17536, #53028, #25551, #61561, #89002, #46846, #69123, #61103, #40667, #2398, #3308, #60626, #45923, #31278, #53510, #32197, #68187, #68656, #82388, #89942, #11354, #75747, #39733, #81905, #83303, #33129, #38818, #25099, #24625, #47308, #3792, #24149, #9946, #74833, #32674, #83778, #67724, #75286, #2853, #10870, #39270, #53972, #31735, #62018, #90393, #76690, #82840, #54430, #10406, #17992, #76223, #18449, #40207, #90852, #4250, #54900, #18933, #47788, #11815, #48730, #42085, #4714, #49673, #13250, #92282, #41134, #62501, #77159, #70545, #84712, #20343, #48257, #19860, #34081, #6133 ),
 ( #77634, #92758, #27925, #19393, #69585, #56814, #28381, #35488, #57273, #26968, #26501, #14187, #71002, #84243, #12783, #62984, #93229, #33592, #41625, #55392, #85655, #35004, #91339, #49213, #42559, #34543, #12289, #70066, #5668, #91816, #5208, #55859, #63451, #27438, #56331, #63920, #85194, #78110, #78569, #20804, #13707, #71476, #6608, #64402, #86116, #21265, #50136, #79035, #44428, #71952, #50621, #64860, #15557, #30699, #81337, #22200, #79511, #51523, #79956, #15095, #35943, #8900, #80409, #23596, #65788, #37324, #7071, #7979, #87962, #72852, #897, #37778, #58206, #73334, #8445, #36873, #57729, #51070, #66232, #93688, #23114, #1346, #29780, #14649, #28845, #43505, #43954, #87051, #87502, #21745, #58659, #7519, #30230, #59120, #52463, #66685, #22650, #1811, #72402, #51998, #36405, #80884, #88448, #65318, #43048, #16032, #44883, #29312, #86576, #73785, #59597, #425, #10299, #68550, #3688, #75644, #16949, #17889, #10767, #89357, #39625, #61466, #47203, #17432, #75185, #16484, #45340, #24513, #74722, #31176, #74241, #67623, #82281, #53395, #89838, #2750, #46282, #32573, #68080, #60991, #60061, #46742, #90296, #81802, #39168, #9843, #25448, #25000, #38246, #52923, #2292, #53871, #18348, #9362, #3205, #45815, #82737, #32089, #54325, #88899, #83201, #67160, #24048, #38715, #31630, #60521, #66077, #52303, #37169, #58955, #2124, #22491, #37617, #73629, #1189, #22042, #80255, #8740, #36236, #81180, #44728, #30070, #72692, #257, #14937, #8288, #51364, #51826, #79795, #15391, #65622, #66528, #88280, #16785, #31013, #80719, #59900, #7811, #87803, #36701, #23435, #52757, #734, #81638, #1647, #9197, #87342, #29140, #44258, #22952, #29619, #15872, #38075, #66986, #16326, #58497, #45176, #74078, #30527, #88742, #23888, #45639, #59429, #7354, #65154, #73169, #58036, #86888, #50911, #43792, #24350, #74548, #61749, #33320, #40394, #62217, #31928, #31472, #19127, #18188, #89198, #24831, #67920, #4440, #38561, #89662, #60360, #3985, #39940, #67463, #25288, #47520, #39464, #9679, #26220, #10140, #55114, #68856, #76425, #60819, #2592, #53714, #32404, #39006, #54166, #11547, #69312, #54623, #3044, #25742, #83495, #10606, #18653, #91046, #53225, #61302, #90138, #82107, #82581, #75941, #17728, #32860, #90581, #17266, #46124, #83979, #75027, #46583, #75481, #68381, #3512, #83035, #47040, #11071, #92009, #41339, #71670, #12013, #63178, #4912, #71198, #13439, #40863, #92470, #20993, #12980, #86302, #47982, #77832, #12487, #62712, #69781, #5406, #41818, #70729, #49410, #34271, #5862, #57004, #27636, #85392, #33798, #35193, #78758, #84435, #34732, #70273, #92957, #78300, #91542, #55587, #26698, #42286, #35677, #19583, #27161, #48452, #56535, #84903, #63648, #77353, #13899, #6325, #28569, #64121, #28116, #56049, #85841, #49859, #42753, #6804, #64592, #93417, #57459, #87687, #15281, #36126, #620, #22840, #50327, #1528, #58844, #44138, #86770, #14376, #29026, #22378, #36587, #65967, #146, #65501, #79688, #51707, #8625, #30891, #16211, #1078, #45062, #21931, #51251, #50803, #37502, #73043, #14830, #29958, #52185, #81066, #30414, #43684, #66411, #59305, #80141, #88153, #73962, #59784, #8173, #37057, #21454, #72580, #80595, #29505, #44612, #73516, #65043, #79234, #23312, #9076, #37956, #66863, #7702, #72134, #43236, #15752, #57913, #58387, #87230, #1998, #7250, #10021, #45519, #18070, #54046, #52637, #39346, #61636, #53592, #33205, #88625, #89543, #53105, #9550, #23772, #46005, #24706, #60703, #61181, #74910, #82465, #3869, #68265, #32275, #74421, #75825, #25626, #31353, #17612, #81983, #39815, #90019, #81517, #2476, #16664, #25172, #76305, #38437, #67800, #60241, #3387, #31810, #46463, #67346, #54508, #82916, #69199, #75366, #46923, #89079, #10480, #68738, #10949, #32748, #83380, #38891, #90469, #18528, #47394, #24228, #2925, #11431, #17139, #40282, #4328, #84785, #33673, #54984, #69662, #63059, #77235, #12862, #40745, #12365, #26578, #92357, #49290, #71557, #56894, #41701, #85733, #62582, #91888, #91424, #78185, #13788, #55467, #42640, #56412, #64000, #48334, #83860, #41213, #19935, #20879, #70150, #27518, #34620, #55930, #76768, #5286, #63530, #90930, #42164, #5745, #48805, #84316, #19013, #4794, #27042, #34156, #70618, #19467, #77712, #85272, #20421, #13323, #6692, #49751, #71080, #78648, #6212, #35081, #92838, #28001, #62097, #26095, #47865, #11896, #48317, #32731, #39329, #61619, #4310, #75806, #26077, #77218, #12346, #26561, #39798, #91406, #55450, #76287, #84301, #41195, #84767, #33188, #62078, #46446, #10930, #47848, #54491, #69646, #4774, #90001, #75348, #33656, #5269, #70133, #34138, #3850, #3371, #10463, #83842, #61164, #90451, #68720, #63041, #68247, #25608, #32259, #62565, #11878, #25156, #90911, #19451, #11413, #54030, #82897, #47373, #83359, #18053, #46905, #18509, #40264, #69181, #18995, #54966, #76750, #91872, #40729, #27026, #55915, #7132, #50682, #56394, #78630, #78169, #64921, #21327, #48788, #27496, #41683, #86176, #7579, #58269, #92822, #85256, #28441, #56876, #85717, #12845, #79568, #57334, #491, #42621, #14250, #77696, #13772, #24, #49733, #13307, #50197, #27985, #43108, #72015, #63513, #70601, #36003, #72460, #14711, #36464, #71063, #5728, #34603, #79101, #92341, #63982, #42145, #43564, #20404, #35062, #49274, #28903, #57791, #6195, #64463, #86641, #71540, #20862, #6673, #35550, #93290, #65379, #29375, #44489, #23180, #59179, #59663, #73393, #52063, #2355, #37837, #30761, #44017, #74298, #24105, #29836, #80945, #51582, #38309, #88506, #22261, #957, #15158, #23653, #74784, #31687, #66292, #58719, #1869, #30291, #88023, #80018, #52986, #52519, #67679, #16090, #81395, #51135, #44942, #67224, #73842, #8958, #81860, #8503, #16543, #45399, #66743, #8041, #1404, #9422, #72914, #31233, #60119, #88958, #87563, #36935, #22708, #17009, #37382, #45878, #65849, #9901, #80468, #38775, #2805, #87111, #15617, #40159, #55342, #32151, #61517, #61052, #76640, #12236, #89895, #41083, #54845, #62444, #46797, #53459, #75699, #18402, #25053, #69076, #91287, #26453, #40617, #53926, #11765, #69533, #90348, #4666, #84193, #5150, #47261, #76175, #60582, #82794, #82340, #68140, #25504, #10824, #11307, #39222, #39684, #17946, #90805, #47742, #70007, #19341, #4204, #48203, #68608, #54382, #3745, #33539, #89417, #32627, #24571, #83727, #77105, #83258, #17488, #33079, #61968, #25964, #18887, #46340, #75242, #10357, #3261, #78977, #42994, #63868, #14129, #28790, #72347, #85606, #49624, #34027, #92231, #35432, #42036, #57222, #86062, #77577, #62931, #21212, #86520, #93633, #21685, #85136, #84656, #91765, #71421, #48676, #78058, #27387, #57677, #26917, #49165, #19808, #50082, #93180, #55804, #78520, #7020, #92702, #12728, #41571, #34956, #56277, #70493, #5621, #20291, #27872, #6082, #6553, #13200, #56765, #71900, #13657, #64354, #34496, #35891, #64809, #63402, #20753, #70950, #50562, #28332, #42509, #79459, #14593, #43450, #88847, #45756, #80358, #15041, #15979, #44370, #73281, #368, #67103, #44831, #81748, #30177, #1755, #36348, #66178, #52412, #37272, #59061, #2237, #22594, #37724, #73734, #1295, #22148, #15499, #8846, #65262, #81287, #66630, #87909, #23060, #51938, #7465, #65734, #30642, #8394, #59541, #88391, #51016, #29254, #23542, #60007, #31121, #23996, #58607, #58150 ),
 ( #16433, #845, #9307, #36813, #80828, #86996, #72798, #51469, #45285, #79903, #7922, #52869, #74188, #16898, #29726, #87448, #38189, #43901, #32515, #46230, #4553, #33427, #19235, #53339, #24941, #55230, #40503, #2698, #68026, #75590, #67569, #74666, #61860, #90243, #10713, #90691, #83611, #31580, #17378, #61411, #53818, #24460, #26337, #3153, #89304, #76060, #60469, #10244, #32036, #11189, #39570, #39113, #69422, #62331, #40049, #68492, #91171, #75134, #60931, #83142, #82224, #3627, #89778, #68966, #18293, #82686, #46688, #54733, #47151, #17836, #4096, #25392, #84085, #54272, #32967, #25851, #47630, #18772, #76534, #9790, #11656, #38665, #57566, #92585, #55694, #49516, #12125, #40971, #84545, #49050, #63287, #27754, #26808, #92120, #12607, #78408, #35312, #86409, #42872, #56650, #71785, #19692, #77945, #48561, #64237, #93521, #77464, #28680, #42396, #49970, #34382, #69893, #27274, #5971, #41452, #85499, #78862, #14012, #28222, #70384, #93068, #57110, #13089, #85950, #6907, #48092, #34844, #63755, #76996, #5512, #13547, #56161, #71307, #6437, #91655, #5032, #21102, #35782, #64695, #33912, #85018, #62821, #20170, #20646, #41927, #70838, #14938, #45177, #79350, #36702, #72240, #44729, #80720, #14485, #66078, #88281, #80256, #59901, #21565, #22492, #79796, #36237, #50448, #72693, #51365, #87343, #87804, #7812, #15392, #30528, #1190, #58956, #7355, #8741, #52304, #58037, #44259, #43793, #66529, #22953, #43343, #29141, #65155, #51827, #9198, #258, #735, #86889, #30071, #58498, #73170, #22043, #81181, #15873, #2125, #8289, #73630, #50912, #37170, #1648, #37618, #59430, #16327, #65623, #23436, #74079, #38076, #29620, #66987, #31014, #23889, #68857, #32405, #17729, #60361, #75942, #18189, #82108, #90582, #24351, #89663, #16786, #89199, #39007, #54167, #52758, #53226, #54624, #11072, #76426, #17267, #46125, #67921, #11548, #46584, #75028, #18654, #47521, #33321, #67464, #3045, #69313, #83496, #45640, #10141, #24832, #81639, #88743, #39941, #10607, #53715, #3986, #32861, #74549, #31473, #75482, #31929, #38562, #40395, #60820, #9680, #90139, #2593, #82582, #39465, #25289, #68382, #3513, #4441, #61303, #83036, #47041, #61750, #25743, #91543, #70730, #47983, #63179, #26699, #27637, #5863, #83980, #34272, #42287, #34733, #62713, #63649, #4913, #78759, #70274, #85393, #48933, #35194, #48453, #12014, #20994, #92471, #91047, #71671, #12981, #69782, #56536, #26221, #55588, #92010, #71199, #6805, #27162, #20541, #77833, #49411, #42754, #28117, #56050, #13900, #13440, #84436, #62218, #57005, #78301, #76886, #55115, #41340, #92958, #41819, #19128, #40864, #6326, #84904, #85842, #64122, #49860, #33799, #19584, #77354, #12488, #5407, #20052, #82355, #30779, #23669, #93418, #2370, #7251, #79689, #31248, #28570, #36127, #2822, #24122, #24589, #147, #65044, #14831, #53478, #88521, #29027, #60597, #89432, #75257, #14377, #43685, #17503, #31704, #57460, #57914, #37854, #86303, #35678, #53001, #52535, #66758, #81875, #45895, #21455, #72135, #81410, #72581, #79235, #46356, #86771, #50328, #38326, #43237, #21932, #50804, #67240, #1887, #7703, #64593, #59678, #60135, #16560, #45414, #74315, #9439, #88974, #17029, #74800, #9917, #38790, #67694, #32167, #76191, #84207, #18900, #10837, #76653, #46812, #26929, #18415, #33552, #90818, #77120, #90362, #53939, #62944, #11780, #39239, #19822, #54862, #17959, #40630, #68155, #39700, #11321, #19354, #48688, #40172, #47755, #25977, #4678, #84673, #70023, #69091, #55817, #55355, #68624, #10372, #5166, #62461, #89911, #3275, #83271, #41095, #83743, #61068, #25067, #69548, #4217, #34041, #91303, #26466, #82808, #48218, #91778, #75714, #47275, #3758, #32643, #33092, #12249, #61531, #25519, #54398, #61983, #70964, #79474, #13214, #78533, #5634, #43466, #35905, #63416, #70507, #56778, #14608, #28345, #34509, #41585, #57235, #71434, #72363, #93193, #64823, #92245, #86077, #7480, #27402, #85620, #36365, #29271, #6570, #64367, #56290, #43010, #93647, #7035, #6096, #65278, #42050, #13672, #85153, #49177, #27888, #71914, #20306, #78071, #383, #28807, #58167, #34968, #63882, #20766, #87011, #35448, #92718, #22163, #77593, #12743, #49638, #42522, #21228, #50097, #78991, #14146, #57691, #86534, #21702, #50579, #66647, #80846, #38205, #60024, #43918, #87463, #37739, #30192, #860, #2713, #73297, #65751, #52427, #36832, #80373, #8409, #81302, #15994, #15514, #16913, #45771, #16448, #44846, #67584, #51485, #44388, #59558, #29741, #51954, #37287, #45300, #88408, #72813, #23075, #31137, #23559, #66194, #74205, #22610, #31594, #59081, #9322, #1773, #24010, #1310, #58622, #9805, #67119, #79919, #60483, #30657, #87924, #2254, #15056, #73749, #8861, #88861, #89320, #52883, #81763, #74681, #38679, #51031, #7939, #54287, #69908, #69439, #53835, #40987, #68982, #18310, #55245, #40064, #76549, #46244, #4112, #84102, #82239, #32534, #19251, #5047, #47166, #11206, #17395, #83626, #11672, #47647, #17852, #26354, #82701, #25408, #75148, #89795, #68508, #18788, #10260, #24959, #48109, #40521, #12141, #46703, #75606, #3643, #33929, #76075, #10729, #77013, #62837, #24475, #3167, #61427, #53354, #39130, #68041, #39585, #83157, #32052, #60946, #4569, #32984, #61875, #33443, #62346, #90259, #90706, #25867, #54749, #91187, #43358, #20185, #12622, #93082, #77479, #27290, #49065, #28237, #27770, #56177, #57580, #86425, #57124, #85513, #14501, #92135, #85035, #6452, #41468, #92600, #77962, #85966, #35327, #19708, #63771, #71800, #64253, #13105, #21116, #34397, #72254, #5986, #49984, #78423, #64709, #41942, #70400, #50462, #78878, #26823, #7371, #42411, #5527, #14026, #55710, #70854, #56664, #6922, #36252, #20659, #42887, #13561, #35796, #91670, #21580, #49530, #84561, #93536, #34858, #48579, #79365, #28695, #63304, #71322, #44276, #2141, #15888, #22059, #29156, #23905, #31030, #52776, #22509, #50928, #9696, #8756, #79812, #15409, #58514, #88759, #58053, #80271, #14953, #88296, #30546, #86904, #44744, #38095, #30088, #65171, #276, #66094, #29635, #43808, #72708, #51380, #1206, #37186, #37635, #73185, #58972, #74096, #73646, #66543, #7829, #52319, #59918, #36718, #87820, #87359, #16343, #1664, #65638, #751, #8304, #59445, #81655, #22970, #51842, #80736, #23452, #81197, #45193, #9215, #16803, #67005, #45659, #74567, #32877, #67480, #3529, #83514, #68400, #90156, #33335, #53731, #68872, #11090, #32419, #53245, #17744, #39956, #2610, #18671, #75960, #61318, #10156, #31489, #46141, #39479, #82597, #83052, #17284, #46598, #3061, #4002, #25758, #47997, #62232, #18205, #91065, #39024, #25304, #67938, #54640, #83995, #31946, #19142, #61765, #40410, #24848, #60377, #75498, #54182, #60838, #47056, #69328, #4458, #47537, #89681, #76441, #11562, #90598, #26237, #55130, #76901, #38577, #89216, #24367, #10621, #82127, #75044, #35214, #64141, #55602, #12031, #92974, #63664, #27655, #40878, #70289, #13455, #20070, #28132, #57021, #84450, #69796, #85858, #64608, #71690, #93434, #63194, #62727, #50348, #49427, #26714, #56066, #5421, #35694, #4930, #27179, #91557, #21010, #71215, #33816, #56554, #78775, #70745, #19600, #48468, #12997, #34286, #77368, #12505, #92024, #41834, #77848, #78316, #84919, #5879, #49877, #85408, #42306, #41356, #13916, #42772, #48950, #34749, #92487, #6820, #6342, #20556 ),
 ( #28587, #57478, #86319, #21471, #14394, #59320, #22856, #8193, #50822, #72151, #86790, #80161, #640, #29975, #57935, #29524, #43701, #15770, #66427, #88640, #73977, #58859, #9094, #79706, #15299, #14848, #1546, #30909, #72600, #59799, #73531, #81082, #65522, #7267, #58404, #37074, #7721, #87705, #16226, #45077, #88171, #36604, #30429, #23331, #44157, #52200, #37971, #23788, #51722, #66879, #43253, #87250, #2016, #79253, #73063, #65983, #36144, #44629, #65064, #8640, #22396, #164, #51268, #1094, #29043, #80613, #37517, #21949, #16680, #53120, #18541, #39828, #40295, #17156, #82000, #2940, #69211, #10494, #24246, #76318, #11444, #90944, #31368, #31826, #33217, #47408, #74436, #46022, #53608, #45535, #52652, #68752, #68279, #82479, #3882, #61648, #9567, #89094, #39363, #60717, #2491, #4340, #74925, #67361, #54059, #38455, #10036, #38906, #82930, #17626, #67815, #62113, #81532, #18082, #46477, #60257, #89556, #24724, #61197, #75381, #3401, #32292, #46936, #90034, #25186, #75838, #32760, #10961, #90481, #25639, #54522, #83391, #34170, #49302, #12876, #92850, #12379, #69676, #78659, #92369, #55001, #35578, #70630, #33687, #27530, #83874, #26591, #27056, #35092, #64493, #91902, #63542, #41714, #20434, #6704, #85745, #55942, #71568, #71090, #55481, #42651, #20892, #78197, #11909, #19025, #5300, #56905, #5757, #76782, #47879, #34631, #19948, #49764, #56423, #13336, #40758, #42177, #26108, #13800, #84798, #4807, #6223, #84330, #62596, #91440, #64011, #19480, #48347, #63072, #77250, #85284, #41226, #70165, #28014, #48819, #77725, #58296, #36964, #21357, #87139, #51614, #28471, #79598, #80502, #66322, #36494, #29405, #57364, #44048, #65877, #8076, #28934, #15650, #64952, #43594, #86206, #7160, #50711, #72949, #50227, #36035, #44520, #986, #73424, #53, #57820, #21836, #37413, #521, #86671, #8534, #1437, #30322, #43140, #14739, #93319, #79131, #72490, #7606, #22290, #72044, #14278, #65411, #51161, #80048, #15188, #29867, #22740, #58752, #87594, #63389, #34015, #35877, #12715, #5136, #85592, #69996, #19796, #41557, #20739, #20275, #48665, #50067, #78963, #49610, #78046, #7005, #84645, #77566, #92688, #62918, #85124, #70480, #78505, #27858, #12224, #56264, #64338, #56749, #5608, #13643, #26905, #64794, #92219, #42494, #70937, #57206, #34483, #91753, #42977, #71408, #19330, #93618, #34941, #55793, #6540, #48192, #27374, #49150, #93165, #28776, #13187, #35417, #6068, #42022, #28317, #84182, #63855, #77094, #86047, #21196, #14114, #41071, #71883, #15487, #86982, #37260, #88377, #23527, #37711, #51003, #8833, #66617, #87436, #1740, #52396, #2222, #44358, #73268, #57660, #22135, #59047, #65719, #80815, #15964, #7452, #86507, #44818, #16419, #81273, #45271, #15029, #14580, #21670, #1282, #72333, #7909, #79890, #74174, #50547, #72784, #43437, #73721, #23047, #79444, #8380, #30627, #22582, #36334, #65248, #58595, #43888, #354, #29241, #36799, #51456, #29713, #30164, #831, #80345, #59528, #66166, #87894, #58136, #9291, #38174, #51925, #67089, #89290, #77335, #33777, #59993, #38651, #52855, #4893, #20034, #70712, #10229, #67555, #40843, #68009, #3138, #23982, #91990, #69762, #12962, #53802, #26679, #88832, #89763, #12469, #60917, #82670, #27143, #46215, #62690, #91523, #24925, #45740, #39097, #55569, #81733, #41316, #84417, #17818, #2684, #16881, #31564, #32018, #75119, #75575, #9776, #46672, #24443, #19565, #48431, #41801, #56028, #11994, #84883, #60455, #70253, #63159, #5388, #34253, #74651, #48911, #77813, #53324, #31106, #82209, #17364, #93400, #86284, #63629, #65029, #86753, #29012, #92938, #7687, #35176, #6783, #27617, #71179, #49842, #129, #92454, #6308, #65487, #21915, #87214, #64098, #28099, #78739, #22362, #57443, #56986, #29487, #58372, #44122, #78283, #13882, #80124, #604, #56514, #85824, #35660, #85373, #5843, #50789, #21437, #64575, #79674, #14815, #20523, #42266, #50311, #42735, #49391, #51236, #20975, #13421, #7236, #71650, #28552, #79216, #36111, #14359, #43219, #15263, #34715, #57897, #72120, #43670, #72565, #36572, #81501, #58826, #73945, #8609, #38419, #16648, #1062, #45044, #53087, #45502, #73497, #74404, #15732, #89526, #81049, #2460, #59767, #45988, #59289, #22821, #31792, #9534, #8154, #82448, #23756, #80579, #67328, #37037, #37485, #9060, #81966, #17596, #37938, #31336, #88608, #60223, #53573, #38875, #66847, #24689, #24212, #66395, #73026, #67782, #89062, #87671, #65951, #52166, #10004, #52619, #29941, #51690, #17122, #1982, #1511, #74893, #44593, #30397, #88135, #2908, #60686, #23293, #16192, #30873, #87356, #65167, #15406, #1661, #30542, #15885, #29153, #80732, #44741, #65634, #73643, #59442, #74092, #22506, #51377, #35793, #273, #37183, #43805, #58969, #87816, #79362, #64706, #22967, #88293, #23448, #52316, #86901, #86422, #93533, #73182, #50459, #79809, #58050, #81193, #28691, #50925, #21577, #51839, #1203, #57577, #80268, #8753, #748, #14497, #43355, #36714, #22056, #72251, #7368, #14950, #29632, #7825, #8301, #72705, #58511, #37632, #44272, #66090, #36249, #16339, #45189, #30085, #67934, #67476, #54178, #10617, #38091, #16799, #31026, #75493, #90594, #47533, #82123, #45655, #17740, #46137, #75040, #2137, #68868, #46594, #83509, #31942, #3525, #67001, #3057, #83048, #39019, #60833, #3998, #24363, #39475, #68395, #89677, #23901, #17280, #32415, #59913, #18200, #61314, #24844, #74563, #88755, #9692, #10152, #53241, #53727, #81651, #82593, #2605, #90152, #25300, #18667, #32873, #47052, #61761, #38573, #75955, #11086, #25754, #31485, #60373, #39952, #54635, #9211, #89212, #52772, #6337, #21005, #55126, #26710, #57016, #42300, #4452, #69792, #77364, #69324, #76437, #63659, #92020, #12500, #92482, #85403, #33331, #19138, #63190, #55598, #26233, #28127, #4925, #91059, #77843, #62228, #12026, #33811, #12991, #41352, #40874, #71210, #35208, #41829, #70284, #92969, #76897, #62723, #84914, #83991, #5417, #91553, #70740, #20064, #47993, #48464, #56548, #48945, #84446, #5874, #19595, #85852, #34282, #34743, #27173, #49421, #56061, #27649, #64136, #20551, #11558, #40406, #78311, #13450, #51263, #13911, #50342, #50817, #58855, #59316, #21944, #87245, #65516, #44151, #30425, #15766, #79701, #1541, #1089, #79248, #66423, #44625, #8188, #35689, #42766, #29038, #80608, #635, #6815, #71685, #29519, #43696, #73527, #58399, #37069, #64603, #22391, #8636, #93429, #57929, #37513, #88167, #72594, #36599, #28581, #15294, #65978, #73058, #43248, #51718, #14389, #14843, #57472, #21466, #159, #29970, #86314, #72146, #49871, #7262, #86785, #78770, #80155, #36139, #65057, #87700, #7715, #22852, #38902, #75377, #45073, #2936, #54056, #81078, #31364, #82926, #68749, #17152, #10032, #16222, #82475, #10490, #46473, #16675, #25182, #52648, #24241, #73973, #88636, #67357, #17622, #9089, #23784, #18079, #39358, #10958, #81528, #45531, #2487, #39825, #74921, #74432, #46932, #75835, #61645, #2012, #60253, #3879, #32757, #37967, #9563, #53116, #66875, #23326, #68275, #67811, #81996, #3397, #32288, #30905, #59795, #31821, #89090, #38451, #52196, #46018, #60713, #24720, #89552, #53604, #61193, #90030, #26588, #54998, #57702, #86545, #57246, #84327, #14620, #90941, #26105, #5297, #76315, #91436, #83870, #86088, #34167, #18538, #62593, #71925, #63069, #19022, #91899 ),
 ( #79003, #50591, #21716, #79485, #47876, #47405, #36376, #27053, #55478, #19477, #21239, #76779, #48344, #7046, #41223, #50108, #11441, #14158, #28818, #33214, #77246, #11906, #43022, #35916, #25635, #4337, #40292, #64834, #43477, #90478, #69672, #62109, #93658, #33684, #12376, #83388, #72374, #7491, #54518, #70162, #69208, #40755, #4804, #16456, #1319, #23084, #60033, #80382, #1782, #37748, #59091, #79928, #44398, #66656, #394, #45308, #8870, #87933, #36844, #58180, #72823, #66203, #15523, #16003, #43927, #73307, #29750, #30666, #52435, #74692, #88870, #44855, #24019, #65761, #30201, #871, #81310, #16922, #58631, #45781, #59569, #67129, #51494, #87022, #8418, #51964, #87472, #73758, #2264, #31146, #74213, #22619, #9332, #38215, #80856, #52893, #81772, #9815, #88418, #23568, #65289, #37297, #29284, #22173, #51041, #15065, #7948, #38688, #25877, #91197, #4578, #26365, #89807, #89329, #77021, #76086, #53364, #82710, #32061, #62355, #2723, #53844, #24484, #61885, #4122, #31603, #83169, #11682, #3655, #67594, #60492, #39596, #3177, #82250, #17405, #24969, #46253, #68519, #60956, #75157, #10269, #17861, #32545, #10739, #11219, #46712, #61437, #47658, #18320, #40075, #39139, #54759, #69448, #68050, #90268, #75615, #83636, #68992, #25419, #54297, #47176, #32994, #55255, #90717, #18799, #76559, #40532, #33453, #84110, #19260, #48118, #49540, #86433, #34868, #6463, #40995, #70864, #57134, #41951, #63781, #6932, #27300, #42421, #78435, #5995, #26831, #85047, #13571, #69918, #85976, #71333, #92610, #77489, #5057, #19718, #13115, #56187, #56674, #84571, #20196, #70411, #35338, #93093, #21592, #35805, #85523, #64719, #12634, #27781, #41479, #28247, #57589, #5536, #50471, #64263, #14036, #92145, #33940, #49074, #20668, #34407, #21126, #42898, #71810, #49994, #63314, #78889, #93545, #28704, #12150, #62846, #91680, #55719, #48589, #77973, #43817, #80745, #87367, #8764, #37643, #29165, #79374, #66551, #38104, #45201, #67014, #36726, #36261, #23914, #22979, #285, #29644, #72716, #9223, #43367, #759, #65182, #1673, #44753, #72263, #30096, #52328, #44286, #14511, #22068, #66102, #58524, #58061, #31039, #7839, #86913, #15896, #50936, #14961, #65645, #73654, #15418, #22517, #74104, #2149, #30555, #73193, #59929, #79820, #51388, #87828, #80279, #8312, #37195, #59453, #51853, #7381, #1214, #88304, #23461, #58980, #81205, #16351, #88768, #60848, #75973, #39489, #25770, #39034, #2620, #11573, #25315, #81664, #62244, #3541, #60386, #54194, #16812, #53255, #53741, #61776, #91079, #24857, #90167, #68412, #47067, #33347, #18684, #82607, #4470, #4013, #82137, #69339, #47548, #11102, #38586, #45669, #31955, #83526, #32430, #9705, #74577, #61329, #46607, #76452, #83063, #39967, #67489, #18217, #40421, #31498, #89691, #52786, #89225, #75509, #68883, #24376, #32889, #90609, #54652, #46150, #17294, #75054, #17754, #10165, #67947, #3070, #10631, #84006, #26728, #85871, #13468, #13928, #84463, #55614, #70303, #42786, #77861, #91571, #49890, #78787, #64619, #4945, #5434, #6831, #21022, #48010, #19613, #27192, #19154, #26250, #42318, #41847, #56079, #71227, #35227, #76914, #5892, #71703, #48482, #84932, #77381, #6354, #35705, #12519, #55143, #20568, #28144, #41369, #12044, #34300, #13011, #63207, #34762, #57033, #40891, #64153, #92037, #92986, #69809, #20084, #33831, #62740, #48965, #70759, #63677, #92500, #27669, #56567, #85420, #49440, #78328, #43264, #93445, #80626, #52212, #59333, #81094, #50834, #50360, #37983, #37085, #14405, #43713, #86803, #23344, #57489, #14860, #79265, #22868, #58870, #86331, #44169, #66438, #58415, #28599, #21482, #652, #57948, #72162, #7278, #79718, #29535, #65535, #65994, #72612, #87261, #8651, #73075, #1105, #36155, #15782, #30441, #65077, #22407, #21961, #44640, #29986, #176, #29056, #7734, #87717, #16238, #36615, #51279, #80172, #8206, #15310, #51733, #73542, #88184, #37528, #73989, #1558, #45088, #9106, #31839, #18093, #2953, #24738, #61659, #82012, #3412, #39375, #60729, #81544, #46034, #68291, #2030, #46947, #10506, #89568, #38469, #59811, #74448, #67828, #17169, #17639, #45547, #74939, #31380, #32305, #54071, #76330, #90491, #23800, #82941, #3894, #9580, #53621, #60269, #75849, #61210, #30921, #67373, #88652, #90045, #54533, #11455, #10049, #2502, #75393, #38919, #82491, #52664, #32771, #25197, #47420, #46490, #10972, #16692, #39840, #68764, #25650, #83402, #18552, #66891, #89106, #24258, #53132, #55013, #19492, #12888, #69222, #20446, #77737, #63084, #11920, #33228, #47891, #41237, #55493, #84809, #19036, #84341, #4817, #70641, #27541, #49774, #35104, #19959, #64022, #40769, #70177, #69687, #56433, #85755, #33698, #20902, #34643, #42188, #26602, #62124, #48358, #91913, #62609, #48830, #71101, #6234, #49314, #91452, #85296, #78208, #5312, #13347, #92862, #78669, #27067, #55954, #40307, #77261, #41725, #12391, #63553, #92382, #83886, #4351, #28026, #56915, #90955, #26119, #34181, #76794, #5769, #51169, #28480, #57829, #7169, #37421, #71579, #28943, #64503, #36972, #72956, #6715, #58305, #80510, #72498, #52102, #13810, #14747, #72053, #57373, #42662, #64961, #43602, #79606, #80056, #62, #7615, #22748, #87148, #15196, #36044, #43150, #86679, #30330, #65418, #79140, #66332, #1445, #35589, #86215, #21844, #88065, #73432, #93329, #50721, #36502, #21367, #50237, #995, #29414, #529, #29876, #51623, #14289, #22298, #44056, #8084, #65886, #59220, #58760, #87602, #15658, #44528, #8542, #23222, #82381, #17054, #45439, #46839, #75742, #46381, #74827, #3786, #81435, #16583, #89459, #66783, #81901, #74340, #75281, #24620, #8999, #53023, #61098, #53505, #9464, #17531, #23694, #32670, #88998, #10400, #67718, #53967, #67262, #30803, #39728, #39265, #16129, #90389, #31730, #88546, #68181, #44980, #38349, #45919, #89937, #25545, #9941, #3302, #2849, #32193, #61556, #10865, #38814, #80987, #25093, #2395, #73881, #68651, #82834, #1913, #37877, #60159, #17987, #60621, #59702, #52558, #31272, #24145, #85190, #70062, #12778, #76218, #34077, #20338, #18445, #62496, #49208, #6129, #48252, #41129, #47303, #19855, #41620, #77628, #47784, #56326, #83773, #55388, #11348, #26010, #4709, #48726, #40202, #54896, #78104, #70541, #42081, #33124, #69581, #18929, #84708, #5663, #63916, #13245, #62979, #70997, #76685, #84239, #11810, #34539, #35000, #40661, #92753, #63447, #54426, #33587, #69118, #91335, #12285, #26497, #91812, #83297, #4244, #92278, #19389, #27434, #62013, #77154, #90848, #5203, #26964, #55855, #43502, #27921, #86112, #29309, #35939, #51065, #79952, #71472, #56809, #15090, #80405, #87497, #15552, #79030, #78565, #66228, #65315, #42555, #71948, #21261, #51518, #85651, #43045, #13703, #43950, #87047, #20799, #72398, #893, #86573, #49669, #6604, #28842, #50131, #35482, #64398, #14184, #57726, #93684, #422, #7068, #21742, #36869, #7516, #58203, #93224, #72847, #58655, #28377, #50618, #64857, #7975, #22196, #57268, #79508, #14645, #65784, #44424, #36401, #29776, #22646, #73330, #8441, #37320, #87957, #62262, #39984, #76932, #24044, #90625, #30225, #60057, #47564, #31171, #52919, #91095, #16480, #32905, #68900, #88895, #16028, #74237, #4032, #59116, #76469, #61793, #81798, #66680, #23110, #8896, #2288, #45336, #47084, #23592, #44879, #25787, #80881, #30693, #52459 ),
 ( #54668, #18233, #69355, #81333, #73781, #55160, #83542, #51993, #12060, #75989, #37774, #18700, #1807, #59593, #11118, #11590, #40907, #67155, #40438, #4485, #33362, #1342, #26266, #84022, #48027, #19169, #88443, #9357, #38241, #28162, #55631, #62756, #48983, #6849, #20587, #26745, #33847, #49457, #63695, #35723, #85437, #57053, #91588, #78345, #64637, #84480, #77881, #93465, #21501, #92520, #56584, #19630, #35246, #85889, #93004, #63224, #71722, #5449, #70777, #48499, #41386, #20101, #64172, #77398, #70319, #28618, #21041, #57507, #34318, #92056, #13028, #86351, #27686, #27210, #50379, #79283, #14424, #12535, #41864, #69827, #4962, #56097, #84951, #5910, #34780, #13487, #49909, #42334, #71245, #78804, #13949, #6374, #42806, #30006, #22427, #86821, #88672, #23821, #9127, #65094, #36635, #44191, #36175, #81565, #30461, #58891, #73096, #59356, #52232, #194, #79735, #87737, #51299, #21979, #52684, #65556, #57967, #44662, #29075, #72631, #670, #73563, #8226, #7751, #38004, #66914, #8672, #37104, #59831, #43731, #29554, #51759, #50852, #66013, #58434, #37550, #80648, #14877, #15331, #23365, #15803, #87280, #66461, #80192, #43281, #1125, #1579, #22889, #16258, #88208, #81115, #2052, #45108, #72179, #7295, #74010, #30943, #18118, #74472, #17193, #17661, #25676, #26143, #82512, #54093, #32331, #10996, #90977, #76353, #46514, #62148, #61681, #46054, #33251, #11479, #68786, #2524, #9603, #89589, #47444, #61233, #67396, #38491, #90068, #10531, #40329, #25220, #3916, #31401, #82965, #69245, #60291, #24760, #4373, #55038, #39398, #3436, #89128, #75872, #32792, #39865, #10072, #18578, #74960, #75415, #24279, #82035, #60749, #90512, #53154, #38940, #16713, #54555, #45568, #67849, #2975, #53643, #31860, #68313, #46970, #83423, #13830, #28499, #62634, #34202, #34663, #27562, #40792, #71124, #20923, #26624, #48855, #48380, #35122, #85319, #19059, #91474, #11943, #56457, #71599, #83907, #63107, #55515, #92402, #27089, #55976, #76817, #49792, #20469, #64523, #12909, #78230, #47914, #77760, #64043, #19979, #41747, #78689, #5334, #49336, #13369, #70660, #4840, #91935, #42210, #69709, #92885, #6254, #5789, #84364, #33723, #19513, #84830, #63577, #28046, #77283, #56936, #12413, #85773, #42681, #93348, #6734, #35607, #41263, #70201, #58324, #57847, #73450, #9016, #86701, #37895, #51642, #59239, #43619, #50254, #72516, #15217, #21865, #36991, #88085, #23242, #37440, #50741, #8561, #66349, #87167, #1464, #52121, #1930, #44073, #72975, #57391, #79625, #58779, #65436, #80528, #15681, #7187, #86233, #44547, #16146, #81003, #44998, #14766, #14308, #21385, #1016, #72070, #7636, #36520, #73900, #79161, #550, #43169, #30350, #22773, #36062, #8104, #66800, #22316, #64979, #82, #51187, #29433, #28961, #80074, #65903, #29895, #87622, #17549, #89016, #9959, #89957, #24163, #52575, #61574, #82401, #16604, #53044, #31292, #75764, #59721, #81919, #81455, #39284, #10420, #88564, #89478, #53986, #67738, #30824, #23712, #24638, #45938, #2412, #45459, #38831, #53525, #46401, #61118, #2864, #75301, #39747, #68202, #32212, #60178, #18007, #32688, #17071, #3322, #74846, #10884, #25112, #9482, #31748, #67282, #82855, #74359, #38368, #46860, #68672, #60640, #3807, #87460, #14605, #81299, #59078, #2250, #44384, #15991, #50576, #80370, #66644, #51482, #73294, #16445, #36829, #51951, #87921, #15511, #36362, #857, #23072, #79471, #1770, #80842, #8406, #87008, #43463, #29268, #22607, #65748, #66190, #380, #29738, #79916, #44843, #8858, #31134, #45297, #1307, #74202, #22160, #37284, #51028, #37736, #67116, #15053, #60020, #73746, #23555, #7935, #72360, #58619, #30189, #43915, #30654, #52424, #9319, #59555, #72810, #88405, #38202, #21699, #7477, #65275, #58164, #46700, #10726, #88859, #53352, #90256, #3164, #18306, #47163, #38677, #24008, #76072, #47643, #54745, #76546, #81761, #33440, #11203, #39582, #24955, #40061, #4109, #16911, #31592, #75602, #68038, #67582, #40518, #17393, #9803, #25405, #74679, #24472, #46242, #54284, #53832, #82237, #83623, #18785, #83154, #82698, #11669, #89318, #75146, #3640, #2710, #89792, #10258, #68979, #32530, #45769, #60943, #32981, #61424, #39126, #61872, #60481, #69436, #32049, #90703, #68505, #25864, #17849, #4566, #52881, #34855, #91183, #71797, #13101, #69905, #63768, #26351, #62833, #63301, #71319, #6919, #34394, #5983, #77958, #56661, #42884, #28233, #92132, #14023, #13558, #91667, #78875, #57121, #78420, #48106, #55242, #41465, #93079, #41939, #19248, #84099, #70851, #56174, #85962, #92597, #42408, #77010, #27766, #21113, #12138, #70396, #49981, #62343, #85031, #49062, #40984, #85510, #6449, #35324, #55707, #64249, #84558, #27287, #5044, #33925, #12619, #19705, #48575, #77476, #5524, #20182, #12394, #82945, #54075, #68767, #41240, #76333, #90049, #48361, #77264, #63087, #3416, #3897, #5315, #84344, #46494, #18097, #25653, #76797, #68295, #24743, #11923, #70182, #19495, #34184, #75853, #75397, #53625, #62127, #39380, #32774, #46951, #82495, #17643, #39845, #10510, #47894, #83889, #61214, #69225, #91455, #83405, #25201, #10975, #54536, #61662, #90494, #18556, #47423, #11458, #40310, #90958, #4354, #33231, #33702, #26123, #55018, #19039, #40772, #55496, #69690, #4820, #62614, #26605, #93331, #27070, #5771, #19961, #64505, #79608, #36504, #71103, #34645, #6718, #35106, #64025, #84811, #57831, #35591, #72500, #20905, #86217, #55957, #56917, #43152, #28028, #49776, #86682, #13349, #28482, #57375, #85757, #12890, #6236, #21369, #48833, #72055, #50239, #78671, #63555, #77740, #92384, #92866, #42190, #42664, #70643, #13812, #56436, #79143, #14293, #7618, #21847, #71581, #50723, #27544, #7171, #85300, #36046, #43604, #20448, #91916, #64963, #64, #78210, #41727, #28945, #14749, #49316, #44983, #2397, #31274, #45441, #58762, #16585, #74342, #1447, #9466, #60161, #9943, #23225, #80989, #65420, #29878, #66785, #73434, #88548, #23696, #52104, #38351, #51625, #15198, #24147, #37879, #532, #74831, #16131, #72958, #1915, #29417, #65888, #66334, #67265, #58307, #37423, #9001, #73883, #59705, #45921, #89000, #30332, #17056, #53025, #998, #81903, #87150, #52560, #51171, #22300, #44531, #80058, #30806, #44058, #8087, #81438, #59222, #36975, #87604, #22750, #80512, #15661, #8544, #88068, #46842, #69584, #84242, #32673, #25548, #2852, #4247, #26013, #62016, #32196, #40664, #68185, #39731, #60624, #10403, #82837, #33127, #31733, #39268, #4712, #54899, #26500, #3306, #61101, #17990, #55391, #90392, #89941, #62499, #91338, #77157, #17534, #75745, #19392, #33590, #89462, #25096, #68654, #24623, #38816, #83776, #54429, #3790, #18932, #47787, #53508, #75284, #83300, #10868, #82385, #48255, #53970, #46384, #40205, #61559, #18448, #47306, #69121, #76221, #11352, #67720, #90851, #76688, #11813, #30115, #12781, #41623, #20802, #91815, #13248, #70544, #71475, #49672, #34080, #78107, #86115, #78568, #5666, #13706, #48729, #58998, #20341, #92281, #63919, #34542, #85654, #44304, #73215, #21264, #63450, #57271, #50134, #42084, #79033, #8331, #51871, #92756, #27924, #12288, #27437, #42558, #49211, #35485, #64401, #55858, #41132, #93227, #66119, #37212, #1233, #56329, #62982, #70065, #6607, #26967, #85193, #71000, #87847, #5206, #6132, #84711, #28380, #15438, #19858, #56812, #22996, #35003 ),
 ( #77631, #53271, #68428, #25332, #59943, #88324, #89241, #23931, #52802, #73671, #46626, #24394, #61350, #9723, #75069, #15916, #45686, #31972, #16829, #38602, #75526, #2167, #17311, #82155, #74594, #1690, #88783, #46166, #44771, #60865, #10181, #67506, #52345, #8782, #23479, #81680, #31056, #31515, #59469, #2636, #45219, #39050, #67962, #90184, #10649, #60403, #39507, #81222, #3087, #16368, #89708, #32447, #74121, #80764, #24875, #82623, #67031, #37660, #9242, #53757, #17771, #66568, #3558, #30572, #38120, #48501, #34782, #20104, #84025, #5912, #5452, #83544, #70779, #48985, #12538, #39986, #47087, #33364, #84954, #4965, #11120, #18235, #33849, #48029, #77884, #69829, #41388, #75991, #62758, #13031, #68903, #62265, #41866, #63697, #76934, #40909, #4035, #19632, #70321, #77401, #47566, #56099, #18702, #55162, #32907, #25789, #4487, #34320, #61795, #54671, #92523, #63226, #54211, #76472, #11592, #91099, #83080, #12062, #40440, #90627, #69357, #26268, #19171, #91592, #26747, #55633, #84483, #92058, #27212, #20589, #66016, #14880, #43285, #57509, #43734, #36639, #49459, #64174, #14427, #6851, #71248, #73100, #49911, #42336, #29080, #13489, #57055, #78806, #57971, #86354, #85891, #87283, #22430, #86824, #21505, #44195, #28165, #21043, #36178, #6377, #28620, #13952, #21982, #65097, #78347, #93467, #7754, #197, #42809, #50856, #93006, #8229, #35726, #79738, #72182, #673, #71724, #35249, #80195, #72634, #56586, #37107, #7298, #64639, #65560, #85439, #29557, #50383, #79286, #27689, #58438, #51302, #15334, #80652, #30464, #52235, #2527, #30946, #59360, #60752, #89593, #60294, #88675, #17664, #1582, #88212, #9607, #15806, #2056, #23368, #89131, #38494, #22892, #66918, #74963, #67399, #81118, #31404, #37553, #46517, #9130, #24282, #81568, #67852, #16261, #44665, #53646, #53157, #30009, #10534, #45571, #8675, #82039, #58894, #45111, #59834, #10075, #39401, #23824, #17196, #16716, #46057, #75418, #24764, #52687, #1128, #38943, #74013, #87740, #82516, #2978, #73566, #51762, #38007, #31863, #74476, #66464, #32335, #19062, #62151, #5337, #83910, #26628, #90071, #47917, #34205, #61236, #76356, #63110, #19982, #90980, #55042, #25223, #33727, #55518, #91477, #61684, #70205, #3919, #69248, #54096, #39869, #18582, #62638, #82968, #68789, #91938, #84367, #55979, #32795, #90515, #47448, #84833, #26147, #25679, #27092, #48859, #12912, #46973, #11482, #77764, #68316, #18121, #54558, #4376, #75875, #3440, #19516, #76820, #33254, #48383, #77286, #11000, #83426, #40332, #11946, #40795, #69712, #4843, #12416, #41267, #7190, #50257, #63580, #13833, #21869, #79165, #42213, #14312, #78233, #58327, #49795, #64982, #28502, #14769, #28049, #85323, #554, #43172, #70663, #51190, #86236, #49339, #72073, #5792, #71127, #42684, #50744, #80077, #71603, #36065, #57394, #85, #22319, #7639, #6738, #87170, #86704, #6257, #41750, #36523, #28965, #27565, #34666, #20926, #72519, #21388, #92405, #56461, #57850, #35610, #65439, #79628, #43622, #20472, #29437, #13372, #35125, #78692, #64047, #92889, #64526, #56939, #85776, #93351, #2415, #38372, #8564, #17074, #44550, #16149, #36995, #80531, #59242, #74362, #72978, #15685, #74850, #31295, #2867, #73453, #37443, #88088, #31751, #66803, #66352, #38834, #67741, #53529, #87625, #23246, #89481, #9962, #65906, #1467, #45001, #8108, #15220, #60181, #30828, #73903, #89019, #24166, #1020, #51645, #1933, #52125, #58782, #60643, #30353, #29898, #16607, #22776, #81006, #9019, #45462, #37898, #59725, #24641, #44076, #9485, #88567, #67286, #23715, #52578, #81922, #81458, #53047, #45942, #83319, #46863, #3325, #17552, #39750, #18465, #54446, #54915, #68676, #47324, #91357, #33144, #26032, #39287, #69600, #19409, #25115, #76240, #75767, #33608, #83795, #46404, #89961, #10423, #18950, #70081, #26984, #61577, #53989, #90868, #25566, #11372, #75304, #48272, #47804, #62999, #40222, #76705, #68206, #69138, #62516, #4266, #62034, #77174, #3811, #11831, #40682, #4730, #32215, #90409, #26518, #61122, #55406, #84259, #12304, #82858, #18010, #10887, #41148, #32691, #5224, #34097, #91829, #82405, #86130, #43062, #65335, #50635, #35501, #79525, #27452, #56830, #56344, #71967, #7533, #85206, #36418, #50152, #57745, #42100, #48744, #71015, #13722, #20357, #64417, #86589, #21760, #35957, #49229, #7085, #64876, #85670, #93702, #14664, #439, #42575, #71490, #55873, #78125, #57288, #63933, #79050, #14201, #5683, #84725, #28858, #43519, #72417, #19874, #13263, #12799, #77648, #93243, #70559, #6147, #35019, #41641, #34557, #92771, #63466, #92295, #27939, #20818, #49688, #78583, #6621, #28396, #21279, #59132, #1359, #1825, #80425, #87976, #38258, #73799, #66697, #79970, #16499, #60074, #65800, #23127, #87516, #74253, #30711, #58219, #36885, #51082, #59610, #16963, #67634, #8458, #912, #37790, #66244, #30242, #22212, #88911, #88460, #9854, #52010, #23608, #87064, #80897, #9376, #16044, #44896, #24061, #44440, #52475, #81349, #8913, #43967, #37338, #45351, #15107, #67172, #2305, #31189, #29791, #72867, #58671, #52937, #73346, #81814, #7992, #45827, #22662, #74733, #38728, #29326, #51535, #15569, #91242, #68091, #3699, #3217, #18842, #48157, #32106, #77061, #90760, #4619, #82748, #89370, #17901, #54339, #61004, #76128, #33493, #62401, #76599, #89849, #47699, #11720, #32584, #40574, #26407, #41033, #83212, #18359, #2761, #25011, #4162, #10778, #25918, #54803, #46293, #31642, #83680, #55296, #84150, #19298, #53882, #53407, #60532, #40115, #17443, #46754, #75655, #12190, #24527, #39640, #82292, #69488, #61924, #75197, #47219, #10310, #61476, #11262, #68564, #39180, #90306, #25459, #69030, #33033, #50510, #35840, #91718, #63353, #70900, #62884, #14544, #57172, #85557, #6034, #86012, #78926, #26871, #12680, #56711, #49114, #19760, #21632, #92184, #84611, #71370, #55758, #5574, #27339, #6502, #34906, #34445, #64757, #93582, #35381, #63817, #86467, #70447, #56226, #78470, #48628, #92651, #85088, #64301, #13607, #77530, #41987, #50031, #42460, #20237, #93126, #41521, #79408, #78011, #28281, #20705, #42938, #13151, #27821, #28741, #21162, #5101, #69961, #49575, #14075, #71847, #33981, #6967, #57624, #52359, #52815, #15450, #80780, #59013, #37674, #23943, #9255, #73232, #88795, #88340, #72749, #59957, #38132, #1703, #29201, #36296, #22547, #74137, #87860, #317, #7414, #23009, #37227, #67047, #51888, #30586, #65213, #15930, #2183, #58099, #51421, #31069, #81695, #66132, #30129, #86947, #8795, #59488, #66583, #36760, #45232, #7870, #44321, #22099, #14992, #87400, #23492, #50969, #43851, #43399, #81235, #72294, #65680, #795, #80311, #79853, #16382, #29675, #8344, #58556, #1247, #44784, #73685, #31983, #47099, #83092, #10662, #31527, #89724, #18247, #45699, #91958, #54224, #39518, #82170, #9739, #24406, #17784, #60876, #61361, #89255, #24887, #75082, #76006, #5357, #27585, #12931, #90195, #41771, #17326, #46637, #46177, #34223, #63599, #10192, #92423, #11137, #20002, #3100, #38615, #53768, #68439, #39061, #25343, #48880, #77783, #27113, #67973, #63129, #55997, #75538, #84852, #70681, #56482, #3572, #32461, #16843, #82634, #41287, #70222, #5811, #34685, #60415, #74611, #67519, #2649, #53285, #65455, #20943, #13389, #87186, #14328, #71145, #13850, #85792, #7655, #20491, #78708, #42232, #102 ),
 ( #49811, #57867, #72089, #49357, #35143, #78251, #7206, #572, #85340, #57413, #42703, #28981, #86252, #21403, #92906, #58344, #86723, #6274, #36081, #21887, #64066, #56955, #43188, #28066, #71621, #43638, #36540, #64542, #6754, #35627, #93368, #50759, #28518, #79643, #29456, #65000, #14785, #72536, #50276, #79184, #76667, #42064, #63430, #63896, #40644, #11794, #26479, #92732, #34057, #47768, #6111, #34982, #20781, #54878, #55369, #56792, #70978, #4230, #69564, #77136, #69104, #76204, #92259, #91793, #12267, #27416, #85170, #33108, #18913, #62959, #84221, #25992, #27904, #4692, #90832, #77608, #61997, #33567, #62477, #12759, #41109, #91318, #85634, #11333, #41600, #70041, #40185, #19368, #48233, #84687, #83757, #5183, #26944, #70522, #19836, #55832, #48704, #56304, #5648, #34523, #20321, #49191, #78086, #13229, #72827, #36380, #22623, #35920, #93207, #8421, #22176, #78547, #59095, #397, #57251, #51044, #13685, #50112, #50595, #58634, #87936, #21720, #87025, #65293, #43930, #30204, #15527, #79489, #1322, #874, #79007, #66206, #44402, #7952, #35463, #42537, #28823, #80385, #29287, #6585, #71448, #58183, #43482, #73310, #79932, #36847, #64382, #15068, #28359, #86093, #21243, #65764, #37300, #49653, #57706, #14162, #29753, #86549, #14624, #43026, #71929, #87475, #7051, #72378, #51497, #64838, #7495, #93663, #52896, #74696, #17864, #38218, #53367, #89332, #16925, #37751, #2267, #24487, #51969, #3180, #60495, #45784, #88422, #16006, #30669, #24022, #67133, #67598, #1786, #31150, #81313, #82253, #10273, #32548, #46716, #2726, #75618, #23571, #81775, #52438, #39142, #68522, #16459, #3659, #17408, #24973, #9335, #44858, #60036, #9818, #45311, #31606, #53847, #82713, #32064, #74216, #68053, #60959, #38691, #89811, #10742, #61441, #46256, #75160, #23087, #88873, #39599, #80859, #73761, #8873, #66659, #59572, #77492, #49078, #56191, #77977, #47661, #47179, #34871, #33944, #11223, #40536, #83639, #20199, #54300, #11685, #76089, #19722, #55722, #83173, #40998, #63317, #55258, #90271, #25422, #91200, #54762, #40078, #18323, #76562, #26369, #62359, #62849, #69451, #84113, #5539, #69921, #91683, #68995, #12637, #27303, #32997, #19263, #18803, #41484, #26834, #4126, #61888, #90720, #84574, #13118, #25881, #4581, #33456, #5061, #48121, #77025, #12153, #85050, #48592, #70867, #70414, #34410, #92148, #41954, #5998, #93549, #21595, #58527, #78892, #288, #36265, #57592, #78438, #42901, #65185, #92614, #43820, #7384, #86436, #35343, #56678, #71336, #64722, #14039, #14515, #42424, #71815, #28250, #29169, #50941, #73196, #87372, #43370, #22520, #64267, #28707, #93096, #79823, #15421, #57138, #44289, #58064, #65649, #49997, #85526, #6935, #50475, #85979, #72266, #763, #29648, #72719, #21129, #14964, #7842, #79378, #36729, #51391, #8316, #86918, #22071, #63784, #35808, #80282, #27784, #20672, #49543, #13574, #6466, #24380, #89694, #3074, #24861, #88307, #87831, #75512, #74580, #51856, #81209, #30558, #60852, #1217, #52331, #22982, #60390, #2623, #30101, #81668, #10168, #2152, #37198, #66106, #38107, #1676, #80748, #58983, #23465, #67017, #9227, #9708, #16354, #31042, #46153, #16815, #38589, #15900, #53258, #67950, #73657, #59932, #59456, #82141, #88771, #31958, #52789, #89228, #44757, #45674, #53744, #8768, #45205, #82610, #17757, #23918, #67492, #37646, #31501, #17297, #75057, #74107, #39037, #66555, #46610, #32433, #75977, #54655, #69812, #68415, #11105, #70306, #91575, #92041, #68886, #39971, #83529, #27195, #62247, #4017, #34304, #63210, #48968, #83066, #18688, #84935, #5437, #61333, #32892, #11576, #3545, #10634, #26731, #26253, #40425, #55618, #19617, #90170, #47070, #91082, #47551, #54197, #56083, #61779, #25318, #12047, #18220, #90612, #25773, #40894, #69342, #76456, #20087, #39493, #4948, #4473, #33350, #55147, #84009, #19157, #48013, #76918, #33834, #62743, #84466, #48485, #77384, #12522, #41372, #78331, #50365, #20571, #655, #85874, #7281, #64622, #50838, #64156, #27672, #36618, #79268, #13014, #87265, #28602, #85423, #14409, #41850, #13472, #13932, #86807, #22410, #49894, #21485, #93448, #72165, #58418, #43716, #42790, #29539, #29060, #71231, #77864, #72615, #36158, #63680, #70763, #57036, #14863, #57492, #34766, #5895, #86335, #49443, #43267, #21025, #71707, #92504, #7737, #65080, #56570, #6834, #179, #6357, #35708, #57952, #21964, #79721, #65540, #92989, #35231, #28147, #45091, #65997, #30444, #23804, #80175, #31383, #88655, #73992, #22871, #44172, #58873, #52215, #66442, #2034, #29990, #1561, #15785, #81547, #38472, #60732, #46037, #30924, #74942, #51736, #81098, #80629, #67376, #2957, #44644, #31842, #45551, #53135, #37531, #73079, #59336, #9110, #73545, #59814, #82016, #17173, #60273, #8654, #2505, #89109, #16241, #24261, #10052, #89571, #37986, #66894, #51282, #88188, #52667, #23347, #74451, #9584, #1108, #15313, #38922, #67831, #8210, #37088, #16695, #87720, #22643, #20451, #91457, #27073, #70184, #7972, #40775, #91918, #33705, #7513, #42193, #69693, #27546, #51062, #41731, #76800, #11926, #77742, #41242, #26608, #4822, #34186, #12893, #48836, #49318, #63090, #70645, #87044, #56438, #78213, #62617, #65312, #15087, #19497, #5773, #5318, #29306, #13352, #55499, #84348, #48363, #71105, #65781, #77267, #55959, #36398, #12396, #84813, #43947, #419, #890, #19963, #34647, #63558, #29773, #92386, #85302, #36866, #58652, #58200, #22193, #79949, #87494, #72844, #73328, #44877, #52457, #44422, #89833, #38710, #67153, #81331, #67617, #60516, #8439, #87955, #38239, #30691, #1340, #3200, #73779, #66226, #52917, #37318, #80879, #8894, #81796, #16478, #16026, #17427, #46276, #16944, #45334, #68075, #51991, #37772, #60055, #30223, #74235, #66678, #45808, #88893, #59114, #23590, #31625, #24042, #1805, #74717, #23108, #32084, #59591, #9837, #2286, #24508, #88441, #9355, #10293, #2745, #80403, #60985, #31169, #89352, #53390, #15550, #82275, #75180, #39163, #51515, #90743, #62379, #40557, #19283, #5560, #84594, #54783, #70434, #69941, #54320, #41506, #19744, #77044, #10762, #17884, #4146, #55742, #69471, #75639, #82732, #4603, #18826, #48612, #33476, #12175, #46736, #91224, #77512, #39620, #33017, #12661, #34431, #47681, #11705, #68544, #84133, #41018, #48142, #18343, #26854, #83195, #25901, #3683, #90291, #69015, #63337, #83662, #26391, #55279, #5084, #24994, #53866, #76582, #32568, #33965, #47198, #61460, #25443, #62869, #76112, #11245, #61908, #40099, #91702, #49100, #56211, #42922, #85999, #29185, #14058, #50494, #20222, #71836, #58082, #85070, #6486, #86935, #43836, #21148, #78911, #77998, #57610, #79395, #21611, #85544, #305, #27805, #93114, #13138, #63804, #42445, #86453, #41974, #92633, #22087, #14531, #79840, #56698, #20692, #71355, #14980, #50018, #49562, #50957, #72738, #36745, #70888, #35365, #7858, #92168, #6018, #78457, #28269, #34893, #27325, #43386, #6954, #57158, #72281, #7401, #13593, #64286, #35827, #64741, #93568, #28725, #36282, #65202, #67032, #51408, #1235, #22998, #2168, #1692, #30117, #31517, #60405, #31057, #59471, #82157, #66121, #59000, #74122, #80300, #66570, #87849, #59944, #9243, #87389, #37662, #45688, #38121, #51873, #88784, #8333, #17313, #73673, #23932, #52347, #38604, #80766, #15440, #24396, #52804, #781, #75070, #16369, #73217 ),
 ( #16831, #81682, #29664, #37214, #22536, #74596, #53273, #10182, #44773, #15918, #9725, #8784, #30574, #58544, #89243, #67508, #46167, #88326, #2638, #44306, #23480, #65667, #81223, #45220, #33850, #54212, #69358, #11593, #32908, #53758, #18236, #40441, #67963, #19172, #76473, #61796, #10650, #31973, #46627, #39987, #83081, #83545, #17772, #47088, #3559, #4488, #26269, #48502, #62759, #18703, #91593, #39508, #68904, #68429, #55163, #84484, #32448, #19633, #33365, #40910, #25333, #60866, #75992, #90628, #61351, #47567, #69830, #4966, #48030, #90185, #84027, #76935, #4036, #12063, #26748, #77402, #25790, #54672, #39051, #11121, #62266, #91100, #55634, #3088, #82624, #89709, #24876, #75527, #72183, #198, #63698, #63227, #50857, #49912, #27213, #56587, #5913, #36179, #70322, #27690, #92059, #35727, #71725, #5453, #57056, #79287, #71249, #12539, #34321, #85892, #14428, #6378, #41389, #56100, #13490, #70780, #84955, #20105, #92524, #42337, #78348, #78807, #85440, #35250, #21506, #21044, #13953, #48986, #93468, #43286, #77885, #64175, #34783, #57510, #42810, #13032, #41867, #20590, #6852, #29081, #49460, #93007, #28166, #64640, #28621, #86355, #50384, #7299, #65098, #86825, #57972, #21983, #14881, #44666, #30947, #15808, #37554, #74477, #1129, #16262, #52237, #73567, #674, #58895, #81119, #43735, #59835, #23369, #8676, #51303, #72635, #87284, #80653, #30010, #30465, #58439, #87741, #44196, #45112, #66919, #89132, #9608, #59361, #38495, #80196, #66465, #15335, #2057, #31406, #73102, #60295, #74014, #81569, #66017, #7755, #22893, #1583, #8230, #88213, #16717, #45572, #88677, #37108, #23825, #52688, #9131, #67400, #2528, #24283, #38008, #79739, #36640, #51763, #65561, #29558, #22431, #11483, #2979, #53158, #40333, #11947, #19063, #40796, #10536, #10076, #91478, #90516, #67854, #3441, #46518, #76821, #17197, #68317, #38944, #76357, #18583, #25224, #25680, #68790, #47449, #33728, #47918, #82969, #4844, #4377, #82517, #69713, #62640, #69249, #31864, #46058, #32336, #83911, #3920, #60753, #74964, #32796, #46975, #82040, #61685, #33255, #89594, #54559, #24765, #53647, #61237, #17665, #75419, #75876, #39870, #39402, #62152, #90981, #26149, #90072, #55043, #54097, #18122, #11001, #83428, #70664, #85777, #84368, #27093, #86237, #13834, #14313, #84834, #55980, #5793, #43173, #78234, #91939, #50258, #79166, #64983, #5339, #34667, #7191, #21389, #48384, #19983, #27566, #19517, #26629, #42685, #42214, #56463, #71604, #35612, #77287, #63111, #13373, #63581, #70206, #72075, #48860, #41268, #28050, #12417, #77765, #12913, #56940, #85324, #41752, #36066, #55519, #20927, #20473, #34206, #92406, #49340, #35126, #71128, #6258, #64048, #49796, #92891, #78693, #6739, #64527, #93352, #28503, #57395, #36524, #16608, #8109, #23247, #80532, #66804, #80078, #43623, #52579, #66353, #28966, #9486, #44551, #7640, #1468, #57851, #555, #1021, #9020, #38373, #52126, #21870, #73454, #30829, #86705, #36996, #59726, #45463, #87627, #15686, #50745, #59243, #81007, #16150, #87171, #1934, #29438, #29899, #79629, #65440, #44077, #88089, #14770, #58328, #88568, #45002, #81459, #22320, #51191, #72979, #74363, #51646, #15221, #23716, #86, #72520, #65907, #58783, #22777, #8565, #37444, #30354, #73904, #37899, #11832, #54447, #82859, #3326, #83320, #76241, #60182, #9963, #53990, #46405, #17075, #18951, #89482, #81923, #68677, #53048, #2868, #24642, #3812, #32216, #31752, #33145, #62035, #32692, #61123, #83796, #67742, #60644, #75768, #45943, #68207, #53530, #61578, #10888, #89020, #39288, #47325, #39751, #82406, #90410, #38835, #47805, #75305, #25567, #18011, #40223, #17553, #74851, #26033, #18466, #2416, #76706, #46864, #10424, #11373, #31296, #89962, #25116, #69139, #67287, #4267, #90869, #54916, #24167, #21280, #6622, #70560, #86131, #85671, #70082, #57289, #35502, #92772, #26519, #33609, #19875, #71491, #85207, #91358, #4731, #20358, #34558, #64418, #56345, #69601, #5684, #20819, #63467, #92296, #93244, #55874, #71016, #13264, #27453, #55407, #48745, #42101, #62517, #49689, #78126, #49230, #12305, #84260, #48273, #41642, #84726, #6148, #19410, #77649, #5225, #35020, #27940, #50153, #28397, #63934, #79051, #41149, #56831, #34098, #78584, #40683, #63000, #77175, #13723, #42576, #26985, #91830, #12800, #65801, #43520, #87517, #44897, #73800, #87977, #7534, #59133, #23129, #43968, #52011, #8914, #52476, #913, #29792, #14202, #72418, #15571, #22213, #37339, #66245, #57746, #43063, #1360, #66698, #37791, #1826, #65336, #64877, #71968, #51536, #28859, #58220, #36419, #30713, #7086, #29327, #93703, #30243, #73347, #35958, #58672, #80898, #72868, #86591, #21761, #15108, #441, #50636, #79526, #87065, #7993, #79971, #80426, #51083, #36886, #16045, #22663, #44441, #14665, #59611, #88461, #8459, #23609, #45830, #33862, #84038, #16500, #88912, #9378, #55178, #70337, #27226, #60533, #24062, #91113, #24528, #53409, #74254, #48513, #26282, #63241, #10311, #76948, #3218, #40923, #38260, #62278, #19645, #45352, #89371, #77414, #34335, #75198, #68092, #67173, #48043, #69843, #12075, #74734, #84499, #16964, #82293, #2306, #52938, #31643, #4977, #31190, #81815, #12552, #62773, #5464, #9855, #38729, #17444, #92072, #39181, #67635, #41402, #81350, #60075, #2762, #46294, #32107, #19183, #91605, #26761, #55646, #49000, #691, #43301, #71740, #85906, #72198, #65113, #77899, #92536, #42825, #35262, #5926, #7772, #78362, #70791, #57525, #41880, #85454, #13502, #86370, #21058, #20602, #22001, #50872, #21521, #49925, #72650, #56600, #49472, #64654, #34796, #57068, #42350, #50399, #93483, #13043, #28178, #36194, #28636, #71263, #79304, #27702, #36656, #64188, #14445, #6867, #29096, #6391, #63711, #14895, #7315, #84966, #65577, #35741, #93021, #216, #20117, #78822, #13967, #57989, #56114, #86842, #79754, #43750, #23843, #10095, #89154, #59379, #74983, #74496, #58911, #46077, #24303, #81590, #15351, #22446, #8694, #60316, #74033, #80211, #87300, #9150, #23387, #53180, #2075, #66034, #38963, #37574, #52709, #16281, #2548, #15826, #73118, #82059, #30966, #58456, #67875, #38028, #37126, #59854, #51319, #30028, #30484, #38514, #29575, #1601, #66937, #45132, #16738, #44211, #17216, #88231, #8245, #9628, #87757, #1147, #22910, #45594, #51781, #80670, #66485, #44683, #88695, #73585, #52256, #67419, #81137, #31427, #18605, #55063, #24785, #76377, #33749, #60774, #11021, #62661, #48404, #90536, #83450, #89614, #62172, #83932, #26172, #90092, #4866, #32357, #3942, #53667, #68339, #46995, #91003, #82536, #3462, #91495, #19084, #84389, #61257, #25244, #75897, #19538, #54579, #54118, #26650, #55540, #41290, #75439, #39891, #77307, #12439, #17685, #82991, #32815, #46537, #2998, #47938, #47470, #61705, #76841, #11968, #10557, #39422, #11503, #68812, #18141, #31884, #25697, #40352, #4398, #69269, #33275, #40816, #69733, #49360, #41774, #28522, #57417, #85795, #13392, #79188, #77786, #12934, #92909, #27116, #20493, #70684, #20946, #28069, #63132, #78254, #71624, #56958, #5814, #34688, #50280, #86256, #78711, #56000, #34226, #27588, #93372, #35146, #91961, #5360, #64069, #42235, #21407, #6277, #13853, #84855, #49814, #14332, #20005, #56485, #43192, #72092, #71148, #42706, #48883, #6757, #35630, #64546, #63602, #70225, #92426, #85343, #82821 ),
 ( #5650, #48236, #76669, #90834, #77138, #70043, #53954, #3771, #47770, #40187, #10850, #12761, #83285, #75728, #62479, #46826, #90377, #18430, #91320, #25994, #25533, #26946, #55835, #26481, #54880, #77610, #61544, #54413, #69566, #39715, #61999, #47288, #55371, #4694, #17974, #33111, #41111, #33569, #76206, #84223, #32656, #41602, #69106, #19370, #11796, #34059, #11335, #68639, #19838, #12269, #89924, #70524, #40647, #4232, #5185, #25080, #83759, #18915, #62961, #61082, #91795, #84690, #48706, #28825, #15071, #399, #64384, #79934, #79491, #35465, #56306, #6113, #78550, #93666, #92261, #34984, #29289, #21722, #22178, #92734, #63898, #13687, #51046, #86096, #27906, #58185, #87027, #72829, #13231, #42539, #43932, #34525, #85172, #56794, #93209, #27418, #63433, #50598, #50114, #28361, #14626, #43484, #20323, #70981, #21245, #71450, #78088, #49193, #85636, #42066, #35922, #20783, #49655, #6587, #64840, #57253, #79009, #14164, #43028, #57708, #71931, #7053, #86551, #72380, #7497, #36382, #65295, #37302, #67135, #16461, #29755, #73763, #81777, #45314, #8423, #74218, #44404, #24489, #16008, #31152, #88424, #74698, #87938, #51499, #60498, #9337, #36849, #17410, #52440, #15529, #38220, #65766, #66208, #8875, #16927, #46258, #37754, #2269, #23573, #60038, #82255, #67600, #66661, #53369, #52899, #1324, #7954, #2728, #88875, #87477, #876, #80861, #38693, #81315, #58636, #22626, #24024, #1788, #31608, #45786, #9820, #80387, #89334, #73312, #30207, #44860, #59097, #23089, #30671, #51971, #59574, #40538, #62361, #4584, #68524, #77027, #10744, #33458, #3182, #54764, #12156, #39145, #83176, #41000, #26836, #68997, #61890, #68056, #69453, #91202, #26371, #3661, #69923, #39602, #76091, #32066, #46718, #25424, #55260, #60961, #75621, #5063, #84115, #62851, #32550, #61443, #54302, #91685, #32999, #90273, #33946, #55724, #19725, #53849, #18325, #84576, #75162, #89813, #47181, #11225, #24975, #10275, #19265, #90723, #40080, #48123, #82715, #17866, #4128, #25883, #83641, #18805, #47663, #76564, #11687, #50000, #34412, #77979, #6000, #78894, #78440, #13120, #14517, #43372, #14041, #42427, #65187, #49080, #41956, #57140, #63319, #49545, #70869, #42903, #85981, #70416, #20674, #28709, #21131, #34874, #71817, #85052, #290, #56680, #6937, #35345, #21597, #63786, #92150, #7386, #35810, #77494, #58066, #28252, #56193, #64724, #12639, #92616, #13576, #57594, #86920, #71338, #93551, #64269, #86438, #29171, #36267, #6468, #48594, #50477, #27786, #41486, #5541, #79380, #27306, #20201, #1220, #52790, #66556, #72722, #79825, #1677, #15902, #81669, #37648, #22522, #88308, #58530, #38590, #30103, #45207, #8769, #88772, #8318, #65651, #74582, #23466, #50943, #31502, #30559, #29650, #52332, #14966, #51394, #22984, #31043, #60391, #87833, #59457, #81210, #16355, #2624, #16817, #51858, #67493, #67018, #80284, #22073, #45675, #74109, #7844, #43822, #58985, #9709, #9228, #36731, #765, #38108, #44759, #87374, #2153, #59933, #15424, #23919, #44291, #73198, #80750, #37200, #66108, #73659, #75978, #53260, #54656, #76457, #18689, #82611, #91083, #24862, #90171, #17298, #60853, #39494, #83530, #82142, #89696, #55148, #11578, #76919, #53745, #17758, #68416, #12048, #47071, #46611, #19158, #48015, #33835, #3075, #3546, #69813, #84010, #46154, #75513, #25319, #75058, #89229, #40426, #11106, #54198, #69343, #4474, #10169, #31959, #39973, #32435, #39038, #40895, #10635, #61334, #90613, #83067, #18221, #68888, #25774, #4018, #32893, #4949, #24381, #47552, #61780, #33351, #62248, #26254, #71232, #48486, #63682, #92042, #28148, #6359, #84468, #34767, #42792, #35232, #64157, #92505, #27197, #28603, #57493, #57037, #56571, #79270, #63211, #56084, #92990, #77385, #27673, #84936, #85875, #21026, #19618, #85424, #71708, #49895, #20088, #78790, #5438, #14410, #70764, #13933, #49444, #35709, #48969, #12523, #21486, #6835, #91576, #72166, #13473, #70307, #64623, #26732, #77865, #20572, #93449, #7282, #78332, #86336, #42321, #50366, #43268, #62744, #55619, #41373, #34305, #13015, #41851, #5896, #88190, #21967, #29062, #15315, #66896, #80631, #86809, #181, #15787, #29992, #2036, #51738, #23349, #57954, #44646, #30926, #50840, #44174, #59816, #81549, #58875, #22873, #79723, #1563, #52217, #59338, #29541, #37988, #65542, #37090, #14865, #7739, #80177, #30446, #43718, #36620, #88657, #81100, #23806, #657, #58421, #73081, #52669, #87722, #87267, #16698, #45553, #74453, #72617, #8212, #36159, #65081, #22413, #51284, #65999, #1111, #73547, #16243, #8656, #37534, #45093, #73995, #66444, #9112, #90051, #82498, #53138, #55021, #31845, #24263, #10978, #89111, #38925, #60734, #83891, #32314, #3900, #38474, #68298, #54539, #39383, #61217, #4357, #24746, #39848, #75856, #3419, #82018, #17646, #68771, #67378, #83407, #46954, #25204, #74945, #2507, #17176, #10513, #53628, #54077, #46040, #46497, #67834, #32777, #90497, #19042, #33233, #82947, #62130, #10055, #18100, #2959, #25656, #47898, #89574, #9586, #61665, #11462, #75400, #31385, #18559, #47426, #76336, #40313, #69228, #90961, #26125, #60275, #44360, #8382, #29243, #73270, #87896, #37713, #51005, #43890, #93168, #57663, #833, #7454, #22584, #51458, #42981, #28320, #80347, #51927, #59049, #80817, #50549, #50070, #57209, #36801, #14117, #43439, #86510, #23049, #86050, #14582, #78966, #15489, #58597, #21199, #72786, #66168, #58138, #71886, #7008, #356, #21673, #35880, #64797, #79446, #86984, #65250, #65722, #72335, #22137, #37262, #7911, #29715, #93621, #1284, #30166, #28779, #79892, #36336, #15966, #87438, #44820, #73723, #8835, #39099, #54258, #11175, #45742, #74176, #75121, #9778, #38653, #59530, #32500, #10231, #53326, #39555, #52857, #16421, #25378, #68011, #1742, #76046, #17366, #9293, #3140, #30629, #67091, #67557, #75577, #66619, #2686, #32021, #82211, #60919, #47134, #61397, #31566, #18279, #17820, #2224, #83128, #90229, #24927, #52398, #88379, #74653, #3613, #46217, #23529, #81275, #89765, #60457, #45273, #53804, #82672, #38176, #46674, #31108, #59995, #89292, #88834, #23984, #24446, #10698, #81735, #68477, #16884, #63273, #33414, #41911, #69407, #40956, #61847, #11642, #84069, #5495, #4083, #40489, #5956, #27260, #27739, #4538, #62314, #19219, #56635, #91640, #91154, #63741, #92568, #78392, #18758, #48077, #20632, #34830, #90678, #26320, #69877, #32954, #40036, #56147, #55680, #5016, #85001, #49036, #25838, #76519, #26794, #76982, #83595, #85485, #55215, #54718, #41438, #47616, #12111, #33898, #70370, #62805, #84531, #49502, #68952, #34368, #19678, #48547, #77448, #12592, #92106, #20155, #77932, #13075, #70824, #22030, #35296, #79338, #87328, #50899, #13998, #79783, #49958, #30057, #21550, #36685, #80241, #72228, #51811, #13533, #14473, #71773, #28209, #42381, #64683, #43331, #7342, #14925, #93509, #36223, #22477, #58021, #43779, #64223, #720, #44241, #78849, #65142, #6896, #58484, #72680, #71294, #21088, #93053, #7799, #1175, #6421, #86397, #42858, #65607, #50434, #243, #57097, #73151, #29606, #87790, #29125, #51350, #85937, #86876, #15378, #8275, #37155, #66063, #28666, #58940, #22939, #35770, #57552, #59886, #53211, #15855, #60806, #24334, #9663, #52287, #73614, #88265, #81623, #2109, #31456, #59411, #30999, #45163, #17250, #67905, #90124, #75467, #60345 ),
 ( #25275, #38547, #2578, #80704, #74063, #82091, #88726, #10126, #38992, #30514, #44713, #3029, #39451, #46569, #68368, #38061, #37602, #8725, #46110, #1633, #23874, #9182, #10589, #66513, #52741, #23422, #31914, #75014, #81167, #89183, #16311, #16771, #66970, #45625, #74530, #67450, #89646, #24816, #53700, #82567, #17715, #3497, #32389, #61289, #12349, #42624, #86179, #91875, #20407, #19919, #6676, #56879, #83021, #63044, #77221, #27988, #43111, #27, #34606, #27029, #63985, #92344, #27499, #48320, #21330, #92825, #36006, #78172, #49736, #18174, #49277, #35553, #85259, #13310, #50200, #70604, #85720, #20865, #42148, #70136, #63516, #78633, #41198, #64466, #13775, #71066, #55918, #5272, #84770, #56397, #5731, #6198, #34141, #35065, #48791, #71543, #93293, #64924, #79104, #28444, #14253, #77699, #57337, #12848, #72018, #7135, #41686, #54152, #23183, #30764, #15161, #21811, #44020, #80471, #58272, #8506, #59666, #88509, #8961, #22264, #73845, #37840, #58722, #66746, #23656, #67227, #15620, #44492, #28906, #87114, #30294, #36938, #52066, #80948, #72463, #57794, #16093, #81398, #52522, #16546, #80021, #79571, #86644, #66295, #43567, #72917, #51138, #45402, #50685, #8044, #14714, #44945, #88026, #7582, #73396, #1872, #87566, #36467, #29839, #65382, #494, #65852, #74301, #29378, #960, #9425, #38312, #22711, #51585, #37385, #1407, #59182, #53928, #67682, #25966, #54847, #40619, #74787, #46343, #76642, #61970, #24108, #89420, #3264, #88961, #2358, #83260, #17948, #32154, #18404, #11309, #52989, #38778, #82796, #75245, #45881, #47744, #24574, #17012, #3747, #81863, #31690, #53462, #32629, #61055, #60585, #90807, #83729, #61519, #89898, #18889, #2809, #82343, #10826, #9904, #25056, #17491, #90350, #39686, #10360, #68143, #76177, #68610, #39225, #25506, #46799, #11767, #75702, #54384, #47263, #69078, #40161, #4206, #31236, #33081, #60122, #78980, #20293, #77107, #70952, #33541, #70009, #70495, #78522, #14132, #41573, #13202, #85138, #63870, #50085, #35434, #5623, #21215, #20755, #5152, #86065, #64356, #27874, #55344, #62446, #48678, #6555, #49167, #26455, #91289, #78060, #63404, #93182, #42038, #56767, #84196, #6084, #28334, #19343, #77579, #57224, #69535, #92233, #56279, #48205, #34958, #85608, #92704, #62933, #71423, #34029, #41085, #34498, #91767, #49626, #4668, #26919, #12238, #13659, #55806, #84658, #19810, #12730, #27389, #42511, #22597, #73737, #8849, #23063, #36351, #87912, #51941, #72801, #80831, #37727, #81290, #848, #58610, #42997, #7468, #44373, #51019, #66181, #1298, #86523, #71903, #30180, #1758, #66633, #30645, #371, #93636, #7023, #80361, #57680, #86999, #65265, #59544, #35894, #58153, #28793, #59064, #8397, #64812, #87451, #15982, #7925, #21688, #50565, #43904, #29257, #79462, #14596, #22151, #36816, #15044, #15502, #79906, #65737, #44834, #51472, #73284, #43453, #88394, #23545, #72350, #29729, #37275, #52415, #17839, #45288, #23999, #38192, #82689, #4099, #54736, #89307, #52872, #24944, #53342, #82227, #9310, #76063, #53821, #90694, #39116, #10716, #74191, #75137, #61414, #46233, #68029, #11192, #31583, #46691, #75593, #10247, #31124, #24463, #39573, #67106, #90246, #68495, #3156, #81751, #2240, #16901, #17381, #60472, #60934, #88850, #32039, #74669, #3630, #32518, #25854, #40052, #89781, #68969, #45759, #32970, #61863, #16436, #9793, #25395, #60010, #38668, #67572, #2701, #54275, #83145, #18296, #47154, #5515, #19695, #70841, #92588, #76537, #26340, #70387, #62824, #33430, #35315, #12128, #4556, #85021, #69425, #19238, #40974, #20173, #48564, #48095, #49519, #78411, #49053, #77467, #6440, #84088, #76999, #92123, #62334, #84548, #69896, #77949, #27277, #11659, #55697, #63758, #56164, #5035, #13092, #55233, #64240, #91658, #41930, #34385, #56653, #33915, #91174, #42399, #5974, #18775, #93071, #63290, #26811, #34847, #47633, #12610, #41455, #27757, #28225, #85502, #20649, #13550, #71310, #83614, #40506, #86892, #8744, #8292, #86412, #73633, #22956, #15395, #42875, #49973, #36240, #87807, #7815, #14015, #21105, #36705, #50915, #51830, #72696, #44262, #78865, #65626, #80723, #71788, #65158, #15876, #37621, #79799, #43796, #6910, #22495, #73173, #80259, #50451, #58959, #21568, #58040, #35785, #28683, #7358, #51368, #64698, #57569, #44732, #37173, #66532, #79353, #14488, #261, #1651, #14941, #93524, #66081, #1193, #30074, #43346, #57113, #72243, #22046, #29144, #738, #29623, #85953, #58501, #87346, #90142, #17732, #18192, #88746, #59904, #74552, #47044, #82111, #2128, #54170, #83039, #68860, #9201, #9683, #11075, #25292, #52307, #23892, #31476, #23439, #30531, #46587, #46128, #60364, #75485, #39468, #81184, #66990, #17270, #38565, #74082, #75945, #52761, #45180, #31932, #16330, #81642, #16789, #60823, #89202, #45643, #39944, #59433, #89666, #24354, #88284, #31017, #67467, #39010, #38079, #53229, #2596, #24835, #67924, #75031, #10144, #10610, #3048, #53718, #82585, #68385, #3516, #32408, #61306, #84438, #70732, #83982, #47524, #56538, #70276, #32864, #13442, #48455, #11550, #5409, #61753, #4443, #4915, #12983, #42289, #69784, #41342, #19586, #92012, #78303, #63651, #33801, #49413, #48935, #33323, #20543, #92473, #56052, #83499, #90585, #76888, #34735, #77356, #54627, #25746, #12490, #91545, #27639, #34274, #84906, #18657, #63181, #85395, #76429, #12016, #3989, #40397, #26701, #27164, #69315, #62220, #62715, #91049, #77835, #20054, #26223, #55117, #19130, #41821, #47985, #40866, #55590, #5865, #79691, #14379, #43239, #64124, #37059, #14833, #51709, #149, #65503, #6328, #36129, #22380, #7253, #29029, #65969, #86305, #7705, #43687, #65046, #85844, #50330, #72583, #35196, #51253, #36589, #57916, #42756, #92960, #78761, #72137, #21457, #21934, #49862, #79237, #35680, #622, #58389, #80597, #1080, #50806, #29960, #71673, #86773, #6807, #87232, #22842, #64595, #15754, #29507, #73045, #57462, #28119, #80143, #15283, #93420, #44140, #8175, #58846, #87689, #28572, #71201, #57007, #20996, #13902, #39348, #82918, #2478, #60243, #44614, #9078, #46007, #52639, #67802, #2927, #88155, #73518, #31812, #3389, #10482, #32277, #2000, #1530, #8627, #81985, #59307, #88627, #37958, #68267, #37504, #59786, #30416, #60705, #10023, #66413, #89081, #17614, #9552, #23314, #52187, #45521, #66865, #81068, #16213, #30893, #74423, #16666, #17141, #23774, #38439, #53594, #24230, #74912, #45064, #89545, #73964, #67348, #81519, #31355, #53107, #38893, #24708, #82467, #61183, #46465, #90021, #75368, #25174, #54048, #34623, #69665, #83382, #41704, #70621, #56415, #90471, #62100, #92360, #77715, #39817, #11433, #19016, #10951, #18072, #5289, #33676, #47868, #34159, #27045, #68740, #54510, #4797, #90933, #61638, #63533, #40284, #32750, #19470, #3871, #47396, #69201, #48337, #76771, #76307, #12865, #5748, #77238, #11899, #27522, #18530, #4330, #26581, #25628, #40748, #33207, #12368, #55470, #26098, #83863, #91891, #84319, #54987, #41216, #62585, #46925, #91427, #70153, #63062, #84788, #55933, #19938, #75827, #48808, #20424, #2256, #36025, #92841, #86662, #49293, #85736, #86196, #513, #31139, #57355, #28923, #7150, #79589, #67121, #51153, #21348, #38207, #36483, #20882, #9324, #80037, #43583, #71083, #78188, #64484, #22281, #64942, #42168, #13326, #43, #79123, #15178, #57811 ),
 ( #43130, #49754, #21826, #44036, #72938, #65400, #78651, #29395, #58287, #50219, #87130, #85274, #6215, #72035, #50701, #35084, #13791, #14730, #93311, #72481, #7596, #64003, #28004, #56897, #42643, #71560, #6695, #35570, #28461, #14270, #3646, #74683, #10262, #53356, #83629, #24012, #75150, #16915, #83161, #25411, #52885, #10732, #32987, #24961, #4572, #60026, #60948, #24477, #9807, #88863, #17397, #89798, #32054, #32537, #46246, #53837, #68985, #39588, #61430, #45773, #47169, #90709, #2716, #82703, #82241, #11209, #90262, #81765, #67586, #38681, #54290, #47650, #31596, #39132, #60485, #68511, #3170, #17854, #89322, #25870, #18313, #40524, #46705, #76078, #68043, #75608, #40067, #4115, #61878, #54752, #18791, #76552, #11675, #69442, #48112, #12625, #5989, #62349, #13564, #70857, #56180, #5050, #26357, #40989, #34400, #48582, #77965, #12144, #77482, #91673, #63774, #20662, #42890, #28240, #13108, #57127, #33932, #63307, #62840, #56667, #20188, #6455, #19711, #77016, #85969, #34861, #91190, #71803, #41945, #69911, #92603, #55248, #26826, #92138, #42414, #33446, #5530, #27773, #49068, #85516, #14029, #93085, #27293, #78881, #78426, #55713, #49987, #21119, #49533, #19254, #84105, #41471, #64256, #71325, #84564, #70403, #35330, #85038, #58974, #36721, #15412, #93539, #754, #87823, #35799, #86907, #22973, #44747, #43811, #7833, #64712, #22512, #44280, #73188, #7374, #30091, #43361, #50931, #28698, #14504, #29159, #51383, #57583, #72257, #51845, #8307, #80740, #36255, #65174, #58056, #15891, #65640, #279, #73649, #8759, #6925, #22062, #14956, #86427, #21583, #79815, #72711, #29638, #58517, #50465, #79368, #87362, #80274, #37189, #66097, #1209, #34239, #78269, #70698, #41302, #43204, #20019, #12454, #92923, #77321, #27129, #48897, #28084, #27603, #56012, #57429, #86270, #56972, #85359, #14345, #91975, #84869, #6293, #70239, #92440, #77799, #85810, #35162, #19551, #63615, #71637, #64084, #12949, #20960, #63145, #72105, #5829, #6769, #84402, #41787, #13408, #34701, #5372, #7222, #56500, #20507, #49828, #49376, #42251, #71164, #78725, #13867, #42720, #21422, #50296, #35644, #64561, #36096, #93385, #28538, #79202, #91508, #26664, #55553, #48417, #73483, #86739, #37024, #45031, #8595, #65472, #37472, #7673, #81488, #73012, #88121, #51676, #37925, #51220, #14800, #23743, #66382, #116, #74390, #15719, #72551, #1498, #28997, #589, #65938, #73931, #9518, #1049, #30382, #80565, #59275, #45489, #30860, #29928, #16635, #16179, #29472, #65016, #59754, #23278, #50774, #57883, #44109, #1968, #44580, #21901, #79659, #52153, #58813, #88594, #81035, #9047, #43656, #66831, #52606, #36557, #8141, #58360, #87200, #87656, #22348, #80110, #15249, #22807, #61605, #31779, #40252, #67769, #39317, #60210, #9990, #82433, #3838, #2445, #38863, #4295, #25595, #26063, #2896, #60673, #17583, #54952, #89988, #89511, #62064, #90898, #76737, #17109, #46432, #18983, #33174, #89049, #24676, #68234, #31323, #38406, #54478, #54018, #3356, #83347, #18495, #53561, #47359, #76274, #32246, #11400, #83829, #67315, #25142, #82885, #24198, #75335, #39785, #10451, #90438, #69168, #81952, #53075, #47835, #74880, #61153, #18041, #46893, #75794, #10917, #68708, #32720, #55903, #5257, #64452, #69633, #27015, #62552, #35051, #71051, #4761, #56379, #78618, #70590, #11864, #40714, #12834, #70120, #26549, #33642, #63030, #41672, #77683, #78158, #91861, #5717, #20851, #85245, #49263, #91394, #92809, #42610, #48304, #34592, #34126, #56864, #13296, #55437, #19439, #84289, #42134, #93278, #77204, #84756, #12334, #20392, #48777, #63500, #41180, #71527, #6184, #86164, #92330, #63968, #19904, #27974, #85706, #49722, #13762, #6661, #28430, #57323, #21316, #72904, #12, #58257, #51572, #14239, #59168, #22697, #8028, #50671, #72002, #86627, #80006, #478, #29825, #57780, #29366, #43553, #15606, #66281, #88497, #73834, #58707, #8948, #79557, #15145, #14698, #1394, #30751, #72449, #59653, #73383, #80935, #65368, #7121, #87100, #36925, #7568, #87550, #16080, #44933, #36453, #22250, #1860, #65839, #51120, #37827, #66733, #23644, #21797, #44006, #79087, #43097, #35990, #947, #80458, #64910, #28891, #30278, #44478, #8493, #88014, #23169, #37371, #52052, #39214, #31678, #2346, #4196, #74774, #67213, #53917, #38298, #81850, #9891, #82785, #82330, #17000, #18395, #47252, #17937, #46331, #69067, #52975, #45868, #61042, #31224, #53449, #38766, #46788, #89885, #74288, #24562, #32619, #25045, #67670, #75690, #88949, #33071, #60572, #10815, #68129, #25496, #2796, #60109, #11298, #39677, #81386, #61961, #3253, #24096, #68599, #16534, #89408, #17480, #61509, #90797, #75234, #3735, #32143, #90341, #52510, #76166, #10348, #45387, #54374, #83249, #9412, #40151, #78049, #11757, #18878, #5140, #56752, #70483, #76633, #83718, #5611, #19799, #85595, #41560, #13190, #47734, #34486, #20742, #40609, #34018, #49613, #71411, #48668, #12719, #69525, #85127, #42025, #49153, #19333, #27861, #55334, #26908, #4656, #91278, #69999, #20279, #33530, #26443, #78508, #70940, #13646, #84185, #42497, #62436, #41074, #48195, #6071, #34944, #77097, #63392, #92691, #84648, #64341, #25956, #55796, #12227, #62921, #54837, #91756, #77569, #92222, #27377, #56267, #63858, #6543, #35421, #62317, #75579, #12113, #55682, #61399, #83597, #83130, #69880, #26322, #53806, #32502, #46676, #91157, #12594, #63275, #4085, #90231, #55217, #61849, #90680, #17823, #84533, #84071, #5497, #47618, #19221, #82674, #18760, #5019, #54721, #76521, #19680, #40038, #48079, #76984, #11644, #39557, #32956, #40958, #10700, #33900, #62807, #40491, #25380, #68479, #54260, #25840, #68954, #69409, #3615, #4540, #18281, #91642, #26796, #34370, #48549, #77450, #41440, #47137, #70372, #11178, #24929, #43781, #27741, #72682, #86399, #245, #78394, #85004, #13535, #49960, #56637, #71775, #29128, #58024, #72230, #85487, #43333, #7344, #28211, #36225, #86878, #36688, #78851, #14001, #92108, #20634, #93511, #6424, #21553, #50437, #41913, #27262, #79340, #50901, #22032, #79785, #49504, #49038, #56149, #35772, #13077, #42383, #71296, #35299, #6898, #77934, #93055, #64225, #57554, #64685, #20158, #57099, #65144, #28668, #92571, #14475, #34832, #14927, #85939, #7801, #42861, #70826, #21090, #5958, #63743, #38064, #722, #75015, #16313, #73154, #66973, #29608, #66066, #66516, #74534, #10128, #37604, #9186, #81169, #59888, #46112, #31459, #1636, #17253, #16773, #1178, #82093, #60348, #23876, #51352, #58486, #44716, #2580, #45165, #22479, #87331, #74066, #59414, #89185, #2112, #52744, #80243, #31002, #24338, #15380, #73616, #53213, #65610, #88268, #52290, #44244, #88728, #81625, #45627, #58943, #67452, #30059, #30517, #8277, #37157, #15857, #9666, #87792, #22941, #51814, #38549, #80707, #8728, #23424, #83023, #55576, #90570, #10591, #62700, #91530, #77342, #17716, #18176, #19572, #4900, #60807, #32392, #39928, #31915, #38994, #26207, #54612, #68846, #55101, #47971, #89648, #75469, #25729, #47027, #82568, #84424, #61291, #53701, #40383, #24818, #68370, #90126, #69301, #3974, #3500, #33786, #26687, #4429, #32849, #48440, #39453, #67906, #76414, #3031, #61738, #33308, #46571, #83483, #83968, #18641, #47508, #25277, #54154, #62205, #11536, #91035, #75930, #11058, #19116, #76875, #12002, #40851, #69770, #77820 ),
 ( #92461, #64108, #41808, #85831, #43226, #72126, #86291, #5851, #57450, #21445, #42275, #50318, #7242, #50795, #92946, #28106, #12476, #70719, #13889, #20530, #35667, #64582, #56037, #41326, #93407, #65035, #36118, #136, #63637, #63167, #70261, #49849, #27150, #56524, #34722, #29018, #5395, #27625, #91997, #28559, #71659, #34260, #56993, #79224, #71187, #84891, #20041, #13428, #85381, #48921, #12969, #49399, #6315, #78290, #78747, #35183, #20982, #14366, #42743, #6792, #57905, #86760, #21921, #22369, #44603, #44130, #30882, #81058, #14822, #87222, #7693, #52176, #67337, #24220, #58834, #51243, #88145, #22830, #51699, #72572, #43676, #59775, #23302, #8617, #80132, #36579, #15271, #80587, #1070, #30405, #58378, #29950, #73035, #16203, #66855, #89071, #74412, #59297, #9542, #8164, #15743, #37047, #1990, #31345, #65959, #60233, #73953, #81509, #87679, #65493, #73507, #37494, #66403, #45054, #16656, #45510, #88617, #1519, #23764, #52630, #9068, #38428, #2468, #79679, #37946, #612, #29495, #17604, #54500, #61173, #76297, #11422, #2917, #53095, #40274, #11887, #19004, #40737, #10472, #10013, #91416, #90461, #67792, #3379, #46455, #76760, #17130, #68256, #38883, #69190, #18520, #45996, #3859, #26087, #18062, #81974, #74901, #54038, #75357, #31801, #60694, #39338, #82908, #25164, #25618, #32267, #46915, #62088, #32739, #83370, #89534, #4320, #83852, #24698, #75816, #90009, #33197, #47384, #53582, #82456, #10940, #90921, #69654, #39807, #68729, #61628, #54976, #47857, #4784, #33664, #62574, #65267, #8399, #50568, #22153, #56769, #86525, #72803, #57682, #79464, #22599, #43001, #58156, #373, #21690, #42513, #7025, #29260, #57226, #78982, #87001, #14598, #86067, #87453, #51474, #51021, #43455, #44376, #28336, #21217, #36353, #13661, #28795, #50087, #79908, #15046, #49628, #93638, #7927, #43906, #14135, #36819, #64358, #73287, #35896, #65741, #72353, #850, #71905, #71425, #80363, #29731, #85611, #37277, #7470, #35438, #58612, #20757, #64814, #15504, #66183, #27877, #78524, #6558, #93184, #89309, #75595, #60936, #31127, #46693, #46235, #30647, #17841, #89783, #53344, #80834, #87914, #74193, #32041, #45762, #51943, #59067, #74671, #88852, #24947, #16903, #82229, #23065, #9796, #53823, #15984, #9312, #82691, #10718, #24001, #81753, #44836, #60474, #17384, #24465, #88398, #3158, #59547, #2243, #73739, #66635, #45290, #75139, #8851, #1760, #39575, #10250, #1300, #23547, #52417, #38194, #30182, #52874, #81292, #37729, #16438, #67108, #60012, #38670, #67575, #2703, #31585, #39119, #68031, #61416, #13094, #55699, #84090, #4558, #84550, #77469, #90248, #11194, #55235, #47635, #18298, #20175, #90696, #83147, #69898, #54277, #32522, #33917, #19697, #91660, #61865, #70389, #4101, #69427, #25397, #40055, #18777, #62826, #47156, #68971, #34387, #48566, #56166, #32972, #25856, #76539, #85023, #26342, #54738, #92125, #27279, #68497, #76065, #11661, #49055, #63292, #83616, #40508, #33432, #62336, #3632, #12612, #19240, #91176, #41457, #5517, #48097, #77001, #12130, #40976, #5037, #77951, #26813, #56655, #43348, #27759, #71312, #93073, #72245, #71790, #6442, #7817, #36707, #7360, #35787, #58503, #42401, #35317, #50453, #85504, #42877, #64242, #36242, #79355, #63760, #14017, #22048, #14490, #28227, #65160, #78413, #87348, #49975, #263, #28685, #14943, #57115, #20651, #740, #29146, #70843, #51370, #86414, #49521, #58042, #5976, #85955, #6912, #50917, #80261, #64700, #86894, #57571, #79801, #22497, #65628, #93526, #41932, #43798, #21107, #34849, #29625, #72698, #13552, #92590, #78867, #21570, #59906, #66083, #73175, #88748, #9203, #46130, #31019, #67469, #37175, #23894, #75033, #8294, #23441, #10146, #60825, #38081, #2130, #52309, #81186, #1195, #39012, #52763, #89668, #66992, #9685, #44264, #74084, #60366, #45182, #81644, #67926, #30533, #45645, #16791, #74554, #30076, #88286, #38567, #58961, #89204, #2598, #31478, #80725, #87809, #22958, #16332, #59435, #24356, #51832, #53231, #73635, #82113, #17272, #24837, #3050, #31934, #53720, #15878, #15397, #44734, #8746, #37623, #66534, #1653, #76890, #84440, #68862, #75487, #3991, #40399, #18194, #62222, #19588, #48457, #62717, #75947, #33803, #91547, #18659, #26703, #77358, #27166, #69317, #4445, #82587, #47046, #83984, #90587, #12018, #40868, #32410, #17734, #69786, #41344, #12492, #70278, #39946, #39470, #46589, #26225, #3518, #32866, #11077, #5411, #10612, #61755, #68387, #4917, #47987, #61308, #33325, #55592, #47526, #90144, #25294, #83501, #25748, #54172, #83041, #54629, #76431, #11552, #55119, #91051, #19132, #34276, #63183, #92014, #12985, #43242, #86776, #92475, #20999, #20545, #7256, #57465, #84908, #63653, #77837, #28575, #43689, #625, #35199, #27641, #64598, #7708, #50333, #57919, #42292, #48937, #71204, #13905, #85397, #35683, #21937, #50809, #36132, #49415, #65049, #152, #85846, #29032, #79694, #56054, #42758, #71675, #20056, #78305, #86308, #64127, #79240, #14382, #5867, #41823, #72140, #14836, #72586, #36592, #13444, #70734, #34737, #93423, #56540, #6331, #92962, #65506, #28121, #57010, #49864, #78763, #21460, #6809, #73966, #2480, #88157, #67804, #29511, #30418, #87691, #44144, #58392, #80599, #59309, #1532, #2002, #15756, #23316, #38441, #9080, #66867, #80147, #16668, #60245, #65971, #52189, #22844, #74425, #30895, #87237, #37062, #51256, #59788, #17143, #22384, #8629, #1082, #37960, #66415, #81070, #15287, #89083, #88629, #10025, #16215, #23776, #73048, #45066, #9554, #52641, #81521, #24232, #44616, #45523, #67350, #31357, #8178, #37506, #53109, #29962, #81987, #46009, #74914, #58848, #51711, #73520, #38895, #18073, #47397, #75369, #46926, #61184, #33208, #83864, #12369, #91428, #76308, #26582, #68268, #3872, #3390, #19017, #48338, #32278, #75828, #53595, #26099, #62101, #60706, #11434, #69666, #61639, #41217, #2928, #32751, #90022, #17615, #31813, #54049, #90472, #68741, #69202, #82919, #25629, #11900, #40285, #4331, #82468, #47869, #33677, #39349, #54511, #25175, #76772, #90934, #89546, #10483, #24709, #54988, #84320, #46466, #10952, #39818, #40749, #83383, #18531, #4798, #62586, #55471, #77239, #19471, #64485, #5290, #35085, #21349, #6216, #28005, #64943, #85275, #6696, #42644, #64004, #84789, #49294, #71561, #34160, #50220, #13792, #92842, #41705, #63063, #77716, #71084, #20425, #20883, #48809, #78189, #34624, #35571, #57356, #79590, #44, #49755, #28924, #70622, #56898, #5749, #86197, #21827, #63534, #50702, #93312, #72036, #56416, #91892, #13327, #85737, #92361, #78652, #7151, #36026, #79124, #27523, #14271, #43131, #28462, #57812, #86663, #14731, #70154, #27046, #55934, #42169, #19939, #12866, #66765, #1896, #87131, #43584, #30787, #2376, #9446, #31254, #977, #514, #81881, #80968, #58288, #87585, #36955, #67246, #7597, #22282, #22730, #65869, #60141, #36484, #58742, #29396, #59685, #8982, #65401, #88049, #16567, #8525, #72482, #51154, #44509, #8065, #80039, #15180, #29858, #73415, #15640, #16113, #51604, #37404, #52542, #23205, #44964, #44038, #88528, #74322, #72940, #66314, #80492, #23676, #73864, #1429, #30313, #59202, #37861, #88980, #52085, #81417, #45422, #38332, #24128, #53006, #9923, #76660, #54404, #91311, #39707, #11327, #45902, #75720, #61990, #46818, #68631, #11787, #32174, #47281, #83277 ),
 ( #17510, #33100, #62469, #46362, #26473, #40178, #18907, #3281, #38796, #61075, #3764, #75263, #90369, #47762, #40637, #90825, #10378, #25985, #54870, #10843, #83751, #69556, #55362, #32649, #61537, #17036, #39245, #18421, #25073, #69097, #4224, #60603, #74807, #4685, #33559, #67700, #2828, #68161, #31711, #89438, #76198, #24596, #25525, #53485, #82361, #89917, #53946, #82814, #17965, #70032, #77128, #63424, #21236, #34976, #41102, #48226, #63890, #78079, #50105, #6105, #42531, #12258, #92725, #79000, #5175, #92253, #14154, #35913, #13222, #70972, #34049, #49646, #71442, #13680, #77602, #86085, #19830, #85162, #62952, #55825, #34517, #78541, #91786, #84681, #43019, #6579, #71922, #48697, #12752, #27410, #7043, #42058, #41593, #64831, #93655, #28815, #26937, #56298, #84214, #19362, #70515, #5642, #20315, #49185, #27897, #35457, #56786, #85628, #64375, #93201, #20774, #28353, #57243, #36841, #7488, #10625, #79926, #72371, #59089, #43474, #87019, #15063, #87931, #87470, #22171, #23566, #53735, #23082, #51492, #75503, #58177, #51039, #66201, #36373, #58629, #43925, #51962, #1317, #79482, #29748, #37746, #30199, #72821, #80854, #391, #39483, #65759, #16001, #44396, #30664, #7946, #65286, #17748, #44853, #86542, #68405, #8416, #29280, #73756, #21712, #869, #22617, #66654, #3533, #80380, #8868, #73305, #1780, #57699, #46601, #50588, #15521, #37295, #59566, #88416, #82601, #14617, #92029, #69801, #13003, #55135, #26719, #61322, #91072, #77373, #62237, #83999, #27184, #47541, #62732, #4937, #26242, #47060, #11566, #33822, #90160, #12511, #91562, #19147, #4006, #25308, #39960, #33340, #76445, #76906, #11094, #40414, #90602, #55606, #19605, #41839, #56071, #12036, #84924, #32881, #48002, #61769, #48473, #77853, #25763, #70750, #84455, #34291, #18675, #54186, #69332, #40883, #54645, #41361, #63199, #20076, #70295, #83519, #5426, #48955, #32423, #83056, #18210, #75965, #68876, #4463, #5884, #6346, #21474, #21014, #14397, #43256, #20560, #34754, #7270, #14851, #50825, #43704, #92978, #85412, #63669, #50352, #78320, #49881, #28136, #72603, #27661, #85863, #49432, #36147, #72154, #56558, #57481, #86793, #6823, #92492, #13459, #86322, #42778, #57025, #42310, #35697, #79256, #65068, #29046, #64611, #167, #71219, #57939, #21952, #78779, #7725, #35219, #71694, #79709, #93437, #64145, #13920, #28591, #4296, #18496, #63031, #6185, #62553, #34127, #12335, #84757, #71053, #56380, #26550, #42135, #41673, #26064, #13297, #85246, #48778, #76275, #83348, #69634, #27486, #41181, #47360, #54479, #70121, #84290, #20393, #5258, #77684, #11401, #91862, #49264, #40253, #4762, #78159, #35052, #19440, #77205, #69169, #55905, #12835, #19905, #83830, #92331, #54953, #91395, #33176, #62065, #40716, #70591, #90899, #18984, #90439, #5718, #25596, #47836, #76738, #33643, #11865, #48306, #55438, #27016, #34593, #63502, #42611, #14240, #44480, #29827, #85707, #57324, #64911, #56865, #8495, #51123, #79558, #14, #80008, #72906, #20852, #6662, #50672, #43098, #13763, #15608, #86166, #78620, #65369, #49723, #93279, #21317, #479, #28892, #28431, #58710, #87552, #29367, #57781, #80460, #64453, #50188, #72450, #71528, #86628, #79088, #58259, #7569, #35538, #35992, #44008, #36454, #72003, #87102, #7122, #73385, #21798, #22252, #14699, #36927, #43554, #15148, #22700, #8030, #92810, #63969, #65841, #949, #51574, #27975, #37830, #38300, #46333, #23646, #88951, #66735, #17002, #68132, #3255, #17482, #30753, #82332, #75236, #67215, #10350, #32145, #75692, #24098, #52978, #37373, #1862, #38768, #45390, #60575, #89410, #80937, #66283, #24564, #89887, #61044, #25047, #88499, #88016, #1396, #74776, #52054, #81388, #59655, #53919, #30281, #52512, #23171, #53451, #2798, #59170, #81852, #39216, #2348, #16082, #44935, #31226, #16536, #73836, #8950, #74290, #60111, #9414, #9893, #45870, #67672, #82787, #31680, #17939, #46790, #91757, #41561, #47253, #69526, #69068, #55797, #12229, #39678, #18396, #32620, #77098, #92223, #49154, #83719, #76167, #19334, #47735, #76634, #3736, #70484, #48196, #85128, #33531, #5141, #68600, #4658, #84649, #40610, #62437, #5612, #25957, #41075, #70000, #91279, #25497, #18879, #34019, #61510, #19801, #62922, #26444, #11299, #90342, #40152, #11758, #54838, #55335, #83251, #84186, #4197, #26909, #48669, #20280, #34487, #77570, #63393, #33072, #12720, #61962, #27379, #56268, #90798, #10816, #54375, #79893, #64342, #70941, #22585, #65252, #93622, #14118, #357, #86985, #6072, #20743, #64798, #57210, #27862, #29716, #6544, #92692, #79447, #63859, #13647, #35422, #14583, #42982, #42499, #43891, #72788, #43440, #71887, #834, #78509, #71412, #86511, #56753, #78967, #93169, #72336, #21674, #34946, #50072, #58139, #50550, #28321, #7455, #49614, #58598, #86051, #36337, #28780, #51006, #21200, #85596, #36802, #29244, #13191, #87439, #57665, #7009, #22138, #42026, #35881, #15032, #7912, #78050, #65723, #88835, #67092, #45743, #32023, #17367, #81276, #3141, #2687, #80818, #68012, #46218, #9779, #37263, #44361, #30631, #82213, #2225, #8383, #15490, #31109, #45274, #75122, #59996, #38654, #73271, #23985, #10232, #66169, #59531, #39100, #60920, #74177, #38177, #1285, #16886, #67558, #74655, #44821, #53327, #15967, #52399, #30167, #23050, #1743, #31568, #59050, #51928, #89767, #60458, #51460, #73724, #8836, #88380, #80349, #9295, #37714, #87898, #66620, #23530, #16422, #52858, #81736, #89293, #24448, #16470, #24033, #16018, #82723, #10284, #10753, #81323, #52449, #67144, #39610, #74708, #88433, #46727, #75630, #61451, #1797, #2278, #3672, #17875, #44869, #45325, #52909, #8885, #23099, #39154, #38702, #81787, #68066, #32075, #37764, #59582, #9829, #31161, #66669, #68534, #74227, #30682, #53380, #23582, #9346, #60047, #82265, #16936, #88885, #32559, #51981, #17418, #45798, #80870, #67609, #2737, #31617, #60508, #89343, #46267, #75171, #3191, #60974, #89823, #24984, #53857, #90733, #62860, #33008, #13129, #4594, #19735, #77035, #63328, #76573, #40090, #49090, #91693, #25433, #6009, #41009, #4137, #26845, #54311, #25892, #91213, #5551, #34884, #62370, #33956, #12166, #84585, #70878, #56202, #26381, #41965, #41495, #54774, #90282, #85061, #48603, #76102, #83186, #69462, #27316, #69932, #47189, #18333, #5074, #84124, #20212, #55733, #77503, #11235, #12650, #77988, #69006, #33467, #61899, #83651, #19274, #70425, #18815, #34421, #92159, #47672, #11696, #40547, #55269, #48132, #85535, #35355, #14050, #29178, #27795, #64277, #80292, #93106, #28261, #72274, #49553, #64733, #57149, #58074, #7393, #20682, #35819, #43829, #36274, #85990, #65195, #6477, #15431, #71827, #86927, #50485, #36738, #50010, #13584, #22529, #298, #92624, #73206, #14524, #71346, #22080, #56688, #21140, #93560, #72730, #8325, #28718, #50950, #79387, #79833, #44298, #29657, #57603, #63795, #14973, #78903, #78448, #58537, #7851, #42436, #42913, #6946, #773, #43379, #86446, #21604, #65659, #87382, #51401, #52797, #89236, #58992, #16825, #67957, #1228, #45214, #3082, #82618, #31050, #23927, #30110, #2631, #24389, #60398, #30566, #39046, #66563, #38115, #87841, #8777, #81217, #31510, #22991, #37655, #31967, #53267, #24870, #1685, #59464, #16363, #53752, #88779, #88316, #60860, #89703, #75520, #15910, #74116, #17765, #46619, #51865, #23473 ),
 ( #52339, #67500, #17305, #37207, #66115, #81676, #45682, #80758, #9236, #38597, #67025, #82150, #46162, #44766, #73666, #75065, #2161, #59940, #74589, #9717, #10176, #48977, #48022, #25326, #54664, #4027, #34312, #68423, #25782, #61343, #33842, #69822, #3553, #55155, #77393, #69351, #10642, #39502, #11586, #68895, #54206, #32442, #61788, #40433, #76464, #76927, #90620, #4481, #19625, #84017, #12055, #90178, #91583, #41380, #47079, #33358, #32900, #55626, #40902, #83074, #18228, #75985, #4956, #92050, #11113, #83537, #39980, #19165, #47559, #62256, #18696, #70314, #62751, #84945, #91090, #26740, #26261, #84475, #48493, #12530, #5445, #63218, #27204, #56091, #20095, #71715, #92514, #57044, #50373, #13022, #57961, #21495, #6842, #49451, #70771, #85431, #78797, #92997, #28611, #56578, #28155, #42328, #14418, #65088, #87274, #72623, #57500, #7745, #78339, #13942, #13481, #188, #29548, #71239, #58428, #72173, #79729, #64165, #5904, #85882, #35716, #6368, #86344, #14871, #43725, #86815, #35239, #29069, #21973, #42799, #79277, #36628, #41858, #21034, #65550, #22420, #64630, #93456, #34774, #43275, #50846, #7289, #49902, #664, #36167, #77873, #63689, #27680, #20579, #16706, #15322, #51749, #17185, #38483, #38933, #15796, #80641, #1571, #67842, #9120, #22882, #74953, #10063, #89583, #29999, #30454, #31853, #46048, #73089, #44655, #52225, #44183, #51292, #67387, #66906, #81108, #2517, #60284, #8219, #87730, #37997, #59348, #1118, #2968, #73556, #66006, #52677, #37097, #8665, #37543, #81558, #16251, #66454, #60742, #80184, #45561, #45101, #58884, #88199, #23358, #59824, #74003, #2045, #30934, #74463, #88665, #23814, #9596, #31394, #89121, #24272, #53147, #82027, #41253, #32786, #47907, #11471, #91466, #10988, #68306, #77276, #90970, #53636, #34195, #69237, #32324, #26136, #82506, #25213, #25667, #33715, #63099, #90506, #62139, #40322, #19051, #5327, #84357, #54548, #70194, #69702, #54086, #24754, #19506, #76810, #10524, #17654, #3909, #55508, #4366, #75408, #46505, #33244, #18570, #48374, #55031, #11935, #39391, #83900, #3428, #61226, #40784, #90060, #4831, #82956, #18111, #83416, #62627, #46963, #47436, #26617, #12405, #75865, #39858, #68780, #76345, #61674, #43162, #27555, #14759, #57840, #50248, #77751, #84822, #71116, #28954, #42674, #48846, #55969, #71591, #85766, #86694, #13822, #79154, #19971, #6728, #21859, #12902, #6246, #50733, #43613, #20916, #78682, #41740, #57385, #14302, #21378, #85312, #76, #56450, #92877, #70653, #63569, #42202, #86228, #5781, #92395, #79617, #72063, #72509, #20460, #49328, #35115, #7629, #49785, #78222, #36514, #91927, #27082, #34655, #64035, #13361, #28039, #56928, #35600, #64515, #93341, #28492, #7180, #36055, #64973, #52569, #74353, #58316, #8097, #52115, #44541, #15210, #17065, #87614, #80067, #66794, #51180, #1008, #22765, #1924, #1457, #29888, #31286, #60172, #30818, #59233, #81913, #65896, #58772, #73893, #44067, #66343, #51635, #59715, #9010, #87160, #37434, #45453, #37889, #80521, #88558, #36984, #45932, #73444, #23706, #80998, #38362, #15674, #72968, #24157, #81449, #8554, #30343, #88079, #89010, #29426, #23235, #22309, #16597, #9476, #16140, #44992, #67276, #2406, #9953, #65429, #53037, #74840, #543, #67732, #89951, #68665, #10878, #11362, #25106, #3801, #47795, #83311, #76231, #89471, #26024, #69592, #75295, #32682, #3316, #83786, #40214, #2859, #46395, #60634, #69130, #26509, #77166, #18001, #10414, #47315, #75757, #39741, #31741, #4722, #4258, #19401, #61568, #33136, #24632, #90401, #18941, #25558, #54438, #33600, #53980, #62026, #90860, #18456, #53519, #46854, #54907, #82395, #76697, #11823, #40674, #39278, #17543, #68196, #62508, #82849, #91348, #32205, #55398, #61112, #84250, #48264, #38825, #7077, #85663, #35950, #77641, #13256, #12792, #28389, #57737, #41633, #86582, #6614, #14194, #92288, #5216, #27445, #63926, #70552, #20811, #43055, #71959, #86123, #5675, #57281, #21272, #42093, #50144, #64869, #50628, #92764, #27931, #12296, #34550, #13714, #20349, #35494, #64409, #55866, #41141, #93236, #93695, #28851, #21752, #63458, #62991, #70074, #34089, #56822, #79042, #91822, #49681, #26975, #84718, #49221, #19867, #48737, #6139, #78576, #56337, #71482, #85199, #78118, #71008, #35011, #42566, #81688, #7526, #52352, #31062, #46171, #43512, #81228, #46631, #67967, #68433, #45225, #16374, #59949, #3564, #38610, #74129, #10656, #39512, #25337, #59478, #88789, #61355, #75531, #36411, #9248, #16837, #72410, #79518, #3093, #2643, #45693, #31977, #89715, #65326, #23485, #67513, #23937, #29319, #32455, #38126, #431, #82161, #88332, #67038, #2176, #17319, #74602, #52809, #90189, #14656, #75075, #9732, #31521, #60409, #89248, #24400, #53278, #10186, #39055, #60870, #24881, #53762, #82628, #17777, #62765, #54677, #26754, #90634, #70784, #62271, #77407, #40915, #27219, #40446, #4041, #13036, #55638, #83086, #63704, #4970, #61802, #84492, #18240, #83550, #55169, #63233, #92529, #26274, #91598, #69836, #48506, #34789, #20111, #84031, #5919, #5458, #18709, #54217, #48991, #12544, #39992, #47092, #33372, #84960, #33855, #11127, #75997, #19638, #48036, #76940, #77892, #41394, #70328, #68910, #34326, #41873, #32912, #91106, #25796, #47573, #12068, #92064, #76478, #56105, #11600, #69363, #4494, #19176, #57061, #28626, #49465, #93013, #71730, #86832, #85446, #28171, #87291, #14887, #15341, #85897, #21050, #6857, #44202, #79294, #49917, #51310, #80202, #66024, #6384, #35732, #8236, #22437, #78354, #78813, #57516, #20595, #27695, #43741, #43292, #86360, #72641, #36647, #13495, #64180, #14435, #64645, #71255, #73109, #13959, #42344, #29087, #35255, #42816, #93473, #57979, #21512, #50390, #37115, #56592, #21990, #72189, #7305, #36185, #65104, #205, #50863, #79745, #7761, #65567, #681, #29565, #58446, #74972, #9617, #1590, #67408, #37562, #17673, #9139, #24292, #81579, #67863, #81126, #44673, #53656, #2537, #30017, #10546, #45580, #8684, #31416, #58901, #30472, #2064, #10084, #39411, #66926, #38504, #16727, #89142, #75427, #60762, #30955, #46526, #46066, #59368, #1136, #89603, #53168, #80660, #87747, #74022, #31873, #74485, #51770, #22899, #60304, #82048, #88220, #17205, #66473, #15816, #38016, #38952, #2987, #24773, #16270, #73575, #82525, #23376, #52245, #45120, #59843, #88684, #23832, #52697, #68800, #69257, #77295, #77772, #40340, #11955, #83920, #62649, #48869, #34213, #4385, #19990, #19525, #3929, #84842, #63119, #26638, #54106, #61245, #47458, #5347, #19072, #25232, #32346, #47926, #62160, #91948, #76829, #55528, #90080, #40804, #27102, #82978, #76365, #55987, #12920, #90989, #55051, #18129, #33736, #84377, #91485, #61693, #70213, #32803, #33263, #46983, #39879, #18592, #48392, #75883, #90524, #68327, #12425, #3451, #25686, #54567, #11491, #11009, #26159, #83437, #69721, #4852, #41276, #20480, #85784, #22327, #7647, #63589, #35133, #42693, #34674, #80085, #28973, #57403, #71612, #57858, #50751, #92413, #78242, #28510, #20935, #85330, #87178, #64056, #56471, #43180, #27573, #71136, #92898, #72082, #6746, #6265, #36532, #65447, #7198, #35619, #58336, #42221, #28057, #50266, #49347, #64534, #56947, #36073, #79175, #13379, #13842, #21879, #49803, #93359, #78700, #64990, #14320, #86244, #21395, #79635, #94, #86714, #14777, #43630 ),
 ( #563, #29448, #51198, #72527, #41761, #70672, #5801, #29906, #59250, #8573, #38842, #72987, #30361, #65916, #38382, #74370, #8117, #59733, #81930, #73911, #53539, #15228, #16158, #73461, #58790, #44084, #66360, #45010, #81014, #81467, #1475, #9027, #24175, #88575, #52586, #1028, #2423, #45952, #51653, #37906, #37451, #60189, #16615, #37003, #22784, #87634, #45470, #2875, #80539, #88096, #15696, #23723, #52134, #66811, #44558, #74858, #9494, #89489, #1941, #67294, #23256, #30838, #89027, #31303, #53055, #9970, #17083, #67749, #31759, #60652, #24650, #61585, #54924, #17560, #62525, #26040, #11380, #53997, #75313, #89969, #83327, #3818, #33152, #61132, #32699, #46871, #18959, #69608, #91838, #77182, #4738, #26992, #12312, #62042, #41156, #82866, #18473, #18019, #33618, #34105, #75775, #63007, #76713, #84267, #68686, #10431, #90417, #40231, #10895, #90877, #19417, #48280, #91367, #39760, #26526, #55415, #47333, #70091, #5233, #82413, #69146, #4274, #46412, #25574, #83805, #54455, #11839, #40690, #32223, #39295, #68214, #3334, #25123, #76251, #47812, #12810, #450, #93252, #70567, #6156, #49239, #79533, #19882, #71025, #41650, #79059, #21288, #48753, #6631, #28865, #20827, #55881, #84733, #56839, #20368, #5692, #77658, #13272, #85680, #27949, #28406, #42109, #49696, #64885, #35511, #57297, #34567, #43071, #86599, #92304, #78592, #78134, #7094, #86139, #63475, #27461, #56353, #50162, #43528, #85215, #35028, #63942, #64426, #92780, #13733, #42584, #21768, #14210, #36426, #71499, #71975, #35965, #93710, #57753, #50644, #14672, #72425, #7542, #65343, #1833, #23137, #43978, #8466, #30719, #58229, #9384, #66704, #52019, #920, #22222, #36893, #30250, #44448, #73806, #8001, #73354, #87525, #59619, #59141, #22671, #72877, #87073, #80433, #87984, #1368, #88468, #15578, #80905, #38267, #8920, #23615, #79980, #16506, #60081, #65809, #16051, #51543, #74261, #52482, #51091, #29799, #15117, #81356, #16971, #67641, #37346, #58680, #37798, #66252, #44903, #45358, #88918, #67179, #9861, #2314, #31196, #24068, #52944, #81821, #45836, #74741, #38736, #29334, #33040, #69038, #90312, #17450, #75660, #4167, #31649, #76604, #40121, #25464, #68098, #89377, #10318, #3705, #17907, #47224, #75204, #46760, #61010, #61929, #83686, #12197, #91248, #76134, #26412, #3223, #32591, #32113, #18847, #48164, #89856, #77066, #90767, #4625, #82754, #24533, #10784, #54345, #25016, #11268, #33499, #62406, #11728, #53888, #47705, #40580, #61481, #69495, #55302, #41039, #83219, #18364, #2767, #39645, #25925, #68569, #54808, #84155, #46299, #60539, #19303, #53416, #82299, #39186, #27346, #26877, #14551, #13613, #84618, #20243, #63359, #93589, #33986, #85095, #55764, #93132, #35388, #62889, #20711, #42948, #34912, #69968, #5108, #28288, #56717, #71854, #56232, #19766, #28748, #42466, #91725, #79417, #49581, #77536, #71376, #48635, #70453, #70906, #78932, #12687, #41993, #6510, #85564, #64308, #50518, #35847, #6040, #21640, #21168, #5580, #86474, #64765, #57178, #41527, #34451, #49121, #6975, #78476, #92190, #78017, #86018, #63824, #57631, #50037, #14083, #13157, #92657, #27829, #7423, #51428, #74145, #88802, #37234, #30136, #36304, #8802, #30593, #66589, #36769, #45239, #72757, #44329, #65220, #15000, #87407, #37682, #325, #43860, #9262, #59497, #31075, #7878, #65689, #22554, #59963, #1255, #803, #67055, #2191, #81701, #22108, #80318, #23949, #38139, #29210, #29683, #73240, #58109, #43408, #88348, #59020, #8351, #23499, #52367, #86955, #79862, #87867, #15457, #50977, #52821, #58567, #66139, #44791, #23017, #51895, #80788, #73692, #15937, #1710, #72302, #81242, #16389, #10669, #33385, #17333, #46183, #25348, #2654, #17790, #75089, #76011, #54229, #38621, #82640, #90647, #83097, #10198, #18251, #53291, #62284, #24894, #55185, #47104, #31533, #60881, #39067, #40458, #74618, #31989, #67524, #40006, #11144, #9746, #61367, #83563, #75544, #16850, #45705, #46643, #67980, #60420, #89260, #3106, #39524, #68445, #68923, #89732, #3580, #25809, #90200, #4054, #24411, #32924, #47586, #82177, #32469, #53774, #61814, #54689, #18725, #76490, #11613, #69376, #4506, #91120, #26291, #35153, #14337, #71629, #6761, #78259, #43646, #43196, #29462, #28528, #65007, #20497, #93377, #86730, #64553, #57421, #7663, #78716, #7214, #72097, #86261, #42240, #42712, #36087, #49365, #21893, #108, #21412, #92913, #13396, #64074, #35635, #13857, #50287, #6282, #79194, #85800, #28987, #57875, #58351, #36546, #50766, #72542, #28075, #79650, #56963, #14791, #87191, #20951, #85349, #65462, #579, #71153, #49819, #62485, #34066, #10501, #55844, #13237, #42073, #56316, #68286, #27426, #85181, #12275, #20330, #70989, #20791, #62968, #91802, #74933, #39370, #77619, #84229, #5656, #34531, #24733, #10043, #63439, #34991, #6121, #63908, #33576, #31833, #48243, #19845, #26954, #70532, #56801, #92743, #41119, #27914, #49200, #4699, #85643, #38913, #92269, #60724, #67822, #55377, #2947, #84698, #89563, #53616, #48716, #70051, #82486, #12768, #78096, #17634, #41610, #46485, #75388, #19378, #91325, #26487, #5193, #77145, #13695, #15080, #36858, #72837, #43036, #51507, #79020, #50607, #71462, #21252, #93674, #43940, #42547, #50122, #15540, #65774, #37310, #14173, #71938, #28832, #66217, #7505, #7059, #73320, #8431, #87947, #28368, #57716, #30214, #44412, #6595, #35929, #79498, #35473, #49662, #883, #65303, #14634, #29764, #58643, #64390, #86103, #36390, #86562, #93216, #1332, #64847, #57260, #51054, #21731, #43492, #72388, #79942, #410, #29297, #59105, #78557, #7964, #58192, #87035, #22186, #87485, #22635, #80395, #44482, #80462, #37375, #8497, #22702, #73387, #30284, #66285, #15610, #1398, #59172, #51576, #26177, #41294, #4871, #84859, #4402, #61709, #70688, #84394, #46999, #27594, #62666, #25701, #19542, #75902, #18610, #19089, #27121, #56491, #11027, #91965, #55544, #40820, #83455, #39895, #54583, #47943, #33281, #91499, #90543, #62176, #76381, #48408, #5364, #18145, #12939, #26655, #41778, #47474, #76845, #11509, #34230, #63606, #40356, #92430, #12446, #20011, #91008, #68816, #55067, #69739, #69273, #77311, #48889, #77790, #56004, #83936, #63136, #5818, #11972, #34692, #3947, #32819, #33754, #70229, #85350, #49820, #86731, #93378, #14792, #43647, #35154, #20498, #72543, #44098, #51211, #73004, #42713, #42241, #29920, #28988, #6283, #35636, #78717, #15241, #49366, #6762, #71154, #7664, #50767, #78260, #36088, #58352, #50288, #13397, #64075, #86262, #13858, #92914, #28076, #71630, #21413, #57422, #57876, #64554, #79195, #580, #65008, #21894, #56964, #36547, #22340, #85801, #14338, #28529, #65463, #79651, #20952, #43197, #72098, #29463, #8132, #7215, #109, #87192, #80102, #37015, #65929, #1041, #24665, #2435, #39307, #81478, #53066, #87648, #23734, #9981, #88586, #16627, #53552, #73922, #89038, #31314, #52597, #73474, #37917, #60200, #37464, #9039, #23270, #24188, #45965, #68224, #82424, #38397, #17574, #30374, #59745, #59265, #74871, #10441, #88113, #3344, #81941, #60663, #45022, #51666, #66821, #45481, #52146, #67306, #89500, #46423, #38853, #81026, #67760, #2886, #74380, #31771, #75325, #58804, #9508, #17098, #22799, #16170, #80556, #1959, #15710, #44571, #8586, #66373, #1490, #30852, #91850, #19893, #83337, #82876, #70579, #69622 ),
 ( #41167, #76726, #4750, #18029, #19429, #63018, #68698, #90889, #90428, #77194, #33630, #61144, #39773, #54009, #62540, #48764, #32235, #11390, #3828, #40702, #69158, #4285, #25133, #27004, #91382, #12823, #54939, #26538, #89979, #26052, #12323, #62054, #83819, #55892, #47346, #55425, #84278, #18971, #46883, #40242, #48292, #75785, #70106, #5246, #47824, #32710, #10905, #61595, #33163, #76263, #11853, #84746, #25584, #34116, #77670, #41662, #54467, #18483, #63489, #64900, #86615, #28881, #92796, #7557, #35042, #6648, #27475, #71039, #49711, #1, #92320, #6173, #65357, #21785, #87088, #63956, #27964, #78606, #22237, #57312, #56853, #29353, #58245, #43994, #78147, #13751, #79994, #464, #56367, #85694, #35528, #85231, #5704, #50661, #21305, #64441, #79547, #14687, #20382, #42122, #86154, #42599, #49252, #51108, #20840, #13285, #7109, #71514, #93267, #28421, #35980, #50178, #79074, #15131, #34580, #57769, #14226, #43087, #71991, #43542, #72439, #36442, #73822, #8481, #38283, #81373, #934, #44920, #52960, #16522, #73369, #45373, #15591, #89394, #80923, #2332, #59637, #45852, #59156, #22685, #31664, #74276, #8015, #82316, #23631, #80446, #9399, #36909, #37360, #8935, #81837, #17466, #37813, #67196, #88484, #31211, #53432, #38753, #66720, #24548, #24084, #66267, #72891, #67657, #60096, #58694, #65827, #52037, #9877, #52496, #29813, #87538, #88935, #1848, #2783, #16987, #74758, #51558, #60556, #44464, #30735, #1382, #30264, #88000, #23153, #16066, #90782, #25032, #61495, #10800, #76620, #33516, #55780, #41058, #25942, #69984, #17923, #47238, #46774, #62422, #91741, #75675, #84633, #40596, #48180, #32606, #39201, #90327, #4182, #39662, #54823, #77081, #12212, #26427, #68584, #91263, #55320, #76150, #84170, #5124, #46316, #33056, #61945, #75220, #3720, #47720, #54360, #69510, #4641, #89871, #10334, #19318, #34001, #62905, #68113, #25481, #3239, #32129, #83701, #61025, #83234, #18381, #53903, #82771, #11283, #40137, #69053, #11743, #18863, #64323, #86494, #78492, #58123, #19782, #20726, #78033, #34469, #48653, #70924, #49596, #85579, #86034, #6055, #13630, #28763, #93149, #57193, #70467, #6991, #50533, #56250, #42481, #13173, #64780, #21183, #77554, #27361, #41543, #50054, #7439, #12703, #92674, #85110, #28303, #56733, #71394, #5595, #79431, #78950, #341, #6527, #14100, #63375, #35403, #93605, #42964, #71869, #14567, #34927, #35863, #57646, #21657, #92205, #27844, #43423, #20260, #72318, #36321, #49136, #65235, #42008, #63842, #29228, #2206, #2668, #59032, #30610, #8815, #81257, #67539, #52839, #23031, #38636, #38157, #22568, #9761, #81716, #45254, #72771, #79875, #66151, #23965, #37695, #43874, #50990, #66601, #80801, #16865, #1723, #74158, #15015, #59512, #45724, #7896, #1267, #74634, #31547, #15949, #73705, #36785, #52380, #9274, #16402, #80330, #88817, #51442, #87879, #65705, #58581, #37247, #67072, #817, #87420, #86968, #31090, #22122, #15473, #44344, #30149, #29698, #44804, #73254, #8366, #51910, #88361, #23511, #59978, #40943, #55201, #82193, #53786, #61381, #53308, #5001, #47601, #76031, #90214, #76504, #69390, #17347, #3123, #47118, #39540, #10213, #12096, #82654, #75103, #61830, #46198, #89749, #17803, #90663, #25363, #24909, #84056, #19204, #25823, #54243, #76967, #60901, #46656, #68937, #39081, #83113, #75560, #54703, #4068, #67995, #32484, #40473, #32938, #10682, #83580, #32003, #69863, #68462, #18743, #11160, #33399, #3597, #18264, #48063, #11627, #89275, #60439, #4523, #24426, #40021, #62298, #91139, #22810, #93388, #63260, #79205, #51679, #86742, #5483, #58816, #87660, #73486, #12578, #14348, #15722, #1052, #55667, #28541, #36099, #26780, #33884, #22351, #50777, #65019, #51224, #44112, #84518, #70357, #21904, #43207, #77434, #80568, #57432, #48533, #36560, #19665, #86273, #21425, #65475, #119, #50299, #29931, #44583, #593, #29000, #62792, #34355, #72109, #43659, #41425, #57886, #7225, #29475, #72554, #79663, #14804, #15252, #7676, #58363, #87203, #80113, #91627, #73015, #8144, #37027, #65941, #88597, #52156, #61156, #74883, #37475, #18044, #53078, #16182, #9993, #66385, #9050, #9522, #17586, #46896, #74393, #45977, #24201, #2899, #82888, #68238, #38409, #54021, #53564, #37928, #25146, #3360, #60676, #88124, #1501, #81491, #39320, #81955, #59278, #30386, #17112, #2448, #32249, #38866, #89515, #23282, #67772, #89991, #81038, #16638, #8598, #45034, #31326, #89052, #73935, #31782, #24679, #82437, #1971, #10454, #66835, #67318, #30863, #59757, #52609, #23746, #46435, #45492, #60213, #75338, #10921, #40720, #27019, #11868, #33647, #70594, #90902, #12338, #48309, #69637, #90442, #54956, #77209, #39788, #55908, #19443, #4765, #47363, #68711, #83351, #76741, #26068, #26553, #54482, #83833, #40256, #41185, #63034, #85249, #5721, #55441, #34596, #76278, #62556, #11404, #91865, #27489, #69172, #56385, #70124, #77687, #62068, #3841, #18987, #91398, #4300, #84293, #12838, #41676, #84760, #33179, #19909, #48781, #5261, #63506, #92334, #20396, #34130, #75797, #32723, #47839, #61609, #25599, #18500, #7571, #92814, #49267, #36456, #8033, #15150, #36929, #6665, #6188, #87555, #86632, #63974, #93282, #42614, #72908, #13300, #64456, #35055, #72452, #14702, #42138, #17, #22254, #14243, #78162, #71056, #50191, #13766, #27978, #56868, #35542, #79093, #21320, #21800, #28434, #43101, #58261, #28895, #50674, #85710, #65371, #80010, #20855, #72007, #71532, #482, #79560, #49726, #78623, #57327, #43556, #65843, #86169, #7125, #35995, #57784, #64914, #29369, #87104, #51126, #44010, #951, #29829, #58712, #68261, #48329, #39811, #54980, #18524, #4788, #18066, #75361, #84312, #4324, #60699, #41208, #76300, #39342, #33201, #89538, #32271, #32743, #40741, #70146, #3864, #69194, #47390, #26091, #12360, #91420, #61632, #77231, #76764, #61177, #31806, #26573, #83856, #17608, #24702, #10945, #62578, #11426, #82460, #53586, #40278, #25622, #55462, #62092, #19008, #46459, #90925, #19463, #10476, #68733, #3383, #90013, #54504, #47861, #25168, #11891, #69658, #33668, #54042, #82912, #46919, #90465, #75821, #83375, #49285, #64476, #63056, #5741, #64935, #86189, #86654, #63526, #34615, #78181, #21819, #56889, #70614, #28916, #57804, #43576, #77709, #13319, #79579, #36, #27039, #92353, #6208, #91885, #5282, #21341, #20875, #35076, #50211, #14263, #55928, #41696, #85729, #42159, #48799, #50694, #27511, #19931, #6686, #84780, #56407, #85268, #35563, #63993, #20417, #14723, #34151, #93304, #92834, #12858, #71076, #27997, #13784, #49747, #78644, #42635, #28454, #71551, #57349, #79115, #43121, #72027, #7143, #36017, #37851, #36476, #72929, #38325, #59677, #60134, #36948, #8056, #22721, #88973, #30305, #44029, #2369, #31247, #17025, #51146, #51596, #53000, #67239, #505, #65861, #73407, #65392, #72474, #88520, #88039, #8517, #23668, #81409, #29387, #15171, #59193, #80482, #22272, #24121, #969, #87122, #73856, #58280, #29849, #58732, #8973, #37396, #87577, #81874, #7590, #66757, #66305, #80030, #15632, #44501, #80960, #1419, #23196, #52077, #1885, #16104, #44956, #30778, #52534, #16559, #45413, #74312, #9438, #62458, #53938, #69087, #32639, #18898, #32166, #89431, #4676, #18413, #74799, #55353, #90360, #53475, #47273, #9916, #46355, #46811, #54859, #84205, #17958, #83269, #61529 ),
 ( #38789, #82807, #76651, #91301, #39698, #25517, #67693, #11319, #33090, #4215, #39238, #47753, #75713, #10836, #76189, #3274, #68623, #83741, #54396, #40170, #2821, #61981, #11776, #82354, #3757, #10371, #90816, #25975, #31703, #17502, #60596, #40628, #33550, #45894, #25066, #75256, #69546, #26464, #24587, #68154, #61067, #89908, #93646, #42048, #13671, #48214, #78069, #64366, #49175, #70962, #14145, #34507, #49637, #85619, #13212, #34039, #92243, #20765, #77118, #93192, #56777, #6095, #84669, #12247, #26927, #20304, #63414, #63879, #91776, #27398, #77590, #78532, #6568, #28806, #43009, #92717, #71913, #19820, #34967, #48686, #35447, #64822, #12741, #57690, #42521, #21227, #5632, #41093, #56288, #27887, #41583, #71433, #50096, #78990, #28344, #70505, #57234, #86076, #7034, #35904, #19352, #70021, #5164, #62942, #55815, #85151, #87923, #859, #15993, #44845, #36364, #86533, #73748, #45299, #52426, #74204, #43917, #43465, #31136, #30191, #7479, #36831, #79918, #16447, #50578, #7937, #72362, #8860, #51953, #79473, #37286, #59557, #51484, #21701, #14607, #87462, #51030, #65277, #382, #72812, #65750, #23074, #59080, #80372, #29270, #29740, #80844, #58166, #66646, #37738, #15513, #87010, #22162, #15055, #22609, #58621, #66193, #44386, #73296, #8408, #1772, #30656, #2253, #81301, #1309, #9321, #88407, #23557, #38204, #67118, #11670, #89319, #40519, #54285, #61873, #46243, #52882, #75147, #17850, #24474, #39583, #90704, #25865, #40062, #53353, #11204, #68980, #89793, #4110, #54746, #4567, #46701, #75603, #60022, #82238, #61425, #68039, #83155, #18307, #9804, #88860, #47164, #18786, #83624, #47645, #17394, #16912, #24009, #3641, #74680, #10259, #39127, #76547, #81762, #3165, #45770, #76073, #25406, #38678, #10727, #32982, #24957, #67583, #2711, #60944, #32050, #31593, #60482, #53833, #82699, #68506, #32532, #90257, #69437, #42409, #77960, #70852, #84100, #20657, #64251, #69906, #92133, #91668, #78421, #34856, #62344, #40985, #55243, #5984, #21114, #71798, #12620, #5045, #41940, #70397, #5525, #26352, #93080, #63769, #14024, #56175, #27768, #91184, #27288, #13559, #63302, #85033, #28234, #77011, #78876, #55708, #48107, #92598, #19249, #62835, #84559, #56662, #20183, #26821, #57122, #85963, #85511, #49063, #49982, #33926, #19706, #49527, #12139, #34395, #48577, #71320, #6450, #77477, #13102, #35325, #42885, #41466, #33441, #43356, #23449, #14951, #30086, #87357, #73644, #86902, #50460, #59443, #73183, #35794, #16340, #51378, #14499, #8302, #64707, #7369, #7826, #15886, #45190, #72706, #44273, #22507, #1204, #81194, #66541, #36716, #52317, #51840, #36250, #6920, #1662, #58970, #86423, #93534, #79810, #37633, #80269, #57578, #28692, #15407, #749, #30543, #37184, #87817, #21578, #66091, #88294, #79363, #43806, #72252, #65168, #29633, #22968, #274, #80733, #44742, #8754, #29154, #58051, #22057, #65636, #50926, #58512, #24364, #39476, #38092, #74564, #39953, #61315, #61762, #38574, #9693, #53242, #90595, #31943, #45656, #3999, #32874, #18668, #52773, #82124, #54636, #68869, #2138, #67477, #75041, #67002, #74093, #90153, #89678, #10153, #25301, #83049, #31027, #16800, #60834, #17281, #39020, #18201, #83510, #46138, #17741, #24845, #68396, #9212, #25755, #67935, #59914, #54179, #2606, #88756, #23902, #32416, #81652, #31486, #3058, #11087, #53728, #60374, #89213, #82594, #46595, #75494, #10618, #47053, #3526, #75956, #78313, #11559, #55599, #13452, #92971, #41353, #34283, #40407, #12993, #34746, #70742, #40875, #49423, #76898, #48465, #69325, #19139, #91554, #41831, #4454, #47994, #42303, #63661, #35210, #12028, #69793, #26711, #64138, #5418, #4926, #71212, #6339, #85854, #26234, #84447, #28129, #57018, #33332, #33812, #77365, #62229, #47534, #92484, #63191, #12501, #27651, #56550, #91060, #83992, #92021, #19597, #55127, #76438, #62724, #70285, #48947, #27176, #56063, #84916, #77845, #20066, #5876, #85405, #20553, #80158, #14845, #37514, #21468, #50344, #29521, #6817, #21946, #79250, #15296, #58401, #42768, #86787, #1091, #87247, #14391, #22393, #57475, #66424, #29040, #44153, #7717, #87702, #7264, #64605, #73528, #51265, #49874, #30426, #65518, #28583, #73060, #78772, #43250, #8637, #59317, #161, #86316, #8190, #57931, #50819, #13913, #80609, #37071, #1543, #43698, #65980, #71687, #79703, #29972, #72597, #36601, #15767, #36141, #58856, #22853, #637, #35691, #51719, #44626, #93431, #21007, #72148, #65060, #59796, #81079, #2013, #89091, #9564, #38903, #66876, #38452, #52649, #24721, #75378, #5182, #84220, #67812, #19367, #88637, #24243, #23785, #10491, #41108, #81529, #70040, #82476, #90031, #74433, #16223, #67358, #46019, #16677, #2937, #25183, #55368, #68276, #45532, #39360, #3398, #53117, #32289, #48232, #34056, #74922, #10033, #88168, #2488, #89553, #31365, #17623, #46474, #37968, #23327, #61194, #77135, #12266, #52197, #60254, #45074, #73974, #31823, #9091, #81997, #17153, #30906, #60714, #53605, #19835, #86092, #28358, #26943, #13684, #35919, #27903, #7494, #62958, #63895, #27415, #77607, #91792, #20320, #92731, #34981, #35462, #49190, #56791, #71928, #42536, #6584, #48703, #50111, #93662, #5647, #85633, #56303, #14161, #64381, #55831, #70521, #84686, #93206, #21242, #12758, #41599, #79006, #21719, #28822, #50594, #78085, #34522, #63429, #57250, #92258, #13228, #85169, #86548, #42063, #70977, #6110, #43025, #7050, #20780, #71447, #64837, #49652, #78546, #57705, #79488, #14623, #43481, #72377, #87474, #66205, #8420, #8872, #22622, #1321, #45310, #80858, #73760, #87024, #23570, #67132, #72826, #30203, #873, #81312, #37750, #65292, #43929, #58182, #66658, #24021, #74695, #15526, #7951, #44857, #73309, #37299, #29286, #2266, #1785, #16924, #59094, #30668, #396, #87935, #16458, #23086, #51968, #31149, #51496, #59571, #88421, #16005, #51043, #44401, #52437, #22175, #74215, #9334, #38217, #36846, #79931, #65763, #60035, #80384, #88872, #15067, #52895, #29752, #81774, #45783, #36379, #58633, #83172, #4580, #75159, #10741, #10272, #25880, #55257, #39141, #84112, #4125, #11684, #89810, #2725, #24972, #61440, #68052, #18322, #40535, #69450, #83638, #3179, #54761, #18802, #39598, #47660, #33455, #48120, #90270, #25421, #9817, #32063, #11222, #17863, #32996, #61887, #31605, #47178, #62358, #67597, #46715, #91199, #19262, #3658, #54299, #60494, #68994, #90719, #76561, #60958, #26368, #53846, #68521, #89331, #82712, #75617, #38690, #24486, #32547, #53366, #82252, #17407, #76088, #40077, #46255, #93548, #34870, #48591, #6934, #35807, #21594, #55721, #27302, #57591, #42900, #5060, #70413, #77976, #69920, #77024, #64266, #92613, #13117, #93095, #85978, #33943, #19721, #63783, #56190, #26833, #28706, #5538, #91682, #78437, #62848, #12636, #34409, #13573, #41953, #41483, #71814, #64721, #42423, #70866, #86435, #77491, #63316, #85525, #84573, #5997, #92147, #71335, #20671, #85049, #49077, #57137, #49542, #20198, #6465, #27783, #12152, #56677, #35342, #28249, #49996, #21128, #78891, #40997, #14038, #79377, #59931, #1216, #58063, #51855, #14514, #50940, #51390, #59455, #88770, #22519, #87830, #66105, #44756, #31041, #16353, #80281, #2151, #1675, #79822, #67016, #45204, #8767, #36264, #43369, #29647, #81208, #30100, #7383, #72265, #58982, #44288, #74106, #22981, #65648, #14963 ),
 ( #30557, #88306, #15420, #23464, #9226, #50474, #8315, #80747, #65184, #43819, #15899, #58526, #73656, #37645, #287, #29168, #66554, #38106, #86917, #22070, #7841, #72718, #36728, #52330, #762, #87371, #73195, #37197, #81667, #39036, #74579, #47069, #83065, #16814, #68414, #90611, #82609, #62246, #23917, #24860, #82140, #38588, #52788, #75056, #53743, #89693, #90169, #10167, #17756, #32891, #3544, #61332, #9707, #11104, #54654, #60389, #46609, #17296, #68885, #25317, #45673, #31500, #67491, #54196, #11575, #2622, #3073, #89227, #32432, #60851, #75511, #24379, #83528, #18219, #4472, #10633, #75976, #53257, #39492, #4016, #39970, #61778, #18687, #67949, #25772, #47550, #76455, #46152, #31957, #40424, #69341, #33349, #34765, #20086, #62742, #84008, #4947, #92040, #12521, #41849, #69811, #19156, #63209, #71230, #5894, #91574, #63679, #33833, #13931, #5436, #20570, #77863, #64155, #77383, #40893, #49893, #92503, #26252, #6833, #70762, #26730, #27671, #55146, #55617, #27194, #6356, #35707, #56082, #56569, #13013, #85422, #71706, #57035, #84934, #42789, #42320, #84465, #91081, #85873, #49442, #76917, #48012, #70305, #28146, #78330, #12046, #19616, #13471, #48967, #21024, #35230, #92988, #48484, #78789, #41371, #34303, #72614, #1560, #16240, #58417, #51281, #28601, #29989, #51735, #87719, #57951, #66441, #178, #65539, #86334, #36157, #14862, #58872, #57491, #65079, #30443, #80628, #52214, #29059, #86806, #43715, #81097, #22409, #21963, #88187, #23346, #9109, #43266, #7736, #45090, #59335, #21484, #50837, #654, #50364, #64621, #15784, #80174, #29538, #44643, #73544, #79267, #7280, #15312, #36617, #14408, #73991, #79720, #72164, #65996, #87264, #44171, #73078, #1107, #8209, #37087, #93447, #22870, #8653, #37530, #54074, #45550, #74450, #2956, #88654, #53134, #9583, #24742, #31841, #60272, #81546, #60731, #89108, #24260, #2033, #32310, #89570, #82944, #46036, #53624, #66893, #17172, #75396, #82015, #74941, #61213, #2504, #82494, #17642, #10051, #23803, #38921, #46493, #37985, #68294, #10509, #67830, #38471, #52666, #67375, #39379, #3415, #90048, #31382, #25200, #18096, #46950, #30923, #59813, #16694, #8501, #23650, #487, #29833, #29374, #44939, #74295, #58265, #9419, #23177, #30758, #15155, #21805, #44014, #80466, #87108, #37379, #59660, #88503, #8955, #22258, #73840, #37834, #58716, #66740, #52516, #67221, #15615, #44487, #28899, #51131, #30289, #36933, #52060, #80942, #72457, #57787, #16087, #81392, #16540, #45396, #80014, #79564, #86637, #66290, #43560, #72912, #8038, #38306, #50678, #65847, #14707, #1866, #88021, #7575, #73391, #36460, #87560, #65375, #955, #22706, #51580, #1402, #59176, #53456, #32148, #68137, #68605, #82337, #61049, #11304, #46794, #39681, #52983, #83255, #33076, #38772, #89892, #60579, #47258, #3742, #31230, #9898, #24102, #32624, #83724, #40614, #3258, #76172, #10821, #2802, #61514, #67676, #18884, #10354, #25501, #82791, #69073, #17485, #45875, #54842, #90346, #60116, #11762, #75696, #31685, #54379, #88955, #89414, #25050, #40156, #2353, #53923, #18399, #17943, #4201, #76637, #61965, #90802, #47739, #25961, #24568, #81857, #17006, #74781, #46337, #75239, #39219, #6549, #20288, #26450, #33536, #49162, #63399, #35428, #85133, #27868, #91284, #78055, #64350, #62441, #77574, #93176, #21208, #92228, #56274, #55339, #34952, #56761, #92698, #62928, #71417, #5147, #70490, #84190, #41080, #19805, #63864, #19338, #70004, #28328, #85602, #57218, #34024, #91762, #48673, #86058, #27384, #26914, #50078, #78973, #14125, #48201, #12725, #69530, #4663, #77102, #55801, #5618, #12233, #84653, #20749, #13196, #34493, #49620, #78516, #41568, #42032, #70946, #6078, #13653, #42505, #65259, #57673, #44368, #21681, #72344, #365, #73279, #72795, #7462, #8844, #37722, #8392, #36810, #59539, #43447, #36345, #51467, #50558, #43898, #29251, #37270, #80356, #64805, #42990, #30175, #1753, #66628, #30640, #58147, #93629, #81285, #15497, #79455, #86993, #22145, #88389, #7016, #51013, #14590, #66176, #1293, #79900, #87446, #15977, #7919, #71896, #15038, #65731, #842, #29723, #58605, #22592, #59059, #87907, #23058, #51936, #80826, #44829, #73732, #23540, #52410, #3625, #47149, #52867, #75132, #74664, #61409, #17834, #45283, #23994, #38187, #82684, #4094, #54731, #89302, #81746, #24939, #53337, #82222, #9305, #76058, #53816, #90689, #39111, #10711, #74186, #10242, #90241, #46228, #68024, #11187, #31578, #46686, #75588, #3151, #31119, #24458, #39568, #67101, #25390, #68490, #32034, #16896, #2235, #45754, #17376, #60467, #60929, #88845, #89776, #9788, #32513, #54270, #25849, #40047, #83140, #68964, #38663, #18291, #67567, #32965, #61858, #2696, #16431, #60005, #85497, #69891, #76532, #5030, #41450, #19233, #63285, #20644, #49514, #63753, #76994, #34842, #92583, #19690, #27752, #78406, #29501, #70382, #5510, #83609, #48090, #85016, #91653, #13087, #41925, #33425, #13545, #34380, #70836, #11654, #92118, #42393, #47628, #26806, #71305, #35310, #77462, #27272, #40501, #49048, #5968, #56647, #12123, #6435, #40968, #84543, #69420, #55228, #33910, #77943, #4551, #84083, #64235, #93065, #18770, #62819, #55692, #48559, #62329, #56159, #12605, #91169, #26335, #20168, #37052, #8621, #38887, #24224, #80136, #51703, #59301, #51247, #2921, #45515, #73957, #88149, #74416, #67341, #15276, #1074, #45058, #37498, #8168, #10017, #80591, #73039, #59779, #44134, #87683, #15747, #88621, #23306, #22835, #53100, #81978, #23768, #52180, #74905, #58838, #44607, #66859, #65963, #81062, #73511, #52633, #1994, #29954, #30410, #38432, #30886, #66407, #81513, #1523, #67796, #16207, #16660, #9072, #31349, #37951, #9546, #17134, #2472, #87226, #58382, #60237, #89075, #46000, #22373, #15091, #15553, #23593, #24045, #80406, #51994, #30226, #8897, #88896, #74238, #44425, #60058, #59594, #43951, #31172, #9358, #66681, #423, #7517, #87498, #45337, #59117, #65316, #72399, #87958, #8442, #23111, #37775, #52920, #38242, #73331, #14646, #88444, #72848, #43503, #67156, #1808, #29310, #36402, #22647, #2289, #16029, #58204, #87048, #44880, #37321, #22197, #73782, #30694, #51066, #52460, #79953, #7976, #51519, #36870, #65785, #66229, #1343, #894, #81334, #16481, #29777, #58656, #83664, #17429, #82734, #9839, #53392, #32086, #47200, #45810, #82277, #47683, #69017, #69473, #46278, #75182, #60987, #4605, #39622, #10295, #11707, #40559, #26393, #60518, #89835, #62381, #76584, #38712, #39165, #17886, #74719, #81799, #4148, #3685, #46738, #33019, #90745, #67619, #24510, #68546, #24996, #31627, #33478, #68077, #2747, #83197, #89354, #3202, #53868, #18345, #75641, #10764, #91226, #16946, #76114, #32570, #61462, #90293, #25445, #54322, #11247, #40101, #61910, #25903, #54785, #18828, #27328, #36638, #65096, #55745, #29078, #91705, #73098, #63340, #79737, #43284, #29556, #41509, #5086, #15333, #57969, #84135, #66015, #7297, #62872, #86823, #19285, #84597, #56214, #65558, #1127, #85073, #196, #19747, #22429, #51301, #21981, #50381, #8228, #48615, #77515, #50855, #41020, #21504, #12665, #14879, #43733, #77046, #79285, #672, #72633, #70437, #7753, #26857, #37106, #92171, #58437, #72181, #87282, #5563, #33967, #44194, #80194, #48144, #55281, #36177, #34434, #12177, #69943, #14426, #30945, #38942, #39400, #2054 ),
 ( #68315, #30008, #59833, #88210, #44664, #58893, #81117, #88674, #23823, #2526, #16260, #52686, #67851, #74475, #67398, #80650, #17195, #60751, #66463, #81567, #23367, #74962, #31403, #87739, #37552, #51761, #60293, #17663, #22891, #9129, #1581, #38493, #66917, #16715, #15805, #89592, #89130, #10533, #45570, #24281, #73565, #9605, #10074, #53156, #82038, #24762, #45110, #46056, #2977, #31862, #8674, #38006, #53645, #30463, #82515, #46516, #75417, #59359, #52234, #74012, #4375, #18581, #47916, #10999, #4842, #61235, #3918, #33253, #12415, #12911, #69247, #40794, #19061, #91476, #77762, #63109, #62150, #70203, #19515, #18120, #55040, #91937, #55517, #82967, #90070, #76355, #34204, #76819, #54095, #25222, #11945, #90979, #27091, #69711, #84366, #46972, #33726, #55978, #75874, #11481, #84832, #48858, #26146, #83909, #39867, #62636, #48382, #26627, #90514, #5336, #32794, #77285, #68788, #61683, #47446, #41266, #25678, #54557, #19981, #41749, #3439, #83425, #40331, #32333, #87169, #28501, #42212, #553, #29435, #15219, #49338, #20925, #51189, #36522, #92404, #64046, #71602, #63579, #70662, #57849, #86235, #6736, #86703, #79627, #27564, #13371, #57393, #49794, #20471, #22318, #92887, #85321, #72072, #56460, #6256, #28048, #7189, #35609, #35124, #65438, #58326, #36064, #64525, #80076, #71126, #56938, #79164, #78232, #93350, #85775, #64981, #14310, #78691, #42683, #50743, #43171, #13832, #84, #21387, #5791, #50256, #28964, #21867, #43621, #14768, #72518, #34665, #7638, #72977, #53528, #9961, #2414, #29897, #36993, #23245, #74848, #88566, #1019, #8107, #23714, #37897, #38833, #59723, #31294, #65905, #52577, #67740, #58781, #52123, #2866, #89480, #66802, #30827, #87624, #9484, #60180, #67284, #37442, #45941, #73452, #45000, #22775, #15684, #88087, #38371, #51644, #44549, #31750, #89018, #60642, #8563, #66351, #81005, #24640, #1932, #1466, #82403, #44075, #80530, #30352, #16148, #59241, #73902, #9018, #81457, #16606, #45461, #74361, #24165, #53046, #81921, #17073, #26516, #10422, #53988, #4265, #90408, #61121, #62998, #39749, #32214, #18948, #3324, #46862, #68675, #47803, #47323, #75766, #77173, #12303, #76704, #11370, #34095, #18009, #10886, #26031, #89959, #18464, #3809, #11830, #54914, #39286, #83318, #91356, #83794, #32690, #40681, #82857, #91828, #25565, #69599, #33143, #84258, #61576, #25114, #70080, #4729, #46403, #26982, #62033, #54445, #33607, #75303, #76239, #40221, #55405, #55872, #69137, #62515, #90867, #19408, #17551, #41147, #48271, #5223, #68205, #5682, #42573, #64875, #93242, #85205, #57287, #27451, #7532, #92770, #14200, #71489, #57743, #71014, #34556, #43518, #86129, #19873, #437, #35500, #92294, #21278, #48743, #20355, #85669, #93701, #29325, #56828, #28395, #6620, #79049, #65333, #50634, #20817, #86588, #7083, #63465, #64415, #79524, #43061, #70558, #77647, #63932, #21759, #50150, #41639, #12798, #71965, #78582, #14663, #35956, #28857, #56343, #72416, #36417, #49227, #27938, #84724, #78124, #13720, #13262, #42099, #6146, #35017, #49687, #51081, #36884, #22211, #79969, #58218, #15106, #43966, #7991, #87062, #65799, #72865, #911, #41239, #18095, #82943, #3896, #70180, #11457, #25199, #77263, #12393, #91915, #32308, #32773, #34183, #19494, #75395, #46949, #54535, #46492, #53623, #40771, #69224, #83404, #69689, #62612, #10508, #90047, #40309, #61661, #3414, #5314, #75851, #68293, #55016, #39377, #10974, #39843, #83888, #18554, #68766, #48360, #63086, #19038, #47422, #82493, #54073, #90493, #62126, #61212, #76332, #25652, #47893, #90957, #4353, #33230, #26122, #84343, #17641, #33701, #76796, #4819, #91454, #11922, #26604, #55495, #65419, #78670, #42663, #27069, #85298, #28481, #35105, #50238, #79142, #70642, #55956, #14291, #84810, #5770, #71102, #48832, #77738, #19960, #64504, #41726, #6235, #20447, #50722, #12889, #42189, #34644, #43151, #86216, #63554, #71580, #63, #85756, #92383, #27542, #28027, #49315, #56435, #78209, #13348, #56916, #92864, #93330, #64024, #20904, #36045, #6716, #57374, #49775, #72054, #57830, #13811, #35590, #21368, #7170, #64962, #28944, #86681, #21846, #79607, #14748, #43603, #72499, #7617, #36503, #37422, #66333, #87149, #60160, #37878, #74829, #23224, #88547, #29415, #59221, #45440, #30331, #52103, #88999, #15660, #30805, #66784, #88067, #15197, #73433, #1914, #58306, #74341, #59703, #80988, #65887, #22299, #8086, #1446, #44529, #44982, #72957, #8543, #58761, #23695, #81437, #9942, #24146, #73882, #53024, #997, #16130, #29877, #16584, #45920, #87603, #38815, #52559, #2396, #80511, #51170, #9000, #9465, #22749, #38350, #67263, #80057, #31273, #81902, #17055, #51624, #44057, #36973, #531, #82835, #18446, #46382, #17988, #32194, #4245, #54897, #77155, #62497, #47304, #91336, #39266, #68652, #68183, #83774, #19390, #3304, #48253, #62014, #69582, #53968, #60622, #46840, #25546, #61099, #76219, #4710, #33588, #47785, #89938, #18930, #76686, #3787, #11811, #26498, #12286, #54427, #83298, #67719, #25094, #69119, #75743, #90849, #26011, #17532, #2850, #40662, #31731, #75282, #10866, #89460, #24621, #53506, #11349, #82382, #39729, #32671, #55389, #10401, #61557, #90390, #84240, #33125, #40203, #85652, #14185, #6130, #79509, #41130, #42082, #5664, #55856, #70063, #92279, #70998, #13246, #13704, #27435, #35001, #50132, #20800, #78566, #91813, #28378, #71949, #77629, #63917, #34540, #86113, #42556, #5204, #48727, #62980, #71473, #28843, #34078, #20339, #12779, #49670, #78105, #92754, #26965, #7069, #6605, #21743, #27922, #35483, #84709, #56810, #21262, #64399, #93225, #35940, #56327, #57269, #79031, #43046, #19856, #64858, #93685, #41621, #57727, #86574, #50619, #70542, #63448, #85191, #49209, #61594, #46422, #68223, #11389, #31770, #46882, #82875, #10440, #31313, #89499, #18028, #45480, #90427, #54008, #39306, #81940, #9507, #24187, #17573, #60662, #61142, #89037, #24664, #74870, #75784, #3827, #26051, #40241, #89978, #69156, #17097, #75323, #45963, #32708, #62053, #9980, #90888, #10904, #18482, #2885, #38395, #53550, #3343, #38851, #25132, #47345, #76261, #25583, #67759, #54466, #83336, #32234, #4284, #33162, #54938, #39772, #68696, #16626, #82423, #74379, #67305, #2433, #60199, #53065, #83817, #62539, #18970, #76725, #69621, #47823, #40701, #11851, #4749, #91380, #26537, #33629, #9136, #43290, #678, #36183, #8681, #44671, #72187, #30015, #52242, #44200, #23830, #79291, #80200, #43739, #202, #14433, #36644, #15339, #51308, #51768, #65565, #73106, #88218, #58899, #22897, #65102, #66471, #16267, #21987, #8234, #72639, #30470, #80658, #7303, #86829, #29085, #15813, #66924, #57976, #58443, #50861, #87745, #79743, #37112, #14885, #1588, #30952, #7759, #59840, #73572, #81124, #29562, #87289, #22435, #66021, #1133, #37559, #45117, #74019, #59366, #23374, #38013, #2062, #88681, #32801, #47454, #90986, #10541, #68322, #52693, #17202, #54102, #60758, #75881, #11006, #2533, #81574, #39875, #16722, #31411, #2984, #74482, #9613, #45577, #90077, #67405, #31869, #46063, #76362, #38500, #67859, #60300, #68795, #18127, #89137, #3446, #25683, #17670, #24288, #53163, #53652, #74968, #82045, #10081, #38949, #82522, #24770, #25229, #89599, #46523, #61690, #32341, #82974, #75424, #3925, #83432, #39407, #61242, #46980, #90521, #54564, #18588 ),
 ( #11488, #40338, #69254, #4382, #33260, #62157, #63586, #48866, #91483, #19068, #33734, #27098, #41274, #70669, #4849, #70211, #84373, #56469, #13377, #35617, #20932, #5798, #49801, #27571, #83916, #26634, #55985, #35131, #64532, #91944, #92411, #41757, #20478, #6744, #85782, #84839, #92896, #42219, #40801, #77770, #78698, #78239, #11952, #47923, #5344, #56945, #34671, #76826, #69718, #85328, #19988, #13839, #49345, #71133, #62645, #6262, #42690, #55524, #34211, #71610, #26155, #12918, #64054, #19522, #28055, #55048, #48389, #77292, #12422, #63116, #561, #21393, #64988, #43628, #58788, #57400, #91, #59248, #80537, #81012, #57856, #28971, #72525, #16156, #51196, #86711, #23253, #52131, #37904, #72080, #7645, #73909, #88094, #50263, #21876, #29445, #86242, #93357, #15692, #15226, #58333, #44556, #8570, #79172, #36071, #80083, #36529, #43178, #45007, #50749, #14318, #1026, #7196, #79633, #14775, #29904, #87176, #65445, #9025, #28508, #87632, #22325, #44082, #72984, #8115, #37001, #65913, #22782, #51651, #73459, #37449, #66358, #1473, #30359, #75310, #67292, #39293, #9492, #83325, #74856, #89967, #53536, #39757, #53053, #16613, #25572, #68212, #1939, #76247, #17558, #74368, #2421, #32697, #53995, #54452, #31301, #60187, #17081, #18471, #24648, #38379, #90415, #47331, #11378, #45468, #45949, #66809, #61583, #88573, #89025, #67747, #59731, #30835, #82864, #82411, #2873, #18016, #75773, #23721, #24172, #46410, #9968, #81928, #52584, #38840, #81464, #3331, #31757, #60649, #89487, #32221, #10429, #61129, #25121, #46869, #10893, #68683, #3816, #40688, #69606, #48751, #26038, #41154, #4736, #5690, #77656, #62040, #12310, #20365, #12806, #33615, #41648, #76711, #56837, #48278, #63473, #26990, #13270, #26524, #83802, #92778, #70565, #69144, #78590, #84731, #47810, #34564, #4272, #62523, #70088, #49236, #40229, #5230, #92302, #55879, #27459, #20825, #6154, #34103, #42107, #56351, #54922, #91835, #35026, #85213, #18956, #33150, #19415, #71022, #19880, #90874, #11837, #78132, #63005, #63940, #27946, #85677, #91364, #55412, #84265, #77180, #21766, #44446, #59138, #7539, #448, #71497, #72874, #918, #36891, #7092, #15576, #43068, #14670, #35508, #79057, #57751, #7998, #6629, #14208, #86596, #65806, #64424, #71973, #73352, #29797, #1365, #35963, #64882, #50641, #30248, #65341, #93708, #37344, #66250, #52017, #86137, #79531, #87982, #8464, #93250, #28863, #43525, #28403, #13730, #58677, #29332, #72423, #87523, #22668, #57295, #50159, #58225, #36424, #21286, #23134, #87070, #22218, #15114, #51088, #79976, #43973, #51541, #80430, #42582, #48045, #76950, #47582, #76007, #4979, #82635, #17785, #90643, #67974, #83093, #46638, #76486, #25805, #10193, #54225, #62280, #54685, #75539, #83559, #24889, #33865, #90196, #11609, #68918, #55181, #68440, #31984, #40925, #18719, #17328, #91608, #32920, #89725, #40454, #46178, #10663, #18248, #91115, #26763, #47100, #69372, #4050, #4502, #62775, #12077, #11138, #84040, #33381, #3101, #40001, #69846, #26285, #60877, #75083, #61362, #19185, #61810, #39062, #53769, #82171, #39519, #3573, #32463, #25344, #77416, #35264, #86372, #19647, #63713, #21523, #7318, #49474, #42352, #48516, #21060, #42827, #78824, #49004, #57527, #84970, #56603, #12555, #28181, #78365, #70340, #34798, #57070, #84501, #35743, #93024, #13504, #27228, #41405, #63243, #85457, #70793, #6393, #92074, #5928, #20119, #85908, #71743, #65115, #50401, #64192, #79307, #56117, #20604, #77902, #6871, #36196, #13045, #218, #49927, #14448, #41882, #5466, #92538, #71265, #27705, #13969, #43305, #72200, #64657, #93485, #28638, #55648, #58913, #9152, #23846, #67422, #80672, #44686, #29098, #87302, #30487, #37129, #52259, #81139, #72652, #57991, #16283, #86845, #7774, #73120, #50874, #79756, #22004, #66487, #43753, #8247, #22449, #52712, #14897, #44213, #36659, #45134, #88233, #65579, #73587, #2078, #87759, #694, #29578, #30031, #51321, #58458, #80214, #15353, #22913, #1149, #1603, #66036, #51783, #38031, #8696, #59382, #15828, #74035, #59857, #37576, #23391, #66939, #30968, #88698, #81593, #16742, #45598, #74498, #9630, #38517, #75441, #10098, #11025, #39424, #68341, #89156, #62175, #39894, #76844, #25247, #90542, #31429, #61260, #47473, #32360, #54123, #91007, #17689, #32818, #11971, #46998, #38965, #3946, #60318, #3000, #3466, #11507, #40819, #90096, #68815, #18144, #25700, #2550, #26175, #82994, #69272, #18608, #17218, #75901, #55066, #54582, #82061, #24305, #10559, #33280, #61708, #53183, #46079, #83454, #76380, #83935, #40355, #4401, #74987, #19088, #47941, #67877, #31886, #60777, #89617, #24787, #53669, #82538, #46539, #56961, #92912, #63135, #71627, #5363, #70687, #91498, #41293, #20010, #35151, #33752, #70228, #35634, #85798, #57420, #34229, #91964, #48888, #86259, #27593, #27119, #93375, #28525, #14335, #48407, #77789, #50285, #64551, #26654, #56003, #5817, #62664, #69738, #20949, #85348, #34691, #49817, #78714, #55543, #12445, #56489, #12937, #19541, #21410, #84858, #84392, #71151, #77310, #41777, #63605, #6280, #92429, #20496, #79191, #4870, #64072, #49363, #78257, #13395, #42238, #28074, #13856, #42711, #6760, #8584, #51664, #65005, #15240, #23267, #80553, #43645, #15708, #79648, #59743, #51210, #66371, #29918, #16169, #29461, #86728, #1957, #44569, #72096, #7213, #52596, #87647, #50764, #73472, #36086, #72541, #44096, #52145, #81477, #73002, #37462, #58802, #1489, #23733, #9038, #8130, #45021, #59263, #57874, #1040, #37916, #30372, #28986, #107, #22339, #73921, #22797, #21892, #14790, #88111, #37014, #66820, #81025, #30850, #7660, #88585, #43195, #36545, #80101, #65461, #577, #65928, #58349, #87190, #10179, #31969, #67959, #38117, #46622, #74118, #45684, #66565, #16365, #88781, #39048, #8779, #45216, #10644, #60862, #32444, #9238, #67027, #23929, #61345, #2633, #2163, #68425, #3555, #83077, #23475, #52799, #25328, #39504, #1687, #31053, #74591, #37657, #44768, #89705, #60400, #9719, #24872, #53754, #30568, #81219, #31512, #81678, #88319, #90180, #16827, #59466, #46164, #52341, #38599, #67503, #75067, #89238, #24391, #54208, #73668, #3084, #53269, #82152, #17307, #82620, #17767, #75522, #19167, #47561, #77395, #26742, #39982, #84019, #92052, #55628, #18698, #84477, #54666, #34776, #26263, #41383, #4959, #84947, #4483, #61790, #70773, #19627, #91092, #48979, #62753, #68897, #75987, #91585, #12057, #77876, #33844, #70316, #4029, #48496, #13024, #11115, #55157, #41860, #63691, #40904, #12532, #32902, #5446, #34314, #63220, #11588, #20097, #76466, #48024, #90622, #83539, #62259, #27206, #25785, #40435, #5906, #56093, #92516, #69353, #33360, #76929, #27682, #69824, #56580, #18230, #47081, #30001, #64167, #35718, #66008, #51294, #13483, #78799, #86346, #78341, #85433, #72626, #7291, #21497, #7747, #666, #42330, #28157, #72175, #64632, #35241, #37099, #13944, #6370, #86817, #71241, #21036, #42801, #21975, #50375, #49904, #80186, #15325, #50848, #79279, #8221, #85884, #71717, #190, #92999, #14420, #6844, #79731, #29071, #57047, #57502, #65552, #57963, #93459, #14873, #28613, #1120, #43277, #43727, #36170, #58430, #65090, #36631, #44186, #29550, #20582, #49453, #87276, #22422, #73091, #22884, #59351, #59826, #67844, #68308, #30937, #2519, #74467, #53149, #39393, #24756 ),
 ( #38935, #31396, #81560, #30456, #51753, #66456, #88667, #74005, #9598, #37545, #9122, #23360, #89123, #46050, #3431, #53638, #38485, #82508, #88202, #23816, #52227, #74955, #10526, #81110, #58886, #82030, #60744, #45103, #80643, #37999, #16708, #16253, #67390, #89585, #17656, #2970, #66909, #10066, #31855, #52679, #46508, #75410, #87732, #45563, #60286, #15798, #2047, #24274, #17188, #44657, #73558, #8667, #1574, #19508, #90063, #75867, #76347, #54088, #82959, #70655, #69704, #46965, #11473, #25670, #55971, #25215, #47438, #18113, #55510, #91468, #10991, #76812, #5329, #90972, #32326, #61228, #33246, #90508, #39860, #68782, #83418, #62142, #4368, #4834, #18573, #26138, #41257, #11937, #33718, #3911, #48376, #63101, #32788, #55033, #54550, #77278, #62629, #61676, #40324, #69239, #26619, #19973, #83902, #19053, #47909, #40786, #84358, #12407, #70196, #91929, #34197, #12903, #27084, #84824, #48849, #77754, #41742, #65431, #86696, #87162, #64037, #35117, #49787, #22311, #57387, #71118, #29428, #58318, #44068, #78224, #78684, #80069, #545, #27557, #92879, #6729, #92397, #5783, #21861, #21380, #35602, #50735, #14761, #56452, #42204, #86229, #13824, #49330, #51182, #28041, #20463, #7182, #85314, #56931, #85768, #36057, #64517, #20918, #15212, #34657, #64975, #93343, #63571, #6248, #42676, #14304, #13363, #28494, #71593, #78, #43164, #50250, #79156, #79619, #72065, #28956, #57842, #43615, #72511, #7631, #36516, #58774, #51637, #65898, #8099, #80523, #87616, #72970, #36986, #15676, #22767, #1010, #29890, #68880, #69336, #77378, #77858, #40418, #12041, #84003, #62737, #48961, #34297, #4467, #41366, #84460, #83060, #26247, #63204, #26724, #54190, #61326, #47545, #5431, #19151, #25312, #32427, #48007, #62241, #92034, #76911, #55611, #90164, #40888, #27189, #18214, #76449, #56076, #20081, #91076, #55140, #47064, #33828, #19610, #91568, #61773, #70300, #4010, #33344, #75970, #39964, #69806, #32886, #48479, #13008, #90606, #68409, #12516, #84929, #54649, #11099, #83523, #4942, #25767, #3538, #18681, #11570, #21958, #35224, #86800, #50831, #71700, #79715, #36612, #80169, #93442, #57486, #41844, #6351, #43261, #49887, #65074, #173, #85417, #70756, #29053, #5889, #20565, #85868, #63674, #92497, #34759, #79262, #56564, #21019, #64150, #65532, #27666, #57030, #49437, #57945, #7275, #78325, #86328, #14857, #6828, #13465, #42315, #42783, #92983, #71224, #28141, #78784, #35702, #13925, #14402, #64616, #28596, #43710, #21479, #72159, #50357, #72609, #7731, #36152, #649, #29532, #58412, #87258, #22404, #51276, #37082, #81541, #2950, #54886, #88181, #22865, #23797, #52209, #81091, #8203, #74936, #52661, #90840, #37980, #9577, #44166, #73986, #60266, #45085, #66888, #10046, #30438, #45544, #16689, #9103, #29983, #23341, #74445, #73072, #89103, #38466, #2027, #80623, #65991, #51730, #16235, #59330, #59808, #87714, #88649, #73539, #67370, #2499, #26001, #38916, #31377, #67825, #31836, #1102, #24255, #58867, #53129, #82009, #15779, #17166, #46031, #62005, #15307, #44637, #8648, #37525, #66435, #1555, #41121, #19847, #55847, #56318, #70053, #48718, #92745, #34533, #27428, #40653, #70991, #20793, #26489, #77621, #48245, #34994, #85183, #18921, #91327, #11802, #20332, #71465, #28370, #62970, #55379, #92272, #26956, #84700, #76677, #49664, #49202, #64392, #12770, #78098, #47775, #41612, #63910, #70534, #5658, #78559, #5195, #13239, #42075, #63441, #4701, #91804, #6123, #69572, #27916, #56803, #85645, #84231, #33578, #19381, #13697, #34068, #42549, #62487, #6597, #77147, #35475, #93218, #83765, #12277, #36860, #51984, #28834, #58194, #57718, #73323, #8889, #86564, #37767, #51510, #59108, #43494, #50124, #72390, #15082, #21733, #65776, #87950, #23102, #37313, #50610, #8434, #66221, #87038, #1335, #80873, #1800, #43942, #72839, #57262, #79500, #58646, #65305, #80398, #15543, #7061, #86105, #44415, #21254, #35931, #7507, #79022, #14176, #43038, #885, #71940, #36392, #14636, #30217, #412, #16021, #29299, #22188, #64849, #51056, #79944, #22638, #93676, #7966, #44872, #73774, #66672, #29768, #87488, #74711, #47192, #82268, #2281, #54314, #83189, #69009, #9349, #9832, #11238, #90285, #52452, #24036, #31620, #23585, #30685, #17878, #46270, #60511, #46730, #39613, #81326, #67147, #17421, #38705, #74230, #76105, #52912, #45329, #32078, #16473, #60050, #81791, #60978, #89346, #88888, #25436, #18337, #89826, #24502, #40093, #31164, #16939, #39157, #38234, #53383, #45801, #24987, #68069, #67612, #2740, #10756, #3194, #75174, #53860, #10287, #59585, #82726, #75633, #68537, #3676, #32562, #61454, #88436, #70428, #33011, #13587, #48606, #11699, #5554, #61902, #4597, #5077, #13132, #42439, #69935, #41499, #19738, #92162, #78451, #63798, #33959, #70881, #20215, #18818, #55736, #92627, #56205, #83654, #90737, #77038, #34887, #77506, #54777, #25895, #12653, #91696, #27798, #34424, #85064, #47675, #63331, #56691, #76576, #12169, #85538, #49556, #26848, #84588, #40550, #27319, #49093, #69465, #33470, #20686, #77992, #4140, #62373, #91216, #48135, #26384, #41968, #55272, #84127, #19277, #41012, #62863, #6012, #51868, #37209, #93108, #64735, #72276, #64279, #15912, #58539, #86929, #7395, #87384, #80295, #28263, #14052, #58076, #50487, #21142, #22993, #93563, #85992, #72733, #57152, #6948, #28720, #7853, #36277, #35821, #1230, #30112, #36740, #65197, #87843, #71829, #57605, #79835, #50012, #300, #86448, #65661, #14975, #78905, #43381, #51403, #43831, #21606, #775, #42915, #80760, #79389, #29659, #22082, #44300, #14526, #29180, #58994, #22531, #6480, #71349, #50952, #15434, #73208, #35357, #8327, #14995, #23011, #23494, #79856, #51423, #29678, #8346, #88343, #73687, #43854, #80783, #30131, #28743, #65684, #8797, #66134, #93584, #6969, #86950, #44786, #58561, #64759, #71849, #87402, #7873, #37676, #22549, #1249, #35842, #15452, #66585, #57626, #22103, #1705, #59490, #36763, #798, #86469, #73235, #59015, #37229, #7417, #15932, #43402, #72752, #21634, #79411, #58104, #87862, #320, #44323, #51890, #30588, #29204, #52362, #14077, #42942, #50513, #14546, #72297, #36299, #50972, #31530, #52817, #60879, #10195, #81237, #59959, #9257, #39064, #68442, #16384, #67521, #88798, #75085, #2651, #60417, #38134, #10666, #67977, #61364, #24408, #31986, #74139, #53287, #53771, #89257, #82173, #39521, #9742, #3103, #89727, #17330, #2186, #38617, #24891, #45234, #75541, #82637, #17787, #45701, #31071, #16845, #46180, #46640, #3575, #81697, #32465, #67049, #23945, #74613, #26056, #85698, #70583, #20844, #91386, #27008, #55429, #13289, #42603, #84282, #71518, #85235, #56857, #12327, #83823, #41171, #48768, #48296, #5709, #49715, #13755, #71043, #70110, #6177, #63960, #19897, #54943, #18975, #47828, #77674, #34584, #76730, #5250, #27479, #63022, #49256, #78151, #40706, #11857, #69626, #4754, #71995, #14691, #7113, #43546, #8940, #58699, #36446, #65361, #87092, #88005, #57316, #22242, #15136, #51563, #30269, #23158, #16071, #44925, #73827, #64445, #93271, #38758, #2337, #52501, #66725, #25037, #61031, #31216, #39668, #67201, #67662, #59642, #9404, #81842, #3244, #1852, #38288, #3726, #53909, #25487, #60101, #88940, #16992, #54366, #89400, #24088, #61501, #90333, #76156, #16526, #45857, #18387, #32611, #88489, #52965 ),
 ( #32135, #31669, #83240, #74763, #9882, #46322, #23636, #2788, #60562, #89877, #75226, #81378, #24554, #17929, #10340, #53438, #39206, #74281, #47244, #82321, #82776, #17472, #10806, #68119, #45378, #37818, #46780, #30739, #75681, #68590, #18869, #12709, #69059, #11749, #12218, #20266, #20732, #77087, #48659, #26898, #5601, #85585, #70930, #41064, #78039, #27367, #25948, #62911, #6061, #63381, #90788, #4188, #84176, #42014, #55786, #61951, #33062, #84639, #5130, #34933, #19788, #92211, #54829, #77560, #63848, #83707, #19324, #92680, #56739, #34007, #91747, #47726, #70473, #26433, #41549, #34475, #56256, #76626, #48186, #85116, #40143, #49142, #13179, #27850, #40602, #69516, #4647, #69990, #55326, #49602, #33522, #11289, #62428, #91269, #65712, #87886, #73261, #58129, #8373, #50060, #79437, #78956, #824, #30156, #14106, #59039, #72777, #80338, #64786, #71400, #93611, #36327, #42970, #86974, #15480, #44351, #58588, #71875, #29705, #87427, #14573, #22574, #37253, #23039, #65241, #347, #78498, #6997, #79881, #86500, #7902, #36792, #28310, #13636, #51448, #42487, #57199, #28769, #6533, #35409, #64329, #22128, #93155, #57652, #35869, #66158, #86040, #21663, #21189, #1274, #43881, #50539, #29234, #43429, #72324, #7445, #50996, #15021, #16410, #66608, #80807, #9282, #81724, #23973, #24434, #38165, #16873, #60908, #2676, #89282, #8823, #39088, #82661, #88369, #45731, #45262, #3130, #53316, #15956, #59520, #73713, #82200, #39546, #90220, #31098, #23519, #60447, #88824, #52847, #44811, #17810, #17355, #32491, #74642, #46206, #37703, #9768, #32010, #38644, #67547, #46663, #75567, #51917, #30618, #2214, #61388, #10689, #1731, #74166, #31555, #52388, #81265, #68001, #75111, #10221, #89755, #24916, #67080, #59985, #53793, #68469, #3604, #70817, #47608, #40027, #26786, #11167, #54709, #76511, #55673, #55207, #83586, #84992, #20147, #84524, #19210, #41904, #25830, #18750, #33890, #68944, #26312, #11634, #19671, #62797, #47125, #91145, #5488, #91632, #40480, #48539, #61837, #5950, #33406, #77440, #12102, #92097, #69397, #4074, #77926, #12584, #54250, #34822, #69869, #32945, #41431, #83120, #4529, #84061, #34361, #63735, #48069, #70363, #40947, #63266, #25369, #49030, #76972, #27253, #56139, #90670, #5007, #13068, #18271, #62305, #76038, #71767, #29599, #43325, #49496, #56628, #72221, #86392, #58478, #14468, #50894, #20625, #7337, #87322, #85478, #6890, #22470, #44234, #21543, #79331, #78385, #58014, #79775, #22024, #85930, #714, #28202, #93504, #13526, #64215, #42851, #86870, #42374, #93045, #51342, #14918, #80236, #57090, #21080, #35764, #15372, #50426, #49951, #73143, #78844, #64677, #8269, #36217, #13990, #37149, #92560, #27731, #71286, #28659, #6413, #35288, #57547, #65137, #238, #29118, #43773, #72674, #7794, #36679, #65601, #75007, #58933, #8718, #52733, #45157, #15849, #17708, #88257, #80695, #67443, #51803, #1625, #23415, #2570, #2101, #30508, #31907, #60799, #31449, #59879, #82560, #66506, #59403, #74520, #44706, #66962, #52281, #60338, #9655, #87783, #38053, #46102, #38540, #81160, #89175, #37595, #46561, #74056, #24327, #81616, #38985, #16304, #73607, #24807, #53204, #1169, #75460, #16765, #9175, #82082, #30052, #30992, #88719, #10119, #10581, #23867, #17240, #45618, #67898, #66056, #89637, #3021, #53693, #22933, #54145, #91027, #5386, #91521, #25268, #32381, #18631, #70251, #83959, #90116, #3488, #19108, #33299, #34251, #55090, #26677, #61282, #47963, #63157, #83014, #47497, #91988, #84881, #62197, #26196, #18166, #4891, #55567, #62688, #32840, #41314, #68838, #40375, #47019, #11047, #83475, #33775, #75921, #39917, #27141, #84415, #56026, #3966, #20032, #48909, #61730, #90562, #69292, #25720, #77811, #19563, #76867, #4421, #48429, #77333, #54604, #76406, #11992, #11528, #40841, #39444, #69760, #12467, #68360, #92452, #42264, #64096, #14357, #42733, #71177, #72563, #7685, #72118, #6781, #29485, #13419, #6306, #21435, #27615, #13880, #35174, #7234, #50309, #34713, #78737, #86751, #79214, #92936, #43217, #49389, #58370, #20973, #36109, #93398, #79672, #28097, #56512, #65485, #65027, #41799, #22360, #57441, #20521, #127, #70710, #56984, #71648, #21913, #51234, #35658, #29010, #28550, #57895, #87212, #36570, #64573, #14813, #50787, #85371, #86282, #602, #43668, #78281, #5841, #85822, #12960, #63627, #49840, #45393, #32147, #75238, #18398, #3257, #39680, #9417, #61046, #47257, #74293, #89412, #76170, #33075, #10353, #68136, #38303, #46793, #68603, #10820, #74778, #83254, #17004, #82334, #67218, #52980, #31683, #75695, #2351, #81854, #11302, #3739, #69072, #45872, #9896, #60577, #4200, #39218, #38770, #40155, #61964, #25960, #60114, #24566, #31228, #90801, #67674, #88953, #82790, #24100, #2800, #53453, #17942, #17484, #46336, #80122, #15261, #32623, #89890, #25049, #53922, #61513, #90345, #25500, #54378, #84189, #20286, #63398, #76636, #26913, #34951, #92227, #55338, #27383, #91282, #71416, #62927, #78054, #41566, #27866, #41079, #4662, #13652, #56273, #83722, #64348, #5617, #62440, #85132, #18882, #19337, #55800, #63863, #93175, #84652, #49160, #70489, #13195, #35426, #20748, #19804, #56759, #70945, #69529, #12723, #49619, #42031, #40613, #47738, #34022, #85601, #34492, #11761, #33535, #6077, #48672, #78515, #92697, #42504, #26448, #6548, #54841, #48200, #91761, #77101, #12232, #77573, #70003, #5145, #87445, #15496, #51466, #21680, #30173, #57672, #29250, #50077, #93628, #72342, #22591, #86057, #28786, #87904, #44367, #15974, #86516, #50556, #7461, #44827, #79899, #79453, #51934, #80824, #66626, #7015, #36343, #8842, #23056, #78972, #14589, #58145, #21207, #28327, #73278, #43897, #86991, #8390, #37269, #14124, #64804, #15037, #65258, #42988, #57217, #66175, #72794, #22144, #1291, #59056, #71894, #43446, #7918, #364, #35887, #73730, #51012, #36809, #29722, #65729, #840, #58604, #80355, #37720, #60003, #61406, #90239, #60927, #89300, #18289, #2233, #31116, #10240, #81283, #2694, #88843, #89774, #39108, #23537, #67565, #75586, #68022, #23992, #3149, #38184, #47146, #9786, #24937, #82220, #68487, #81743, #45281, #54268, #32031, #30638, #11185, #46226, #9302, #53814, #59537, #52865, #31576, #10709, #40045, #60465, #82682, #17374, #17832, #76055, #25388, #24455, #3623, #46684, #16429, #53334, #83138, #39565, #74184, #88387, #74662, #32510, #75130, #52407, #67099, #1750, #16893, #45750, #38661, #27269, #90687, #48556, #5965, #32963, #76991, #34839, #20641, #62816, #55689, #61856, #34377, #56156, #92115, #62325, #70833, #4548, #69887, #25847, #40499, #19229, #63282, #54728, #69417, #63750, #85012, #56644, #33422, #91165, #48087, #85494, #26803, #26332, #92579, #27748, #13542, #47626, #12120, #49511, #78403, #83606, #55225, #5026, #84079, #68961, #4092, #20164, #91649, #18768, #40965, #33907, #77457, #76529, #84540, #19687, #49045, #12601, #11652, #41447, #77940, #70379, #5506, #13084, #41922, #58950, #50443, #65616, #29135, #15386, #28675, #85945, #1184, #14933, #71302, #51821, #86884, #49966, #43788, #6431, #42867, #43339, #51359, #80713, #14481, #79791, #58030, #36696, #22947, #8283, #72236, #44251, #58492, #57106, #253, #37163, #728, #28218, #35306, #21559, #73163, #22038, #93062, #64232, #50907, #36232, #66072, #72688, #29614, #21098, #7807, #30065, #78857 ),
 ( #87798, #87337, #14007, #42390, #71781, #6903, #35778, #86405, #64691, #93517, #57562, #79346, #7350, #65150, #22486, #80250, #31466, #45633, #3038, #24824, #8735, #52298, #2586, #88736, #59422, #61298, #38070, #30522, #17259, #1642, #45171, #66980, #46118, #74541, #90133, #2118, #88274, #75021, #23430, #74073, #31008, #10134, #9672, #9192, #75476, #10601, #39000, #38555, #32399, #16319, #59894, #24344, #81175, #16779, #23882, #67914, #53219, #37612, #81632, #89655, #82100, #52750, #31921, #67457, #25284, #60354, #60813, #89191, #82575, #53708, #17723, #68377, #46578, #44723, #54161, #39460, #3507, #15866, #73623, #66523, #83975, #92004, #92466, #55109, #26694, #4907, #77349, #63644, #48928, #19123, #56045, #5402, #3981, #40859, #77826, #41333, #68852, #75937, #62212, #20048, #33792, #39935, #47036, #62707, #76882, #12976, #91537, #70268, #11065, #55583, #41814, #32856, #91042, #70725, #34728, #12009, #69777, #61745, #48448, #34267, #12483, #76421, #84899, #18648, #47978, #90577, #54619, #33316, #63174, #25737, #83491, #5857, #27157, #27632, #47515, #11543, #26214, #83030, #84431, #40390, #18184, #69308, #4436, #19579, #6799, #37053, #22375, #78296, #49855, #57456, #49406, #1075, #43681, #72131, #86298, #72577, #65498, #13435, #92952, #43233, #35673, #6321, #42282, #28565, #36584, #65040, #57000, #29023, #28112, #73040, #64588, #79685, #7247, #29502, #42749, #35189, #15277, #57910, #85387, #65964, #36123, #64115, #86765, #20536, #85837, #21451, #616, #56530, #50324, #143, #21927, #50800, #71194, #51248, #79230, #58383, #7699, #20988, #14372, #80137, #14827, #78754, #13895, #93413, #87227, #44135, #71665, #8169, #74418, #23769, #60700, #45516, #81979, #51704, #9547, #89539, #87684, #37953, #24703, #75362, #52634, #16661, #22836, #89076, #17136, #53101, #23307, #31807, #59302, #30887, #80592, #1525, #73958, #24225, #15748, #30411, #53588, #46001, #17609, #88150, #52181, #9073, #46460, #81514, #81063, #82461, #10477, #68262, #8622, #66860, #39343, #29955, #44608, #16208, #59780, #73512, #58840, #74906, #38433, #88622, #10018, #38888, #37499, #66408, #67342, #1995, #45059, #2473, #31350, #60238, #67797, #2922, #68734, #61633, #19009, #76302, #3865, #84313, #19464, #47862, #40279, #41209, #39812, #32745, #26092, #54043, #11427, #90466, #76765, #54981, #47391, #90015, #10946, #54505, #11893, #32272, #25623, #48331, #40742, #77232, #83376, #18525, #69196, #70147, #4325, #33202, #12361, #5283, #34152, #46920, #62093, #3384, #61178, #75822, #90926, #83857, #82913, #25169, #55463, #69659, #4789, #18067, #33669, #26574, #62579, #91421, #67185, #37803, #39651, #16512, #8925, #89383, #73812, #23620, #45363, #24538, #24073, #52487, #53894, #82762, #53422, #81826, #10790, #88473, #81362, #2773, #66709, #88925, #74266, #82305, #31654, #16056, #60086, #68104, #60545, #9389, #17456, #30725, #68574, #2320, #46306, #74746, #61016, #38273, #1838, #46765, #75210, #23143, #3711, #38742, #59625, #10325, #52025, #31201, #52949, #3229, #32596, #16977, #39192, #9867, #32120, #87990, #17914, #45842, #89862, #25022, #67647, #75666, #80911, #44909, #47230, #54351, #40587, #92196, #12203, #18370, #25472, #41047, #55308, #27352, #77072, #19772, #83225, #69974, #56239, #76140, #69501, #85101, #13163, #84161, #48171, #11274, #26884, #48642, #84624, #54814, #63366, #90772, #91254, #19309, #20251, #76611, #91731, #33992, #5114, #40127, #4632, #62895, #90318, #41533, #55771, #77543, #33046, #69044, #4173, #62412, #11734, #12693, #61936, #33506, #25931, #70459, #5586, #70913, #49127, #34458, #78023, #83692, #26418, #18853, #41999, #6046, #47711, #61486, #29216, #36775, #21174, #27835, #50043, #86481, #64314, #14557, #65695, #809, #15007, #28294, #79867, #43866, #64771, #72763, #29689, #73246, #21646, #50524, #34918, #93139, #36310, #42954, #58115, #86960, #78483, #63831, #22113, #92663, #13619, #78939, #56724, #85570, #20717, #72309, #49587, #14089, #57184, #58573, #42472, #71860, #71383, #50982, #331, #6516, #79422, #7885, #93596, #35394, #86025, #35854, #6981, #28754, #57637, #43414, #7430, #65226, #87413, #22560, #51434, #80323, #15463, #44335, #59026, #89268, #39074, #44796, #67062, #66595, #53299, #9754, #37240, #15942, #30142, #74625, #89739, #46650, #81248, #73699, #16857, #45246, #74151, #1260, #67987, #45713, #82648, #31082, #2661, #66144, #2198, #82184, #81708, #3113, #31996, #17340, #1716, #46191, #75096, #38146, #10205, #60889, #8357, #59970, #23955, #87873, #30600, #38628, #16395, #31540, #60428, #51901, #23023, #24418, #80794, #8808, #52373, #37689, #59503, #88354, #67531, #23505, #9268, #88808, #24901, #52830, #53781, #17797, #6284, #42242, #39531, #27595, #49821, #41779, #21414, #75552, #77791, #41295, #90207, #10676, #34231, #12940, #48890, #49367, #63137, #70689, #85802, #56492, #20499, #32477, #64076, #13859, #19543, #5819, #70230, #28077, #78261, #68453, #83105, #3587, #13398, #64555, #61374, #56005, #48409, #85351, #20012, #34693, #25356, #42714, #71155, #57423, #63607, #35155, #54236, #92431, #56965, #92915, #20953, #71631, #91966, #78718, #6763, #35637, #77312, #84861, #93379, #12447, #28530, #86263, #5365, #27122, #43198, #57877, #51213, #65465, #1043, #28989, #582, #14794, #80558, #37466, #59747, #45024, #29922, #73924, #21895, #80104, #50768, #66375, #1961, #79653, #30854, #44573, #52148, #36549, #72099, #29465, #8134, #43649, #50289, #1492, #14339, #110, #58354, #7216, #36089, #88588, #87650, #65009, #87194, #72545, #9041, #86732, #22342, #7666, #73476, #15712, #15243, #58806, #23272, #44100, #79196, #73006, #37017, #65931, #22801, #51668, #8588, #30376, #59267, #88115, #81028, #16172, #37919, #66823, #61146, #74382, #10908, #54471, #60202, #82426, #81943, #68702, #25135, #52599, #31316, #45483, #89981, #11394, #62058, #2888, #89040, #32237, #60665, #89502, #16629, #83341, #54011, #4289, #46425, #18032, #81480, #17576, #3832, #53554, #75327, #18487, #38855, #82878, #46886, #10443, #38399, #31773, #75788, #9510, #32714, #39776, #39309, #24190, #67308, #53068, #24667, #67762, #68226, #2437, #3346, #17100, #61599, #90432, #33167, #47350, #25588, #76267, #45967, #40246, #74873, #69162, #23736, #9983, #30498, #73130, #80682, #65124, #71755, #227, #36669, #14457, #58467, #15838, #44695, #58922, #72210, #30041, #87770, #14907, #22922, #73596, #23403, #65590, #704, #78833, #43314, #80224, #86858, #8257, #37138, #28647, #36206, #43763, #51792, #29588, #22458, #35753, #66046, #8707, #21532, #72663, #7326, #37585, #15361, #13979, #86381, #6880, #51331, #66496, #42838, #58002, #50413, #87311, #22013, #50883, #64666, #1613, #44222, #59392, #7783, #1158, #93494, #88244, #57537, #79319, #29107, #79765, #67432, #82547, #24794, #46089, #66950, #31438, #53679, #81149, #32368, #89626, #74996, #23856, #45146, #59868, #53193, #2559, #3010, #30979, #60328, #16753, #17697, #39433, #61717, #47007, #31895, #75911, #52722, #82071, #81605, #68349, #3955, #45608, #32828, #46549, #54132, #38528, #74045, #89165, #10108, #74510, #60788, #83002, #18154, #61269, #9641, #3477, #90104, #17227, #25255, #11036, #90550, #38975, #67887, #52269, #24315, #75450, #10568, #39904, #68825, #2089, #16293, #9163, #38042, #88708, #69746, #47483, #76392, #64082, #63144, #40363, #4878, #19097 ),
 ( #5827, #47950, #70696, #34699, #55552, #63613, #20505, #25709, #77319, #41301, #54591, #83944, #27128, #33762, #48896, #77797, #69280, #83463, #12947, #18619, #4409, #62673, #11516, #33288, #62183, #91974, #91016, #91507, #76853, #49374, #26184, #40827, #55075, #41785, #84867, #11979, #70237, #92437, #84401, #26663, #19550, #48416, #12453, #5371, #34238, #56011, #20018, #27601, #56498, #85357, #78267, #13406, #42249, #71162, #6290, #35160, #31217, #36915, #59161, #58700, #45379, #1853, #28082, #8020, #22243, #66726, #81843, #38759, #73374, #65832, #8941, #37365, #66272, #87093, #60102, #37819, #74765, #23159, #88490, #58249, #88006, #74282, #30270, #52043, #88941, #15596, #30740, #59644, #80928, #15137, #8486, #23637, #51113, #9405, #52502, #16072, #939, #79999, #29818, #1387, #44469, #44926, #72896, #73828, #87543, #81379, #16527, #9883, #24089, #38289, #52966, #22690, #67203, #51564, #2338, #45858, #80451, #92921, #16993, #43999, #53910, #60563, #46781, #4648, #18388, #24555, #31670, #47245, #61502, #33523, #83241, #25949, #89401, #76157, #62429, #53439, #75682, #91270, #19325, #90334, #54367, #82322, #33064, #54830, #90789, #61032, #69517, #3245, #68591, #17473, #39207, #17930, #61952, #46323, #68120, #26435, #83708, #55327, #32136, #89878, #10807, #84177, #25488, #25038, #48187, #77088, #12219, #75227, #39669, #67663, #2789, #10341, #82777, #3727, #32612, #11290, #18870, #40144, #69060, #47727, #76627, #4189, #11750, #40603, #20268, #84640, #86502, #63383, #55787, #42489, #26899, #70475, #92213, #71402, #70932, #5603, #6999, #35871, #6535, #34935, #57654, #41551, #34477, #49604, #19790, #42016, #27369, #35411, #78500, #62912, #13182, #21191, #13638, #56258, #64331, #77561, #21665, #49144, #93157, #27852, #14108, #85118, #48660, #93613, #28312, #69991, #50541, #85587, #12710, #57201, #5131, #78041, #6063, #50062, #79439, #63850, #86042, #56741, #78958, #41065, #64788, #92682, #42972, #71877, #20734, #28771, #34008, #91748, #349, #7447, #30158, #8825, #88826, #74168, #44353, #81267, #30620, #29236, #66160, #9284, #66610, #58131, #36329, #87429, #45264, #59041, #65243, #72326, #87888, #8375, #38167, #23041, #1733, #86976, #51919, #67082, #22130, #22576, #2216, #59987, #37255, #1276, #50998, #73715, #59522, #37705, #7904, #16412, #43883, #15482, #79883, #15023, #58590, #88371, #72779, #36794, #31100, #23521, #23975, #65714, #826, #51450, #52849, #80809, #29707, #14575, #43431, #80340, #73263, #15958, #44813, #52390, #9770, #75113, #82663, #74644, #26314, #68946, #3606, #17812, #4076, #90672, #38646, #24436, #68471, #60910, #31557, #33408, #10223, #2678, #83122, #67549, #17357, #39090, #18273, #46665, #46208, #47610, #76513, #47127, #75569, #4531, #82202, #68003, #90222, #60449, #10691, #3132, #76040, #25371, #89284, #53795, #61839, #54252, #32012, #11169, #53318, #62307, #89757, #40029, #32493, #54711, #24918, #39548, #40482, #32947, #16875, #91147, #61390, #25832, #83588, #45733, #18752, #11636, #69399, #81726, #27255, #92562, #78387, #20627, #19212, #5951, #28204, #20148, #93505, #55209, #56141, #19672, #69871, #84063, #12586, #84994, #49031, #27732, #41433, #77927, #64217, #34823, #56629, #12104, #42376, #85932, #91634, #13070, #48541, #6415, #85480, #48071, #62799, #76974, #13527, #42853, #40949, #34363, #26788, #63736, #92099, #41906, #5009, #21082, #71288, #35765, #70819, #35290, #33892, #93047, #57092, #49953, #78845, #13991, #70365, #71769, #6891, #64679, #55674, #63268, #84525, #77441, #5490, #66058, #51344, #239, #21545, #36218, #29601, #43774, #73145, #7338, #72676, #86871, #58934, #15850, #38055, #23417, #8271, #52282, #29120, #58480, #58016, #44708, #74057, #22026, #9177, #22935, #30509, #14920, #50428, #7795, #80237, #50895, #37151, #59405, #88258, #8719, #79778, #73609, #37597, #87324, #66507, #81162, #66964, #15374, #44236, #28661, #36680, #30053, #65602, #51805, #80697, #72223, #57548, #1627, #86393, #65138, #716, #79333, #14469, #43326, #1171, #22472, #87785, #16306, #45158, #59881, #17242, #52735, #23869, #75462, #32842, #88721, #10121, #61732, #47499, #89639, #82562, #81617, #61284, #83016, #25270, #89177, #3968, #31451, #3023, #16766, #67445, #46104, #90118, #45620, #2572, #90564, #18168, #83477, #60340, #24329, #75009, #18633, #53695, #53206, #25722, #54606, #40377, #74522, #38987, #76408, #11530, #9656, #82084, #31909, #38542, #2102, #47021, #17710, #60801, #75923, #11049, #67900, #24809, #46563, #10583, #39446, #30994, #68362, #3490, #32383, #54147, #39919, #68840, #70713, #5389, #33778, #35177, #64099, #34716, #63160, #85825, #69763, #4894, #77814, #55092, #70254, #62691, #63630, #12963, #91029, #41317, #49392, #41802, #91524, #5844, #11995, #20976, #77336, #92455, #56029, #42267, #55570, #19110, #28100, #27618, #4423, #13883, #20035, #76869, #56515, #33301, #26680, #34254, #78284, #69294, #91991, #85374, #84884, #20524, #49843, #92939, #27144, #71180, #13422, #83961, #48912, #56987, #6309, #47965, #62199, #48432, #26198, #40844, #84418, #19566, #12470, #93401, #21438, #28553, #86285, #57444, #35661, #50312, #79217, #42736, #71651, #6784, #64576, #68931, #74628, #3115, #2663, #83107, #39533, #67065, #45715, #59972, #10678, #25817, #76497, #17342, #9756, #46652, #75098, #10207, #31084, #4062, #75554, #18734, #60891, #32479, #2200, #31998, #18259, #67989, #89742, #32932, #53301, #68455, #3590, #24903, #52832, #46193, #61376, #88810, #47112, #90209, #53783, #38630, #23957, #67533, #39076, #82187, #82650, #16859, #17799, #31542, #25358, #54238, #47595, #61824, #76020, #90656, #60430, #11153, #89270, #40014, #83572, #24420, #38148, #54697, #81710, #91619, #4516, #26774, #63254, #40937, #84981, #42362, #71275, #85467, #4992, #56616, #20614, #41419, #49484, #6402, #49938, #92085, #27240, #11621, #69857, #13057, #19658, #34811, #63724, #55193, #40466, #92549, #69384, #19197, #55659, #33393, #62292, #91129, #49018, #26300, #84512, #33878, #35275, #48057, #48527, #76961, #27717, #70804, #12089, #56128, #78374, #70351, #62786, #77428, #12569, #5477, #34347, #20133, #77915, #41893, #5939, #85918, #64204, #13513, #93034, #28190, #57079, #21069, #35203, #63656, #77840, #64132, #57013, #40871, #84443, #92479, #27170, #91550, #93426, #70281, #62720, #49418, #33807, #77361, #5414, #78308, #12988, #12495, #13908, #42761, #13447, #41826, #64601, #48461, #41348, #56545, #26707, #48941, #34279, #42297, #85400, #69789, #20059, #28124, #20548, #63187, #71207, #19592, #28578, #56058, #6334, #27644, #21002, #92017, #55595, #6812, #92966, #76894, #57469, #85849, #84912, #49868, #12023, #70737, #5871, #78767, #86311, #71681, #35686, #47990, #4920, #2007, #81075, #51260, #88162, #37510, #36136, #73053, #16219, #73524, #7259, #14386, #631, #52193, #65975, #72143, #79244, #1086, #15291, #45070, #37066, #8633, #43245, #29967, #73970, #65054, #29516, #9086, #66871, #44148, #8184, #156, #80604, #66420, #44622, #14840, #23322, #50814, #22388, #29036, #86782, #65511, #15762, #57924, #21941, #37964, #1538, #30901, #79698, #43693, #58396, #59792, #58852, #72591, #21463, #50337, #7712, #36596, #87242, #80152, #87697, #22849, #51715, #30422, #59313, #33212, #75833, #10487, #24715, #10956, #3877, #81525, #31361, #75374, #67808, #38447, #40290, #17147, #9559 ),
 ( #61190, #60250, #11439, #2933, #18077, #39355, #61643, #74918, #67354, #47402, #90027, #23781, #4335, #68272, #2484, #25179, #52645, #89087, #89549, #32755, #88633, #60710, #32283, #3394, #82923, #69206, #54516, #53600, #90476, #39823, #24237, #46470, #83386, #46930, #74429, #16673, #31818, #25633, #54053, #45528, #53113, #68747, #82472, #18536, #76313, #81993, #46014, #10029, #38899, #17619, #70159, #92846, #13796, #55938, #48815, #26103, #27527, #49299, #85280, #55476, #64008, #91434, #63067, #83868, #33682, #12374, #56420, #54995, #62590, #28010, #78194, #49761, #26586, #84325, #41221, #78656, #19943, #19475, #85742, #20888, #6700, #40753, #5295, #19020, #12871, #84793, #56902, #77720, #20430, #47874, #41710, #42648, #76777, #34165, #71565, #62107, #70627, #5753, #11904, #13332, #42174, #71087, #48342, #90939, #77243, #91896, #69670, #27051, #34628, #6220, #4802, #63539, #92365, #35089, #23210, #49, #64948, #79594, #52090, #87135, #7156, #59207, #88053, #73868, #14275, #14735, #16117, #1433, #57361, #28929, #36489, #28467, #35574, #22735, #51157, #65406, #51608, #44514, #86203, #72040, #22286, #43589, #79128, #80973, #57816, #50224, #36959, #21353, #86667, #21831, #65872, #517, #50706, #30317, #44968, #981, #29400, #64490, #36030, #72486, #44043, #43135, #58292, #7602, #29862, #72945, #80044, #15184, #15645, #8070, #58746, #87589, #80497, #93316, #73419, #8529, #37408, #66317, #88985, #52546, #61543, #75270, #37865, #18429, #53492, #16571, #10386, #66769, #9451, #9928, #17972, #47287, #74813, #46368, #24604, #3287, #83284, #68638, #38802, #75727, #25079, #23681, #60608, #3770, #61081, #88533, #1901, #81886, #39714, #82368, #59690, #67706, #46825, #17518, #39252, #81421, #89923, #32655, #45426, #2834, #67250, #53953, #68167, #30791, #74326, #38337, #32180, #90376, #8986, #17041, #2381, #82820, #45907, #31717, #31260, #25531, #10849, #60147, #89444, #54412, #24133, #53011, #27417, #12268, #34058, #70979, #91319, #12760, #48705, #70042, #90833, #55370, #77609, #11334, #56305, #19837, #5184, #47769, #69105, #83758, #77137, #26480, #26945, #54879, #84222, #40645, #41601, #63431, #85635, #6112, #55833, #34983, #76668, #41110, #11795, #92260, #27905, #69565, #56793, #70523, #78087, #62478, #4231, #19369, #62960, #4693, #84688, #13230, #42065, #85171, #33568, #20322, #49192, #91794, #63897, #92733, #20782, #5649, #34524, #76205, #48234, #40186, #33109, #61998, #25993, #18914, #49654, #36848, #13686, #93208, #93664, #71449, #6586, #87937, #87026, #64383, #28824, #43027, #73311, #42538, #64839, #35464, #72828, #15069, #28360, #398, #22624, #14625, #78548, #57252, #50596, #14163, #86094, #21244, #7052, #79490, #21721, #22177, #35921, #50113, #71930, #51045, #57707, #7953, #65765, #79008, #86550, #875, #43483, #72379, #7496, #36381, #65294, #29288, #79933, #58184, #43931, #29754, #8422, #58635, #87476, #51498, #80386, #15528, #44403, #37301, #66207, #1323, #30205, #59096, #24023, #81314, #37752, #51970, #74217, #52897, #88874, #89333, #9336, #81776, #32065, #67599, #60496, #73762, #10274, #53848, #59573, #16926, #16460, #68054, #24488, #80860, #30670, #44859, #53368, #10743, #61442, #2268, #88423, #31607, #60037, #45785, #16007, #82714, #82254, #3660, #74697, #17409, #8874, #9819, #3181, #38692, #2727, #17865, #38219, #46257, #75161, #39143, #66660, #31151, #60960, #1787, #89812, #24974, #46717, #23572, #52439, #45312, #75619, #67134, #39600, #68523, #32549, #23088, #26835, #77493, #5999, #85051, #69922, #20200, #61889, #91201, #90721, #12638, #41955, #25882, #70868, #84575, #92149, #76563, #83174, #11686, #48122, #54763, #5062, #27304, #56192, #70415, #83640, #41485, #5540, #26370, #34411, #49079, #34872, #77026, #12154, #55259, #63318, #77978, #18324, #32998, #40999, #69452, #40079, #90272, #18804, #11224, #91684, #76090, #47662, #40537, #55723, #84114, #4582, #13119, #25423, #19723, #19264, #54301, #33457, #62360, #33945, #68996, #62850, #48593, #47180, #4127, #85527, #35809, #43821, #72267, #64268, #36266, #6467, #80283, #71816, #86919, #50476, #36730, #49998, #13575, #22521, #65186, #92615, #73197, #14516, #71337, #289, #27785, #93097, #64723, #72720, #8317, #93550, #7385, #79379, #58065, #44290, #29649, #28708, #65650, #79824, #78439, #21596, #58528, #22072, #49544, #56679, #42902, #764, #43371, #20673, #42425, #29170, #57593, #87373, #50942, #14965, #35344, #7843, #51392, #28251, #6936, #15422, #63785, #86437, #57139, #85980, #21130, #78893, #14040, #30102, #15901, #1218, #58984, #37199, #87832, #22983, #80749, #66107, #44758, #51857, #73658, #20305, #90817, #61982, #76652, #49176, #84206, #4216, #56289, #85152, #70963, #11320, #11777, #13213, #92244, #54397, #25976, #33551, #25518, #32640, #19821, #48215, #19353, #27399, #84670, #18414, #83270, #40629, #63415, #77119, #47274, #90361, #12248, #26465, #78070, #41094, #48687, #76190, #70022, #42049, #40171, #69547, #61530, #69088, #55354, #5165, #33091, #91777, #77591, #55816, #54860, #34508, #83742, #62459, #18899, #47754, #4677, #26928, #91302, #34040, #62943, #12742, #41584, #70506, #5633, #51374, #23898, #58966, #72702, #31023, #59910, #45650, #79806, #80265, #81648, #66997, #29150, #745, #8298, #268, #7365, #88290, #22962, #37180, #23445, #16337, #58047, #43802, #87813, #15401, #50922, #52769, #29629, #22053, #8750, #86898, #36711, #58508, #37629, #66087, #65632, #2134, #88752, #66538, #1200, #16796, #7821, #87353, #15882, #14948, #30082, #22503, #1658, #44738, #44268, #73179, #81190, #73640, #51836, #30537, #80729, #36246, #59439, #52313, #45186, #74089, #9208, #38086, #65164, #47049, #9689, #83988, #25297, #82119, #75950, #38571, #75037, #75490, #83504, #19135, #46591, #18197, #90149, #68865, #55123, #40403, #10614, #47530, #90591, #89209, #89673, #54175, #53236, #24841, #39016, #11082, #61758, #74560, #69321, #83045, #4449, #46134, #39472, #10150, #25751, #26229, #67931, #67473, #3995, #76434, #60828, #2602, #53724, #32412, #3054, #39949, #11555, #33328, #54632, #31939, #18663, #62225, #68390, #91054, #31482, #60370, #61311, #32870, #24360, #82590, #17277, #17737, #3521, #91659, #83146, #39574, #26812, #3631, #18297, #83615, #61415, #90247, #77950, #77000, #54276, #18776, #32971, #63291, #32520, #54737, #25396, #62825, #5036, #47155, #84089, #12611, #4557, #68496, #76064, #40507, #4100, #11193, #40053, #90695, #69426, #11660, #12129, #25855, #33431, #48565, #19239, #40975, #68970, #55698, #70388, #61864, #62335, #47634, #84549, #69897, #76538, #91175, #26341, #33916, #27278, #55234, #48096, #19696, #77468, #41456, #5516, #34386, #92124, #56165, #20174, #85022, #49054, #41931, #71789, #58041, #42876, #64699, #7816, #28226, #43347, #79354, #6911, #27758, #85954, #14489, #70842, #86893, #50452, #35786, #78412, #5975, #20650, #14016, #262, #28684, #93525, #29145, #22047, #34848, #49520, #57570, #21106, #56654, #58502, #35316, #85503, #72244, #92589, #42400, #64241, #7359, #86413, #71311, #72697, #36706, #36241, #21569, #29624, #13551, #6441, #65159, #93072, #50916, #57114, #79800, #14942, #63759, #78866, #43797, #65627, #49974, #739, #87347, #22496, #51369, #13093, #66991, #53230, #66533, #30075, #39011, #52762, #15396, #89667, #31018, #87808, #81643, #44263, #80724, #81185, #89203, #24836 ),
 ( #8293, #59905, #17271, #73174, #88285, #46129, #31933, #74083, #2129, #37174, #45644, #67468, #9684, #73634, #82112, #15877, #16331, #66082, #51831, #30532, #74553, #1194, #44733, #75032, #2597, #67925, #8745, #37622, #59434, #3049, #38080, #1652, #10145, #60824, #80260, #58960, #23440, #22957, #52308, #45181, #9202, #88747, #23893, #16790, #38566, #31477, #60365, #24355, #54171, #83040, #62221, #39469, #54628, #18193, #19131, #91050, #75486, #25747, #33802, #26224, #47045, #55118, #90143, #70277, #61754, #76889, #40398, #26702, #39945, #3517, #12491, #83983, #82586, #63182, #4444, #61307, #47986, #17733, #75946, #83500, #62716, #92013, #18658, #12017, #69316, #40867, #34275, #19587, #47525, #55591, #69785, #68386, #11551, #48456, #4916, #32409, #46588, #32865, #84439, #33324, #10611, #25293, #91546, #76430, #77357, #41343, #5410, #11076, #53719, #68861, #3990, #90586, #57918, #72585, #20998, #13904, #84907, #86307, #14381, #50332, #20544, #29031, #56539, #28120, #48936, #92474, #71203, #21459, #20055, #27640, #86775, #43241, #14835, #85396, #49414, #6330, #43688, #78762, #78304, #50808, #79693, #65505, #5866, #35198, #7707, #21936, #77836, #13443, #57009, #12984, #27165, #72139, #42757, #85845, #7255, #36131, #41822, #63652, #71674, #64126, #70733, #36591, #42291, #34736, #28574, #92961, #49863, #6808, #57464, #35682, #64597, #56053, #93422, #79239, #65048, #151, #80146, #624, #51255, #8177, #15286, #87236, #44143, #22383, #29510, #73047, #37061, #58391, #62806, #76047, #39556, #48548, #62316, #24928, #5496, #40490, #3614, #91156, #53805, #90230, #90679, #5018, #34369, #61848, #33415, #11643, #84070, #70371, #55681, #25839, #91641, #12112, #10699, #47617, #84532, #48078, #75578, #82673, #68953, #26795, #69408, #46675, #17822, #4539, #83596, #19679, #26321, #76983, #68478, #55216, #77449, #32501, #4084, #12593, #41439, #18759, #76520, #61398, #19220, #40957, #69879, #83129, #89766, #25379, #54720, #54259, #18280, #40037, #33899, #47136, #11177, #32955, #50436, #50900, #27740, #92570, #13534, #79784, #21089, #34831, #86877, #22031, #7800, #41912, #42382, #43780, #29127, #85003, #56636, #64224, #56148, #63274, #79339, #78850, #93054, #14474, #72229, #20157, #5957, #49959, #71295, #13076, #14926, #85486, #77933, #64684, #49037, #20633, #49503, #93510, #28210, #78393, #58023, #72681, #28667, #57098, #92107, #63742, #6423, #71774, #14000, #36224, #35298, #70825, #27261, #35771, #85938, #42860, #6897, #57553, #86398, #21552, #43332, #7343, #65143, #244, #8727, #74065, #52289, #31001, #18514, #2579, #66515, #9665, #52743, #51351, #88267, #31458, #88727, #22478, #29607, #15856, #67451, #81168, #87330, #721, #16312, #30516, #60347, #45164, #23875, #58485, #9185, #89184, #80242, #44715, #24337, #83364, #59413, #23423, #15379, #2111, #81624, #59887, #30058, #38548, #66065, #37603, #44243, #8276, #80706, #16772, #73153, #37156, #53212, #45626, #47378, #1177, #58942, #73615, #76292, #38063, #87791, #36687, #65609, #22940, #51813, #1635, #66972, #74533, #90916, #91410, #63046, #76755, #40269, #56399, #27031, #91877, #71068, #6200, #19455, #55920, #84772, #19921, #12850, #63518, #36008, #93295, #80022, #64468, #14255, #64926, #15162, #14715, #43113, #44493, #8507, #44021, #72464, #1408, #79106, #28907, #51139, #28446, #79572, #50686, #72918, #8046, #6678, #43568, #58723, #36939, #29379, #65853, #21332, #30295, #58273, #961, #29840, #87567, #37386, #35555, #22712, #57339, #51586, #80472, #86181, #15622, #66296, #59183, #23185, #78635, #50202, #16547, #66747, #80949, #9426, #81864, #24109, #24575, #38314, #17013, #61057, #2810, #89421, #8962, #39226, #82797, #88510, #45882, #45403, #3265, #53464, #16094, #59667, #73846, #82344, #39687, #90351, #31237, #23657, #60586, #88962, #52990, #44946, #17949, #17492, #32630, #74789, #46344, #37841, #9905, #32155, #38779, #67683, #46800, #67228, #75246, #10361, #31691, #1873, #60123, #68144, #30766, #89899, #25057, #53929, #52523, #81399, #74302, #75703, #2359, #10827, #68612, #3748, #61520, #52067, #12732, #34959, #20295, #5154, #49168, #90808, #26456, #25967, #41574, #70953, #54848, #6085, #19811, #27390, #11768, #18405, #40620, #77108, #83731, #34030, #56280, #85140, #5624, #18890, #70496, #34499, #55345, #63405, #78061, #63871, #12239, #41086, #25507, #47745, #26920, #33542, #48679, #77581, #69079, #54385, #92234, #83261, #4207, #69536, #47264, #76179, #11311, #62934, #40162, #13203, #55807, #33082, #61971, #76643, #91768, #42039, #4669, #62448, #91291, #84659, #84197, #19344, #48206, #70011, #36352, #73285, #21689, #87000, #27875, #57681, #43905, #28794, #50566, #87452, #14134, #29259, #65266, #86524, #13660, #71904, #372, #56768, #72802, #58154, #79463, #64357, #85610, #6557, #93637, #42999, #43454, #71424, #7024, #57225, #22152, #79907, #8398, #22598, #72352, #51473, #93183, #14597, #28335, #15045, #44375, #86066, #37276, #51020, #849, #78981, #20756, #35895, #7469, #21216, #7926, #29730, #58611, #36818, #50086, #65739, #80362, #15503, #92706, #49627, #78523, #42512, #35436, #64813, #30646, #67574, #74192, #89308, #24464, #15983, #66182, #53343, #30181, #44835, #16437, #87913, #23064, #10717, #9794, #80832, #45289, #59546, #89782, #59066, #81291, #51942, #82228, #31584, #73738, #16902, #39118, #31126, #1299, #8850, #67107, #88396, #37728, #66634, #23546, #2241, #38193, #38669, #52416, #60011, #75138, #45761, #2702, #1759, #17382, #3157, #9311, #88851, #24000, #52873, #46234, #81752, #68030, #74670, #60473, #24945, #10249, #32040, #75594, #60935, #53822, #82690, #17840, #46692, #53803, #61846, #62312, #24926, #90228, #68476, #47132, #33413, #18757, #82671, #25837, #68951, #67556, #10697, #47615, #11174, #38652, #45741, #32019, #83594, #3612, #9777, #16882, #32498, #46673, #76518, #61396, #40035, #74652, #25377, #11641, #2685, #60918, #40488, #4537, #75576, #39553, #31565, #18278, #4082, #76045, #46216, #54716, #82210, #17819, #60456, #24444, #3139, #32953, #89291, #53325, #69406, #90677, #91153, #17365, #75120, #89764, #52856, #54257, #10230, #81734, #39098, #68010, #83127, #70369, #8155, #85936, #48076, #19677, #27259, #19218, #65952, #13532, #41910, #56146, #42380, #35295, #76981, #62804, #13074, #5494, #69876, #73027, #48546, #40955, #27738, #12110, #55679, #77446, #56634, #84999, #84530, #21087, #49957, #85484, #20154, #44123, #26793, #12591, #34829, #5015, #49035, #41437, #20631, #63740, #33897, #92105, #6419, #92566, #34367, #49501, #91639, #37038, #26319, #78391, #63272, #77931, #70823, #13996, #84068, #5955, #71293, #64222, #93052, #28208, #57096, #55214, #59768, #39330, #1063, #1983, #59290, #15733, #29942, #52167, #30874, #66848, #67329, #81050, #88609, #10005, #45503, #38420, #51691, #81967, #31793, #37486, #23757, #88136, #45989, #2461, #58827, #8610, #22822, #31337, #82449, #87672, #73946, #66396, #9535, #37939, #52620, #80580, #60687, #60224, #75349, #81502, #89063, #44594, #16649, #74894, #74405, #24213, #89527, #16193, #53088, #17123, #38876, #73498, #9061, #67783, #1512, #2909, #24691, #53574, #30398, #23294, #45045, #17597, #46447, #10464, #46906, #83360, #32732, #4775, #55451, #77697, #63042, #47849, #91873, #39799, #69182, #68721, #84302, #19917, #3851, #48789, #62566, #70134, #54492, #61166 ),
 ( #32260, #18054, #18510, #90002, #25157, #61620, #25609, #69647, #4311, #90452, #34139, #27027, #33657, #62079, #84768, #47374, #76288, #76751, #54031, #33189, #11414, #91407, #11879, #82898, #40265, #48318, #40730, #90912, #26562, #10931, #12846, #26078, #19452, #54967, #41196, #83843, #75807, #55916, #77219, #3372, #68248, #18996, #12347, #5270, #5729, #42146, #42622, #50683, #51136, #13773, #79102, #57335, #36004, #22262, #7580, #71541, #14712, #57792, #56395, #93291, #36465, #25, #27497, #34604, #20863, #72461, #86177, #92342, #63514, #21328, #35551, #65380, #50198, #28904, #85257, #14251, #492, #20405, #49734, #29376, #87112, #64464, #28442, #49275, #7133, #86642, #64922, #35063, #43565, #71064, #6674, #78170, #13308, #85718, #21809, #6196, #63983, #58270, #79569, #80019, #92823, #27986, #78631, #41684, #43109, #56877, #70602, #72016, #53460, #87564, #59180, #89418, #74785, #36936, #8504, #16091, #8042, #15159, #2356, #30762, #44943, #31234, #24106, #65850, #51583, #1870, #88024, #58720, #60583, #37383, #29837, #16544, #958, #73843, #73394, #9902, #38776, #74299, #8959, #31688, #15618, #44490, #23654, #22709, #37838, #66293, #9423, #52520, #80469, #80946, #88959, #81396, #1405, #45400, #30292, #24572, #23181, #38310, #59664, #81861, #52064, #66744, #67680, #67225, #44018, #72915, #88507, #60120, #52987, #17010, #45879, #2806, #61053, #25054, #10358, #3262, #68141, #32152, #82341, #17489, #89896, #46341, #75243, #39223, #35643, #43655, #36095, #63614, #70697, #56971, #14799, #28537, #34700, #41786, #57428, #71636, #72550, #93384, #65015, #5828, #86269, #7672, #92438, #85809, #36555, #29471, #6768, #64560, #27602, #43203, #115, #7221, #71163, #79658, #13407, #78724, #56499, #49375, #28083, #72104, #85358, #78268, #65471, #28996, #588, #42250, #6291, #20959, #58359, #21420, #35161, #87199, #22347, #77798, #20506, #49827, #12948, #64083, #92922, #13865, #42719, #50295, #79201, #86738, #14344, #21900, #50773, #60208, #44107, #87655, #37924, #30381, #1048, #2894, #73482, #65937, #52605, #37023, #80564, #8594, #81487, #9516, #29927, #73011, #59274, #81949, #1967, #8140, #15248, #30859, #45030, #17106, #66829, #38404, #58812, #59753, #45972, #22806, #88120, #74878, #31777, #73930, #88593, #51674, #16634, #67313, #74388, #44579, #53073, #15718, #52152, #37471, #66381, #1497, #45488, #23277, #81034, #9988, #2443, #38861, #16178, #9046, #23742, #67767, #31321, #89047, #60671, #89508, #51219, #24196, #80109, #5255, #84287, #46430, #18039, #25593, #17581, #63028, #11862, #40250, #54476, #40712, #33640, #75333, #61151, #11398, #3836, #68232, #70117, #46891, #39315, #26060, #10449, #54016, #75792, #54949, #83345, #82883, #19437, #48302, #83827, #18492, #41177, #25140, #10914, #33172, #3353, #47356, #39782, #18981, #62062, #32243, #90436, #4759, #90896, #68706, #47833, #89986, #34124, #32718, #76735, #69166, #91392, #61603, #76272, #77202, #69631, #53559, #24673, #4293, #62549, #26547, #82431, #55435, #12332, #7119, #7566, #63965, #35536, #13760, #86162, #72447, #57778, #27972, #64908, #14236, #12832, #49720, #86624, #50186, #41670, #91859, #79084, #55901, #70588, #42132, #19902, #48774, #36451, #64450, #5715, #71049, #85242, #21794, #84754, #13294, #77680, #21314, #57321, #34590, #42608, #10, #56862, #27013, #63498, #92806, #56376, #92328, #27484, #49261, #85704, #20849, #93276, #78156, #78616, #35988, #71524, #28428, #20390, #43095, #28889, #6182, #6658, #35049, #72000, #50669, #79555, #14696, #43551, #37825, #52973, #9889, #44475, #72902, #73832, #8491, #37369, #58255, #31222, #8946, #45865, #88012, #59650, #475, #30276, #16532, #1392, #23166, #60107, #80456, #1858, #66731, #59166, #80004, #73381, #30748, #29363, #45385, #88495, #52049, #36922, #87098, #8026, #66279, #15603, #16078, #44004, #80933, #29823, #23642, #52508, #74771, #88947, #44931, #24094, #65837, #81384, #945, #74286, #16998, #58705, #65366, #9410, #67210, #51570, #22248, #38296, #2343, #87548, #81848, #51118, #15143, #22695, #32141, #83715, #47732, #68597, #18876, #33528, #77095, #90339, #54372, #38764, #3251, #40149, #46786, #61959, #25494, #83247, #67668, #61039, #69065, #75688, #90795, #25954, #82328, #2794, #54835, #31676, #17478, #82783, #60570, #89406, #24560, #76163, #53446, #17935, #89883, #62434, #46329, #53915, #75232, #76631, #4194, #10346, #18393, #11755, #3733, #39212, #68127, #39675, #25043, #10813, #32617, #61507, #47250, #11296, #33069, #40607, #69523, #4654, #91275, #26441, #55332, #84183, #19331, #48193, #70938, #70481, #57207, #13644, #41072, #19797, #34016, #78506, #93619, #50548, #85125, #48666, #20740, #49151, #78047, #5137, #71884, #49611, #86508, #34942, #6541, #69997, #6069, #86048, #42023, #63856, #7006, #27375, #42495, #71409, #92689, #26906, #20276, #35418, #62919, #21197, #64339, #27859, #77567, #91754, #12716, #13188, #56265, #56750, #84646, #85593, #5609, #93166, #28318, #21671, #35878, #50068, #64795, #41558, #78964, #34484, #14115, #57661, #63390, #12225, #42978, #28777, #92220, #55794, #65720, #37261, #15030, #59048, #16420, #45272, #59529, #72785, #30628, #88378, #15488, #23528, #74175, #23983, #9292, #37712, #65249, #72334, #58596, #38175, #30165, #36335, #43438, #87895, #73269, #67090, #1283, #66618, #7453, #23048, #2223, #355, #87437, #31107, #59994, #8381, #66167, #29242, #44819, #1741, #8834, #7910, #81274, #43889, #80346, #58137, #51004, #29714, #73722, #86983, #79891, #88833, #52397, #79445, #36800, #832, #22583, #14581, #51926, #51457, #22136, #44359, #80816, #15965, #26278, #56596, #41876, #4045, #69367, #76944, #68914, #20598, #63237, #91601, #12071, #92068, #84963, #32915, #18713, #62769, #55173, #25800, #27698, #4497, #90637, #77410, #61805, #11604, #33375, #12548, #40919, #40449, #70787, #5922, #41398, #69839, #92532, #76481, #62274, #84495, #54680, #4973, #91109, #70332, #19641, #83554, #48039, #56110, #48509, #84034, #5461, #47576, #85450, #19179, #34331, #26757, #48996, #33859, #55642, #34792, #27222, #11131, #76000, #20114, #77895, #13039, #39995, #63707, #50395, #58452, #58907, #21517, #86838, #65109, #43746, #30024, #15347, #79300, #22442, #65573, #64184, #7311, #93016, #93479, #42821, #73114, #13498, #64650, #6387, #72646, #14892, #71259, #212, #51315, #14440, #87753, #49468, #43297, #13963, #28174, #78358, #6862, #72194, #36190, #21996, #35737, #29092, #87296, #57985, #50868, #35258, #36652, #80207, #85902, #79750, #71736, #687, #7768, #57064, #21054, #49921, #29571, #37121, #78818, #28632, #57521, #44207, #86366, #8241, #66030, #1143, #60312, #3458, #45589, #17212, #51777, #81586, #67871, #52705, #74492, #17681, #38024, #53176, #89150, #16734, #37570, #2071, #24299, #80666, #2994, #82055, #9624, #88227, #15822, #30480, #23839, #66933, #67415, #1597, #30962, #81133, #46073, #10091, #32353, #46533, #2544, #75435, #23383, #38511, #52252, #38959, #68335, #16277, #61252, #74979, #24781, #9146, #44679, #59850, #31423, #45128, #31880, #53663, #82532, #60770, #74029, #89610, #10553, #39418, #22906, #73581, #8690, #66480, #59375, #88691, #54575, #91491, #4394, #19534, #48400, #39887, #90088, #77303, #54114, #68808, #40348, #18137, #46991, #34683, #33745, #3937, #69265, #70679, #55995, #75893, #83446, #90999, #82987, #25240 ),
 ( #90533, #25693, #4862, #11017, #26168, #18601, #55536, #62657, #32811, #62168, #70220, #26646, #47466, #84385, #61701, #12929, #33271, #12435, #76837, #63127, #76373, #11499, #48878, #41285, #55059, #5809, #40812, #83928, #5355, #19080, #47934, #11964, #34221, #69729, #91956, #27111, #84850, #20000, #77781, #41769, #93367, #36539, #79642, #78249, #21402, #29455, #21886, #49355, #56480, #42702, #571, #14327, #20489, #27583, #43187, #57411, #58343, #79183, #50758, #85338, #72088, #87185, #13387, #71620, #22334, #15235, #86251, #50275, #42230, #28980, #14784, #86722, #56954, #65454, #92905, #64541, #71144, #35142, #13849, #57866, #6273, #64065, #51205, #43637, #80093, #28065, #85791, #6753, #44091, #7205, #20942, #72996, #8125, #63597, #72535, #36080, #92421, #49810, #78707, #64998, #35626, #28517, #101, #7654, #45476, #58797, #9034, #17091, #74375, #37457, #9501, #73467, #53546, #45016, #60195, #23729, #9976, #23262, #80546, #89495, #38389, #65923, #46418, #81473, #44564, #67301, #1035, #66366, #37912, #45959, #75319, #66816, #2429, #52592, #31309, #17567, #2881, #1949, #38847, #53061, #51659, #88581, #31766, #89033, #22790, #29913, #16164, #67755, #16621, #87641, #15703, #24182, #30846, #60658, #81936, #74864, #8579, #24658, #82419, #1483, #73917, #37010, #30367, #59739, #59256, #88104, #52140, #81020, #33624, #3823, #12318, #39767, #11385, #32230, #75780, #54461, #69615, #68219, #10900, #70099, #91374, #91844, #68692, #32704, #83332, #26999, #62049, #61590, #34111, #63013, #48759, #82871, #18478, #84740, #5240, #61138, #90422, #40237, #3339, #10436, #26532, #26046, #69152, #55420, #19424, #89974, #46877, #90883, #47340, #54002, #55887, #25579, #25128, #11846, #18024, #76257, #4280, #40696, #33158, #54932, #19888, #39301, #83812, #18965, #47818, #62533, #76720, #4744, #84273, #41162, #48286, #77189, #41656, #28412, #71505, #14678, #93258, #35971, #5698, #57303, #43534, #70573, #85686, #72431, #29342, #6638, #64432, #34573, #43077, #64891, #7100, #71031, #79539, #13278, #78598, #63482, #49245, #27955, #71981, #92312, #78140, #7548, #77959, #65348, #42115, #6164, #56845, #455, #35518, #35034, #36432, #58235, #22228, #56359, #20833, #87079, #77664, #27467, #63948, #13740, #85223, #12816, #28871, #86145, #42590, #57759, #86605, #20374, #92787, #21295, #49702, #50168, #79065, #14217, #21775, #50651, #36899, #80438, #8472, #52489, #80913, #15583, #16979, #45844, #16514, #44911, #67649, #51549, #44454, #59628, #65815, #52028, #73360, #45365, #88475, #72882, #23145, #31203, #23622, #37352, #81364, #87529, #2775, #59147, #74268, #37805, #24075, #66259, #925, #9869, #9391, #79985, #60547, #1840, #58686, #38275, #15122, #1374, #16058, #60088, #89385, #73814, #67188, #66711, #2322, #31656, #74749, #8927, #52951, #88927, #22677, #38744, #51098, #43984, #29805, #30256, #8007, #87992, #30727, #81828, #25474, #17458, #62897, #11736, #40129, #54353, #40589, #33508, #46308, #61018, #11276, #3713, #68106, #69976, #46767, #39194, #25933, #10327, #53896, #75668, #54816, #83227, #82764, #84163, #19311, #83694, #18372, #41049, #25024, #17916, #33048, #3231, #47231, #10792, #18855, #61938, #75212, #90320, #4634, #90774, #39653, #47713, #89864, #5116, #32598, #76613, #69046, #91256, #68576, #32122, #77074, #69503, #53424, #33994, #4175, #61488, #62414, #82308, #76142, #26420, #55310, #24540, #48173, #12205, #13621, #86027, #72311, #57639, #27837, #64773, #14091, #12695, #49589, #86483, #50045, #77545, #84626, #70915, #28756, #42474, #48644, #55773, #71385, #85572, #21648, #6518, #78941, #19774, #35396, #50526, #41535, #6048, #79424, #43416, #20719, #78485, #70461, #57186, #42956, #21176, #85103, #93598, #27354, #92665, #5588, #63368, #42001, #71862, #34460, #92198, #14559, #6983, #7432, #56241, #20253, #34920, #36312, #64316, #49129, #56726, #78025, #35856, #93141, #13165, #63833, #91733, #28296, #26886, #38969, #9156, #82997, #74504, #89621, #53188, #39427, #52716, #16287, #25250, #67881, #1606, #75905, #17222, #74039, #3004, #30491, #66943, #67426, #75444, #11030, #38522, #10102, #82066, #60781, #47002, #32363, #2554, #68344, #82541, #81143, #24309, #61264, #24789, #52263, #59386, #45602, #3471, #46084, #23397, #88238, #74991, #60322, #90099, #31890, #53674, #45138, #17692, #54126, #38036, #9634, #18148, #65228, #89160, #46542, #2083, #10563, #30973, #59861, #88702, #23850, #81597, #31433, #16747, #11511, #83938, #5366, #3950, #40358, #5820, #27123, #27596, #4404, #69275, #19091, #56493, #91501, #33283, #63608, #92432, #78262, #18613, #47945, #20500, #34694, #61712, #62178, #40822, #32822, #39898, #56006, #55546, #69741, #84862, #48891, #90546, #76385, #26657, #76847, #83458, #85352, #91010, #54586, #41296, #25704, #26179, #55069, #70231, #4873, #11974, #49368, #68820, #34232, #33756, #47477, #62668, #84396, #48411, #19545, #77314, #12448, #63138, #91967, #20013, #77792, #12941, #41780, #70690, #58355, #43199, #65010, #8135, #28531, #43650, #79654, #7217, #28078, #86264, #14795, #42243, #87195, #50769, #36090, #78719, #6285, #20954, #14340, #57424, #57878, #85803, #21415, #71632, #72546, #583, #22802, #37018, #86733, #65932, #13860, #72100, #42715, #29466, #58807, #6764, #87651, #7667, #15244, #93380, #35156, #50290, #111, #35638, #21896, #44101, #73007, #22343, #64556, #51214, #80105, #28990, #1044, #29923, #51669, #36550, #65466, #13399, #79197, #71156, #64077, #92916, #56966, #49822, #80559, #59268, #15713, #73477, #66376, #44574, #37467, #8589, #1493, #88116, #23273, #30377, #81630, #22037, #73160, #14932, #81173, #23428, #50906, #8733, #31006, #22946, #2584, #58029, #58949, #22484, #72687, #86883, #15385, #87797, #30064, #30520, #44250, #51820, #66978, #37609, #1640, #43787, #45169, #88733, #727, #80712, #51358, #9190, #59419, #79790, #65615, #7806, #88272, #45631, #36694, #37162, #29613, #66521, #66071, #52295, #58491, #38068, #16317, #15863, #87336, #80249, #8282, #44721, #1183, #74071, #73621, #2116, #59892, #23880, #52748, #67456, #16777, #74539, #9670, #38553, #32397, #31919, #47513, #76880, #60811, #12007, #25735, #33314, #17721, #24342, #46576, #83028, #89653, #11063, #62210, #91040, #11541, #24822, #76419, #40388, #61296, #69306, #26212, #69775, #18182, #47033, #60352, #53706, #32854, #39458, #54617, #83489, #75019, #89189, #18646, #53217, #10132, #75474, #82098, #17257, #46116, #68850, #38998, #10598, #82573, #55106, #67911, #68375, #3036, #4434, #90575, #3505, #75935, #83973, #90131, #25282, #54159, #39933, #3979, #61743, #19121, #47976, #40857, #70724, #71193, #56043, #34727, #13894, #49405, #42280, #55581, #85836, #35672, #41331, #63643, #63172, #49854, #6320, #33790, #12481, #26692, #35188, #86297, #43231, #77825, #70266, #13433, #41813, #5856, #91535, #64587, #64113, #79229, #27630, #92951, #62705, #92465, #78753, #56529, #85386, #93412, #20046, #28111, #56998, #20535, #19577, #78295, #28564, #84429, #12975, #57455, #50323, #20987, #42748, #48445, #71664, #6797, #21450, #92002, #14371, #34265, #4905, #77347, #5400, #48926, #27155, #84896, #73849, #39231, #60589, #61060, #37844, #8966, #23661, #89902, #31240, #44949, #3268, #32159, #17952, #52070, #52527, #53932, #68148, #1412, #66750, #74305, #66298, #73400, #89424, #88966, #9430, #24579, #82347 ),
 ( #38317, #1877, #53467, #25060, #30770, #82801, #67686, #75249, #59670, #30299, #88513, #60127, #81402, #52993, #10364, #8510, #17495, #16551, #46348, #37389, #67232, #59186, #88031, #23188, #24113, #81867, #80953, #45406, #74792, #2362, #2814, #31696, #16097, #17017, #45886, #9909, #38782, #90810, #68616, #3751, #85144, #84199, #61523, #25969, #40165, #70499, #10830, #61975, #32633, #70014, #12241, #39691, #91295, #19814, #11770, #90354, #54852, #69081, #5626, #25511, #83734, #54389, #5157, #41088, #83263, #26458, #48681, #40623, #46804, #75707, #47747, #11313, #18408, #47266, #4209, #76645, #18892, #19346, #33084, #69539, #55809, #55347, #48208, #76182, #34033, #77583, #4671, #33544, #62451, #91770, #77111, #62936, #26922, #84662, #12734, #34501, #41577, #63408, #92237, #27392, #56282, #86070, #13206, #79911, #57684, #852, #43003, #14600, #49170, #78984, #65270, #50090, #71907, #15048, #35440, #50570, #86527, #14138, #34961, #93186, #21693, #78063, #375, #79466, #7028, #85613, #42041, #27880, #21220, #64361, #64816, #92710, #28338, #78526, #43458, #7472, #29733, #43909, #93640, #72805, #20759, #35898, #49631, #36357, #65743, #13664, #58614, #72355, #22155, #6561, #70956, #57228, #28799, #42516, #29263, #51023, #7930, #58158, #71427, #87003, #36823, #20298, #6088, #63873, #56771, #45292, #9314, #87455, #51945, #88854, #1765, #16906, #45764, #37279, #22602, #74674, #51477, #66185, #37731, #15506, #44379, #32044, #31129, #44838, #24003, #23550, #80837, #53347, #82231, #52876, #81294, #10253, #87916, #23067, #2245, #73289, #88400, #15986, #81755, #60015, #8401, #59549, #67577, #9798, #73741, #38672, #30184, #39121, #30649, #2705, #74196, #60476, #8853, #1302, #46237, #31587, #80365, #3160, #38197, #59072, #89312, #66638, #52419, #16440, #24467, #67110, #17388, #75141, #68033, #55238, #41460, #26817, #90698, #33920, #77005, #75597, #18779, #55703, #19243, #46695, #53827, #40057, #91663, #11664, #17844, #24950, #40513, #54740, #84554, #76541, #48102, #82693, #69431, #19701, #10720, #68974, #48571, #12615, #83618, #47638, #39577, #26345, #12134, #84094, #54279, #62829, #90251, #61867, #68500, #32525, #11197, #40979, #3634, #61419, #77472, #69901, #70392, #25400, #83149, #4104, #5520, #4561, #18300, #60938, #89786, #47158, #76067, #32976, #25858, #33435, #62339, #91179, #5040, #27283, #72701, #21574, #49978, #64246, #50456, #43352, #56170, #70847, #21110, #13555, #77954, #79805, #56658, #49058, #35790, #20178, #63764, #86417, #85027, #14020, #65163, #92128, #42405, #267, #14947, #28230, #78871, #13097, #93530, #79359, #57574, #27763, #36245, #92594, #35321, #41935, #5980, #78417, #28688, #34852, #85507, #29149, #14494, #22052, #20654, #49524, #71315, #50921, #85959, #6446, #58046, #86897, #34390, #93076, #57118, #43801, #63297, #42881, #71794, #6916, #64703, #72248, #7364, #23444, #37628, #88751, #16795, #744, #44267, #88289, #80728, #51373, #53235, #30081, #22502, #9207, #87352, #37179, #58965, #38085, #66537, #66086, #67472, #2601, #66996, #1657, #24359, #8297, #1199, #16336, #80264, #8749, #87812, #2133, #45185, #29628, #73639, #81647, #74088, #22961, #31022, #73178, #82118, #15881, #59909, #52312, #74559, #51835, #15400, #60369, #23897, #36710, #17276, #81189, #44737, #52768, #65631, #30536, #59438, #45649, #46133, #9688, #38570, #31481, #89208, #7820, #58507, #31938, #53723, #24840, #10149, #60827, #82589, #17736, #39015, #75036, #89672, #67930, #3053, #27382, #34490, #21205, #64347, #7459, #86055, #6075, #71415, #92226, #42030, #20746, #35885, #63396, #70944, #36341, #57670, #58143, #34949, #63862, #49617, #86989, #28325, #92695, #362, #29248, #15035, #49158, #78513, #51010, #65256, #56271, #27865, #6547, #85131, #70487, #86515, #50076, #35425, #21678, #79451, #20283, #13194, #57214, #13650, #78053, #22142, #56757, #85599, #71892, #42502, #93173, #78971, #7013, #14122, #42986, #79897, #5616, #64802, #93626, #28784, #50554, #14587, #43444, #72340, #44825, #73276, #9300, #52405, #65727, #15972, #23990, #81281, #44365, #16427, #80353, #60463, #51932, #67097, #30636, #16891, #30171, #87443, #2692, #45279, #72792, #53332, #88385, #51464, #74182, #7916, #8388, #73728, #52863, #82218, #8840, #38182, #59535, #2231, #24453, #9784, #37718, #45748, #60001, #58602, #1748, #38659, #31114, #29720, #36807, #23054, #74660, #23535, #838, #22589, #88841, #66624, #67563, #81741, #31574, #15494, #89298, #43895, #37267, #80822, #66173, #1289, #59054, #87902, #75128, #76527, #4546, #40497, #10706, #19227, #54726, #32029, #61405, #39563, #40963, #10238, #32508, #68019, #69415, #11650, #39106, #61854, #84077, #76053, #55687, #17372, #18287, #75585, #60926, #46224, #68485, #47144, #83136, #83603, #3621, #11183, #26329, #90685, #18766, #3147, #33421, #48085, #53812, #40043, #90237, #62323, #47624, #89773, #24935, #82680, #91163, #5024, #17830, #25386, #46682, #25845, #54266, #68959, #4090, #76989, #55223, #91647, #32961, #12118, #69885, #33905, #62813, #26801, #42388, #79345, #5963, #21096, #57104, #78400, #5503, #63748, #85944, #19685, #64690, #28216, #13540, #56154, #77455, #92113, #85492, #34837, #35304, #63280, #92577, #49043, #49965, #71780, #251, #14480, #64230, #43338, #85010, #20639, #20163, #6902, #36231, #77938, #65149, #78856, #86404, #70831, #12599, #27746, #71300, #13082, #93060, #21558, #50442, #93516, #41919, #35777, #28674, #49509, #57560, #72235, #29134, #6429, #14006, #84538, #56642, #42866, #7349, #48554, #41445, #34375, #70377, #27267, #66257, #52024, #52486, #30254, #59145, #46764, #81361, #25021, #60085, #73811, #32119, #61015, #8470, #80910, #16511, #82761, #68103, #87989, #1837, #9388, #1372, #37350, #89382, #24072, #38272, #24537, #17455, #23142, #44908, #88924, #45362, #16055, #53893, #30724, #8924, #9866, #37802, #66708, #59624, #38741, #67184, #88472, #3228, #89861, #67646, #2319, #17913, #23619, #74265, #16976, #31200, #52948, #81825, #2772, #45841, #74745, #60544, #82304, #53421, #46305, #75209, #10324, #39191, #83691, #5113, #62411, #48640, #61935, #25471, #34456, #48170, #10789, #85100, #26417, #83224, #77071, #39650, #76139, #76609, #84623, #20250, #47710, #19308, #91253, #69973, #56237, #41532, #11733, #77542, #91730, #90317, #33504, #70458, #33991, #61485, #68573, #54813, #12692, #55307, #32595, #3710, #84160, #69500, #5585, #12202, #62894, #54350, #41045, #63365, #18369, #18852, #92195, #27351, #4631, #26883, #47229, #55770, #19771, #75665, #69043, #11273, #40126, #40586, #4172, #33045, #25930, #90771, #13162, #49586, #15006, #36309, #36774, #13618, #78482, #58114, #78937, #29215, #43865, #87412, #6980, #64770, #49126, #42471, #50523, #57183, #72308, #7429, #92662, #78022, #65225, #41998, #27834, #93138, #70912, #6045, #34917, #86479, #63829, #28293, #71381, #72762, #56723, #64313, #85569, #329, #14556, #20716, #93595, #22112, #14088, #6515, #35393, #50042, #86024, #21173, #42953, #71859, #35853, #28753, #21645, #57636, #79421, #86959, #43413, #50981, #79866, #7883, #65694, #808, #29688, #58572, #67530, #23954, #51433, #30141, #44334, #88807, #10204, #60887, #1715, #59025, #31081, #59501, #88353, #15461, #82183, #59969, #3112, #45245, #16856, #80322, #81247, #2660, #52372, #74150, #17339, #37688, #52829, #81707, #16394, #37239 ) ),
 .UNSPECIFIED., .F., .F., .F.,
 ( 4, 3, 3, 3, 3, 3, 3, 3, 3, 3, 3, 3, 4 ),
 ( 4, 3, 3, 3, 3, 3, 3, 3, 3, 3, 3, 3, 3, 3, 3, 3, 3, 3, 3, 3, 3, 3, 3, 3, 3, 3, 3, 3, 3, 3, 3, 3, 3, 3, 3, 3, 3, 3, 3, 3, 3, 3, 3, 3, 3, 3, 3, 3, 3, 3, 3, 3, 3, 3, 3, 3, 3, 3, 3, 3, 3, 3, 3, 3, 3, 3, 3, 3, 3, 3, 3, 3, 3, 3, 3, 3, 3, 3, 3, 3, 3, 3, 3, 3, 3, 3, 3, 3, 3, 3, 3, 3, 3, 3, 3, 3, 3, 3, 3, 3, 3, 3, 3, 3, 3, 3, 3, 3, 3, 3, 3, 3, 3, 3, 3, 3, 3, 3, 3, 3, 3, 3, 3, 3, 3, 3, 3, 3, 3, 3, 3, 3, 3, 3, 3, 3, 3, 3, 3, 3, 3, 3, 3, 3, 3, 3, 3, 3, 3, 3, 3, 3, 3, 3, 3, 3, 3, 3, 3, 3, 3, 3, 3, 3, 3, 3, 3, 3, 3, 3, 3, 3, 3, 3, 3, 3, 3, 3, 3, 3, 3, 3, 3, 3, 3, 3, 3, 3, 3, 3, 3, 3, 3, 3, 3, 3, 3, 3, 3, 3, 3, 3, 3, 3, 3, 3, 3, 3, 3, 3, 3, 3, 3, 3, 3, 3, 3, 3, 3, 3, 3, 3, 3, 3, 3, 3, 3, 3, 3, 3, 3, 3, 3, 3, 3, 3, 3, 3, 3, 3, 3, 3, 3, 3, 3, 3, 3, 3, 3, 3, 3, 3, 3, 3, 3, 3, 3, 3, 3, 3, 3, 3, 3, 3, 3, 3, 3, 3, 3, 3, 3, 3, 3, 3, 3, 3, 3, 3, 3, 3, 3, 3, 3, 3, 3, 3, 3, 3, 3, 3, 3, 3, 3, 3, 3, 3, 3, 3, 3, 3, 3, 3, 3, 4 ),
 ( -1.998401444325281773E-15, 0.06249999999999825140, 0.1249999999999985012, 0.1562499999999986122, 0.1874999999999987510, 0.2187499999999988898, 0.2499999999999990008, 0.2812499999999991118, 0.3124999999999992228, 0.3437499999999993339, 0.3749999999999995004, 0.4374999999999997780, 0.5000000000000000000 ),
 ( -0.05654842365434873536, -0.02821878541515033395, -0.01405396629555113498, -0.006971556735751535498, -0.003430351955851735756, -0.001659749565901835885, -0.0007744483709268859496, -0.0003317977734394109818, 0.0001108528240480639859, 0.003652057603947863728, 0.007193262383847663470, 0.01073446716374746278, 0.01427567194364726295, 0.01781687672354706140, 0.02135808150344686157, 0.02489928628334666175, 0.02844049106324646192, 0.03021109345319636375, 0.03198169584314626557, 0.03552290062304606227, 0.03906410540294585898, 0.04260531018284566263, 0.04437591257279556445, 0.04614651496274546627, 0.04968771974264526298, 0.05322892452254505968, 0.05677012930244486333, 0.05854073169239476515, 0.06031133408234466003, 0.06385253886224445674, 0.06739374364214426039, 0.07093494842204406403, 0.07270555081199396585, 0.07447615320194386768, 0.07801735798184365744, 0.08155856276174344721, 0.08509976754164325086, 0.08687036993159315268, 0.08864097232154305450, 0.09218217710144285815, 0.09572338188134266179, 0.09926458666124245156, 0.1010351890511923534, 0.1028057914411422413, 0.1063469962210420450, 0.1098882010009418486, 0.1134294057808416523, 0.1152000081707915541, 0.1169706105607414559, 0.1205118153406412596, 0.1240530201205410632, 0.1275942249004408668, 0.1293648272903907825, 0.1311354296803406705, 0.1346766344602404741, 0.1382178392401402500, 0.1417590440200400537, 0.1435296464099899416, 0.1453002487999398573, 0.1488414535798396332, 0.1523826583597394368, 0.1559238631396392405, 0.1576944655295891562, 0.1594650679195390441, 0.1630062726994388478, 0.1665474774793386514, 0.1700886822592384551, 0.1718592846491883708, 0.1736298870391382587, 0.1771710918190380624, 0.1807122965989378660, 0.1842535013788376697, 0.1860241037687875854, 0.1877947061587374733, 0.1913359109386372769, 0.1948771157185370528, 0.1984183204984368565, 0.2001889228883867444, 0.2019595252783366601, 0.2055007300582364360, 0.2090419348381362397, 0.2125831396180360433, 0.2143537420079859590, 0.2161243443979358470, 0.2196655491778356506, 0.2232067539577354542, 0.2267479587376352579, 0.2285185611275851736, 0.2302891635175350615, 0.2338303682974348652, 0.2373715730773346411, 0.2409127778572344447, 0.2426833802471843327, 0.2444539826371342484, 0.2479951874170340242, 0.2515363921969338001, 0.2550775969768336315, 0.2568481993667835472, 0.2586188017567334629, 0.2621600065366332388, 0.2657012113165330147, 0.2692424160964328461, 0.2710130184863827618, 0.2727836208763326775, 0.2763248256562324534, 0.2798660304361322293, 0.2834072352160320607, 0.2851778376059819764, 0.2869484399959318921, 0.2904896447758316680, 0.2940308495557314439, 0.2975720543356312753, 0.2993426567255811910, 0.3011132591155311067, 0.3046544638954308826, 0.3081956686753306585, 0.3117368734552304899, 0.3135074758451804056, 0.3152780782351303213, 0.3188192830150300972, 0.3223604877949298730, 0.3259016925748297044, 0.3276722949647795646, 0.3294428973547294803, 0.3329841021346292562, 0.3365253069145290876, 0.3400665116944288635, 0.3418371140843787792, 0.3436077164743286394, 0.3471489212542284708, 0.3506901260341282467, 0.3542313308140280226, 0.3560019332039779383, 0.3577725355939278540, 0.3613137403738276299, 0.3648549451537274058, 0.3683961499336272372, 0.3701667523235771529, 0.3719373547135270686, 0.3754785594934268445, 0.3790197642733266203, 0.3825609690532264517, 0.3843315714431763674, 0.3861021738331262831, 0.3896433786130260590, 0.3931845833929258349, 0.3967257881728256663, 0.3984963905627755820, 0.4002669929527254977, 0.4038081977326252736, 0.4073494025125250495, 0.4108906072924248809, 0.4126612096823747966, 0.4144318120723247123, 0.4179730168522244882, 0.4215142216321242641, 0.4250554264120240955, 0.4285966311919239269, 0.4321378359718237028, 0.4356790407517234787, 0.4392202455316233101, 0.4427614503115230860, 0.4463026550914228618, 0.4498438598713226932, 0.4533850646512224691, 0.4569262694311222450, 0.4586968718210721607, 0.4604674742110220764, 0.4640086789909218523, 0.4675498837708216282, 0.4710910885507214596, 0.4728616909406713198, 0.4746322933306212355, 0.4781734981105210114, 0.4817147028904208428, 0.4852559076703206742, 0.4870265100602705344, 0.4887971124502204501, 0.4923383172301202260, 0.4958795220100200574, 0.4994207267899198888, 0.5011913291798697490, 0.5029619315698197202, 0.5065031363497194405, 0.5100443411296192719, 0.5135855459095191033, 0.5153561482994689635, 0.5171267506894188237, 0.5206679554693186551, 0.5242091602492184865, 0.5277503650291182069, 0.5295209674190681781, 0.5312915698090180383, 0.5348327745889178697, 0.5383739793688175901, 0.5419151841487174215, 0.5436857865386672817, 0.5454563889286172529, 0.5489975937085169733, 0.5525387984884168047, 0.5560800032683166361, 0.5578506056582664963, 0.5596212080482163564, 0.5631624128281161878, 0.5667036176080160192, 0.5702448223879158506, 0.5720154247778657108, 0.5737860271678156820, 0.5773272319477154024, 0.5808684367276152338, 0.5844096415075150652, 0.5861802438974649254, 0.5879508462874147856, 0.5914920510673146170, 0.5950332558472144484, 0.5985744606271142798, 0.6003450630170641400, 0.6021156654070141112, 0.6056568701869138316, 0.6091980749668136630, 0.6127392797467134944, 0.6145098821366633546, 0.6162804845266132148, 0.6198216893065130462, 0.6233628940864128776, 0.6269040988663127090, 0.6286747012562625692, 0.6304453036462125404, 0.6339865084261122608, 0.6375277132060120922, 0.6410689179859119236, 0.6428395203758617837, 0.6446101227658116439, 0.6481513275457114753, 0.6516925323256113067, 0.6552337371055111381, 0.6570043394954609983, 0.6587749418854109695, 0.6623161466653106899, 0.6658573514452105213, 0.6693985562251103527, 0.6711691586150602129, 0.6729397610050100731, 0.6764809657849099045, 0.6800221705648097359, 0.6835633753447095673, 0.6853339777346594275, 0.6871045801246093987, 0.6906457849045091191, 0.6941869896844089505, 0.6977281944643087819, 0.6994987968542586421, 0.7012693992442085023, 0.7048106040241083337, 0.7083518088040081651, 0.7118930135839078854, 0.7136636159738578566, 0.7154342183638077168, 0.7189754231437075482, 0.7225166279236072686, 0.7260578327035071000, 0.7278284350934569602, 0.7295990374834069314, 0.7331402422633066518, 0.7366814470432064832, 0.7402226518231063146, 0.7419932542130561748, 0.7437638566030060350, 0.7473050613829058664, 0.7508462661628056978, 0.7543874709427054182, 0.7561580733326553894, 0.7579286757226052496, 0.7614698805025050810, 0.7650110852824048013, 0.7685522900623046327, 0.7703228924522544929, 0.7720934948422044641, 0.7756346996221041845, 0.7791759044020040159, 0.7827171091819038473, 0.7844877115718537075, 0.7862583139618035677, 0.7897995187417033991, 0.7933407235216032305, 0.7968819283015030619, 0.7986525306914529221, 0.8004231330814028933, 0.8039643378613026137, 0.8075055426412024451, 0.8110467474211022765, 0.8128173498110521367, 0.8145879522010019969, 0.8181291569809018283, 0.8216703617608016597, 0.8252115665407014911, 0.8269821689306513512, 0.8287527713206013225, 0.8322939761005010428, 0.8358351808804008742, 0.8393763856603007056, 0.8429175904402004260, 0.8464587952201002574, 0.8500000000000000888 ),
 .UNSPECIFIED. ) ;
#54165 = CARTESIAN_POINT ( 'NONE',  ( -15.81668226956704437, -284.5299966992748182, -341.1752946549420926 ) ) ;
#54166 = CARTESIAN_POINT ( 'NONE',  ( -99.56188087693280409, -292.5693872661504997, -226.0073650280881452 ) ) ;
#54167 = CARTESIAN_POINT ( 'NONE',  ( -22.30719664980588490, -293.5558465555933481, -195.2920634523905790 ) ) ;
#54168 = CARTESIAN_POINT ( 'NONE',  ( 16.15769396357575616, -294.0993445966775539, -320.0281577205441295 ) ) ;
#54169 = CARTESIAN_POINT ( 'NONE',  ( 17.41777575143020229, -288.8344578622092627, -219.0937542781570926 ) ) ;
#54170 = CARTESIAN_POINT ( 'NONE',  ( 11.49423899803039006, -282.5632069539214513, -329.9620495350150691 ) ) ;
#54171 = CARTESIAN_POINT ( 'NONE',  ( -96.20880343660680012, -295.2789984273261439, -222.9904693623223011 ) ) ;
#54172 = CARTESIAN_POINT ( 'NONE',  ( 9.207117593550204759, -282.2657466507333766, -331.6979549828733980 ) ) ;
#54173 = CARTESIAN_POINT ( 'NONE',  ( 36.33469206697079557, -277.6906994140549614, -282.6588970334490796 ) ) ;
#54174 = CARTESIAN_POINT ( 'NONE',  ( -67.68488546085839630, -297.9805209788416391, -333.4427485647536855 ) ) ;
#54175 = CARTESIAN_POINT ( 'NONE',  ( -96.11153733409877020, -276.0394692712719689, -318.1978790994803035 ) ) ;
#54176 = CARTESIAN_POINT ( 'NONE',  ( 164.2231345125756263, 293.9636489450775230, 0.000000000000000000 ) ) ;
#54177 = CARTESIAN_POINT ( 'NONE',  ( -91.71503398925338502, -283.3617779264020555, -319.1808570932154225 ) ) ;
#54178 = CARTESIAN_POINT ( 'NONE',  ( -7.704856378814294970, -281.6371007568332061, -199.7093206184912901 ) ) ;
#54179 = CARTESIAN_POINT ( 'NONE',  ( 28.50291222047669493, -286.0935370845697321, -230.7958420713842997 ) ) ;
#54180 = CARTESIAN_POINT ( 'NONE',  ( -60.59835322099827692, -293.5065951240130175, -200.0428200160021959 ) ) ;
#54181 = CARTESIAN_POINT ( 'NONE',  ( 35.30614460431431922, -277.4443150188960203, -293.3552709575204744 ) ) ;
#54182 = CARTESIAN_POINT ( 'NONE',  ( 21.46101486130531555, -276.2047420173916521, -221.4168743546945848 ) ) ;
#54183 = CARTESIAN_POINT ( 'NONE',  ( -45.91020518985178711, -276.9970026567052628, -342.9071279572621052 ) ) ;
#54184 = CARTESIAN_POINT ( 'NONE',  ( -76.18347497306811533, -299.5323573762630645, -206.3374066044498534 ) ) ;
#54185 = CARTESIAN_POINT ( 'NONE',  ( -44.16684723920729283, -283.9654691774103981, -195.8396727926966037 ) ) ;
#54186 = CARTESIAN_POINT ( 'NONE',  ( -22.19379459336163407, -291.9076566441407294, -194.8330674582151971 ) ) ;
#54187 = CARTESIAN_POINT ( 'NONE',  ( -110.4702084345482973, -292.4237138758828110, -248.9447296573441122 ) ) ;
#54188 = CARTESIAN_POINT ( 'NONE',  ( -1.091915261902661749, -291.4656311383803313, -206.6270448332325032 ) ) ;
#54189 = ORIENTED_EDGE ( 'NONE', *, *, #31528, .T. ) ;
#54190 = CARTESIAN_POINT ( 'NONE',  ( 6.175662656369911296, -291.2049992168653034, -207.5531134937818933 ) ) ;
#54191 = EDGE_CURVE ( 'NONE', #49322, #86359, #63635, .T. ) ;
#54192 = CARTESIAN_POINT ( 'NONE',  ( -46.99305993686557770, -291.5928996371412154, -197.9806044408231287 ) ) ;
#54193 = VERTEX_POINT ( 'NONE', #16908 ) ;
#54194 = CARTESIAN_POINT ( 'NONE',  ( -91.37096054294096348, -290.8784016147202465, -324.8631133841032010 ) ) ;
#54195 = CARTESIAN_POINT ( 'NONE',  ( -94.87621839796359779, -279.8387046437596837, -225.2447159202324656 ) ) ;
#54196 = CARTESIAN_POINT ( 'NONE',  ( -111.9703692608760548, -295.6943165506294804, -252.6960605321189632 ) ) ;
#54197 = CARTESIAN_POINT ( 'NONE',  ( -73.57233305379359933, -286.2360350986262461, -202.4740180238676999 ) ) ;
#54198 = CARTESIAN_POINT ( 'NONE',  ( 14.22956605511410899, -287.0863711728291605, -213.1393770527902234 ) ) ;
#54200 = CARTESIAN_POINT ( 'NONE',  ( -109.5185953549989364, -284.7351460723400010, -281.7571326386113242 ) ) ;
#54199 = CIRCLE ( 'NONE', #63296, 5.841085083515828558 ) ;
#54201 = CARTESIAN_POINT ( 'NONE',  ( -48.55409767855074676, -154.7049544282185707, -365.0407483515538161 ) ) ;
#54202 = CARTESIAN_POINT ( 'NONE',  ( 4.175116275386621112, -57.89727328217816194, -353.1401067649683228 ) ) ;
#54203 = CARTESIAN_POINT ( 'NONE',  ( -13.16113611277997286, -92.07136048423980412, -356.2614093299528690 ) ) ;
#54204 = CARTESIAN_POINT ( 'NONE',  ( -16.34428335865657544, -275.9710053673329639, -340.4978363436782729 ) ) ;
#54205 = CARTESIAN_POINT ( 'NONE',  ( -26.99140282775333333, -275.8377754050243880, -342.9358892107668453 ) ) ;
#54206 = CARTESIAN_POINT ( 'NONE',  ( -80.58524852322130982, -296.9908841998434923, -206.6612070728645847 ) ) ;
#54207 = CARTESIAN_POINT ( 'NONE',  ( -101.2730542070560631, -255.2172494999240939, -324.5853935562917059 ) ) ;
#54208 = CARTESIAN_POINT ( 'NONE',  ( -17.50202521352245100, -275.4861885082246431, -344.2508031272387825 ) ) ;
#54209 = CARTESIAN_POINT ( 'NONE',  ( -104.1289863278719992, -274.7377560944700576, -238.4639016002249150 ) ) ;
#54210 = CARTESIAN_POINT ( 'NONE',  ( -107.0622175921625541, -291.3342242559098736, -248.4777640785070787 ) ) ;
#54211 = CARTESIAN_POINT ( 'NONE',  ( -66.85294953455573363, -296.2319582254946226, -341.3206550665373697 ) ) ;
#54212 = CARTESIAN_POINT ( 'NONE',  ( -40.44406008143359799, -298.5066111514885847, -193.4331447318857897 ) ) ;
#54213 = CARTESIAN_POINT ( 'NONE',  ( -6.762974776336586835, -294.8058561910875710, -336.6479308520583800 ) ) ;
#54214 = VERTEX_POINT ( 'NONE', #82695 ) ;
#54215 = CARTESIAN_POINT ( 'NONE',  ( -45.46994408713371882, -279.0743969435646932, -345.5347241672198493 ) ) ;
#54216 = ADVANCED_FACE ( 'NONE', ( #53349 ), #16741, .T. ) ;
#54217 = CARTESIAN_POINT ( 'NONE',  ( -1.158829664570814266, -280.0268634296121490, -202.4617307364441388 ) ) ;
#54218 = CARTESIAN_POINT ( 'NONE',  ( -4.951263143486116292, -277.5561718139133518, -336.0581420091110090 ) ) ;
#54219 = CARTESIAN_POINT ( 'NONE',  ( 38.69364737444505664, -277.3221468995234886, -271.1386050336082008 ) ) ;
#54220 = CARTESIAN_POINT ( 'NONE',  ( -106.0557790435301371, -271.3861665340733680, -243.5918377119631089 ) ) ;
#54221 = CARTESIAN_POINT ( 'NONE',  ( 151.0356227160792173, 20.07892719424426531, -6.469110745567457244 ) ) ;
#54222 = EDGE_CURVE ( 'NONE', #70758, #44168, #44270, .T. ) ;
#54223 = CARTESIAN_POINT ( 'NONE',  ( -103.3707550275782125, -279.1408952144284399, -239.1108996205265953 ) ) ;
#54224 = CARTESIAN_POINT ( 'NONE',  ( -0.1326142521014597453, -275.3369914631144297, -203.1178688480154904 ) ) ;
#54225 = CARTESIAN_POINT ( 'NONE',  ( -34.70072416815290239, -287.7044471030052364, -346.8223730069888120 ) ) ;
#54226 = CARTESIAN_POINT ( 'NONE',  ( -19.06272597346500675, -276.2874411237381196, -197.5690879805409566 ) ) ;
#54227 = CARTESIAN_POINT ( 'NONE',  ( 197.3748232817348764, 214.9910457053126720, -12.45182892472558756 ) ) ;
#54228 = CARTESIAN_POINT ( 'NONE',  ( -104.1994306258546459, -289.3487598654411386, -300.1956215619385375 ) ) ;
#54229 = CARTESIAN_POINT ( 'NONE',  ( -83.20842201836086360, -284.7912459432007495, -208.5731160702488580 ) ) ;
#54230 = CARTESIAN_POINT ( 'NONE',  ( 33.71362441991469439, -279.5217295442126897, -249.6460300550033651 ) ) ;
#54232 = CARTESIAN_POINT ( 'NONE',  ( -24.87709350065013325, -284.2920719180544324, -196.9197892110969974 ) ) ;
#54231 = CARTESIAN_POINT ( 'NONE',  ( 33.52199464820392194, -280.3870375958060777, -290.2032872373982286 ) ) ;
#54233 = CARTESIAN_POINT ( 'NONE',  ( -72.52723074908284673, -291.5180280395061914, -336.6096410231270397 ) ) ;
#54234 = CARTESIAN_POINT ( 'NONE',  ( -109.2794766816137866, -279.9491332198462601, -255.7347404808160718 ) ) ;
#54235 = CARTESIAN_POINT ( 'NONE',  ( 153.9124347780988558, 19.64445381522117273, -13.06493381020000477 ) ) ;
#54236 = CARTESIAN_POINT ( 'NONE',  ( 3.411515403631638854, -278.9897245405375656, -205.9123239624678661 ) ) ;
#54237 = CARTESIAN_POINT ( 'NONE',  ( -25.36654160979586692, -294.2049700471081337, -196.3233153089201721 ) ) ;
#54238 = CARTESIAN_POINT ( 'NONE',  ( -111.0968542681884514, -277.0243621970629988, -252.0279950036088508 ) ) ;
#54239 = CARTESIAN_POINT ( 'NONE',  ( -21.62302894800675901, -277.4968351821499368, -341.8051730164002038 ) ) ;
#54240 = CARTESIAN_POINT ( 'NONE',  ( -19.33235961746500564, -284.8212877188626067, -343.3921109489503465 ) ) ;
#54241 = CARTESIAN_POINT ( 'NONE',  ( 199.2180164324846885, 65.99917555505274436, 9.231954786409863445 ) ) ;
#54242 = CARTESIAN_POINT ( 'NONE',  ( -111.4507632717454442, -292.2836565199086181, -285.1629776817619017 ) ) ;
#54243 = CARTESIAN_POINT ( 'NONE',  ( 28.56531585670742146, -286.2319341979917908, -230.7562762363980085 ) ) ;
#54244 = CARTESIAN_POINT ( 'NONE',  ( -33.44604961925815445, -290.5018405187756230, -196.6513770150382072 ) ) ;
#54245 = CARTESIAN_POINT ( 'NONE',  ( -48.18343439337095191, -257.6947538200772101, -441.8664075291517861 ) ) ;
#54246 = CARTESIAN_POINT ( 'NONE',  ( 24.38957341470759133, -274.7865101104688392, -310.3359109574766990 ) ) ;
#54247 = CARTESIAN_POINT ( 'NONE',  ( 29.49653226403537332, -292.1230395086887484, -302.7830874750350745 ) ) ;
#54248 = CARTESIAN_POINT ( 'NONE',  ( 180.0056393205866812, 275.0000000000000568, -23.52000000000002800 ) ) ;
#54249 = CARTESIAN_POINT ( 'NONE',  ( 204.5044540939250055, -142.7221692137691775, 10.75739200365177695 ) ) ;
#54250 = CARTESIAN_POINT ( 'NONE',  ( -96.91006988601124306, -289.6766801822311663, -222.6713173928956735 ) ) ;
#54251 = CARTESIAN_POINT ( 'NONE',  ( -44.11789767307843846, -287.5651773448868767, -196.8728633981021403 ) ) ;
#54252 = CARTESIAN_POINT ( 'NONE',  ( -3.532012552953720963, -286.8519857654526390, -338.4261147132313567 ) ) ;
#54253 = CARTESIAN_POINT ( 'NONE',  ( 16.39241035757632758, -288.2596624369529650, -220.0631055782272369 ) ) ;
#54254 = DIRECTION ( 'NONE',  ( 0.000000000000000000, 0.000000000000000000, 1.000000000000000000 ) ) ;
#54255 = CARTESIAN_POINT ( 'NONE',  ( 24.38005006197849767, -288.8969061526918836, -309.6425039094027056 ) ) ;
#54256 = CARTESIAN_POINT ( 'NONE',  ( -4.070783131847124814, -294.4685365476391894, -202.7343734838937337 ) ) ;
#54257 = CARTESIAN_POINT ( 'NONE',  ( -31.58484446399026524, -275.0599930413331435, -345.7531370534237567 ) ) ;
#54258 = CARTESIAN_POINT ( 'NONE',  ( -114.1899909918911504, -278.9414962150229371, -265.8795465218101413 ) ) ;
#54259 = CARTESIAN_POINT ( 'NONE',  ( -68.99714594278383117, -289.7190220462043726, -201.7376668321577426 ) ) ;
#54260 = CARTESIAN_POINT ( 'NONE',  ( -114.3778064568944473, -278.5724984469516698, -268.7342460199392349 ) ) ;
#54261 = CARTESIAN_POINT ( 'NONE',  ( -68.76235899478038505, -299.6170060965190487, -202.6375507934338600 ) ) ;
#54262 = CARTESIAN_POINT ( 'NONE',  ( -48.18343439339133027, -259.2200010660633893, -490.9919136895239262 ) ) ;
#54263 = CARTESIAN_POINT ( 'NONE',  ( -111.4792264354816496, -282.4020810444002905, -282.0364618641495440 ) ) ;
#54264 = CARTESIAN_POINT ( 'NONE',  ( -48.18343439339133027, -273.4572633954001049, -501.0766502680399412 ) ) ;
#54265 = CARTESIAN_POINT ( 'NONE',  ( -98.68261331631168787, -276.1197464466183078, -312.1720956079731764 ) ) ;
#54266 = CARTESIAN_POINT ( 'NONE',  ( 26.17159961013963709, -279.0146858647894419, -230.3756277867683480 ) ) ;
#54267 = DIRECTION ( 'NONE',  ( -0.000000000000000000, -0.000000000000000000, -1.000000000000000000 ) ) ;
#54268 = CARTESIAN_POINT ( 'NONE',  ( -17.55649340310105444, -275.2812735462158003, -344.0581555474273614 ) ) ;
#54269 = CARTESIAN_POINT ( 'NONE',  ( -67.56199773301453604, -296.9760875402213856, -337.5868661549849321 ) ) ;
#54270 = CARTESIAN_POINT ( 'NONE',  ( 24.84853269909145723, -281.0701806179488926, -315.2595392251381554 ) ) ;
#54271 = CARTESIAN_POINT ( 'NONE',  ( -92.93080483620325083, -298.1701144406042090, -222.6631096285022693 ) ) ;
#54272 = CARTESIAN_POINT ( 'NONE',  ( -113.8724468745746350, -297.8407426462014769, -272.4729998593145410 ) ) ;
#54273 = CARTESIAN_POINT ( 'NONE',  ( -56.86318510286623962, -273.4602324978485512, -199.9450507135116482 ) ) ;
#54274 = CARTESIAN_POINT ( 'NONE',  ( 16.28830337206679602, -294.8132240839003657, -217.8575379677758121 ) ) ;
#54275 = CARTESIAN_POINT ( 'NONE',  ( 1.519845867310069432, -286.7232157719415113, -203.8718733310966513 ) ) ;
#54276 = CARTESIAN_POINT ( 'NONE',  ( 11.88383322424419042, -274.5161321889597730, -327.9558429501450405 ) ) ;
#54277 = CARTESIAN_POINT ( 'NONE',  ( -40.34088398147816434, -288.9221676367471900, -347.3157677629409932 ) ) ;
#54278 = CARTESIAN_POINT ( 'NONE',  ( 11.29925779746202075, -285.8043899257965563, -215.5438567272127557 ) ) ;
#54279 = CARTESIAN_POINT ( 'NONE',  ( -98.38794543784490543, -289.1445077773954040, -226.7909839002715842 ) ) ;
#54280 = ORIENTED_EDGE ( 'NONE', *, *, #37333, .F. ) ;
#54281 = CARTESIAN_POINT ( 'NONE',  ( 197.3296566515638517, 72.17749256844233230, 11.72628858667597740 ) ) ;
#54282 = CARTESIAN_POINT ( 'NONE',  ( -39.96654905466119345, -288.5935412221524530, -343.4251110606689963 ) ) ;
#54283 = DIRECTION ( 'NONE',  ( 0.000000000000000000, 1.000000000000000000, 0.000000000000000000 ) ) ;
#54284 = CARTESIAN_POINT ( 'NONE',  ( -110.4577676580129122, -285.1979998434574100, -293.7895017599760195 ) ) ;
#54285 = CARTESIAN_POINT ( 'NONE',  ( 38.37221553467777824, -292.7706920483784643, -283.0986210119398834 ) ) ;
#54286 = CARTESIAN_POINT ( 'NONE',  ( 35.82579292587770681, -282.8820415415041793, -249.0315653850595936 ) ) ;
#54287 = CARTESIAN_POINT ( 'NONE',  ( 39.12742986579735316, -282.8975608405727939, -272.7632898019847971 ) ) ;
#54288 = CARTESIAN_POINT ( 'NONE',  ( -84.86338689133147284, -283.5626794147622149, -325.7749185349479148 ) ) ;
#54289 = CARTESIAN_POINT ( 'NONE',  ( -15.78223258401995466, -278.7735471704858128, -342.2500475701118035 ) ) ;
#54290 = CARTESIAN_POINT ( 'NONE',  ( -114.1208200687033383, -296.6333268327786641, -263.8704576249846241 ) ) ;
#54291 = CARTESIAN_POINT ( 'NONE',  ( -8.794634858030523361, -275.7486761903030583, -202.5845589780735168 ) ) ;
#54292 = CARTESIAN_POINT ( 'NONE',  ( -58.08844729270684581, -289.8030236876819004, -198.6033643427983861 ) ) ;
#54293 = CARTESIAN_POINT ( 'NONE',  ( -108.9187350773352421, -271.5601969347183058, -254.1173938365915888 ) ) ;
#54294 = ORIENTED_EDGE ( 'NONE', *, *, #83427, .F. ) ;
#54295 = DIRECTION ( 'NONE',  ( -1.000000000000000000, 0.000000000000000000, 0.000000000000000000 ) ) ;
#54296 = CARTESIAN_POINT ( 'NONE',  ( -103.0306629604617825, -286.0030208859412824, -305.4889604292825993 ) ) ;
#54297 = CARTESIAN_POINT ( 'NONE',  ( 26.26309263966161822, -295.1986084039461389, -313.2087882425091721 ) ) ;
#54298 = CARTESIAN_POINT ( 'NONE',  ( -77.11146713443663714, -286.1553927568982658, -208.9638037404032502 ) ) ;
#54299 = CARTESIAN_POINT ( 'NONE',  ( 28.88687997502078275, -275.1176961439708748, -309.1760041730879038 ) ) ;
#54300 = CARTESIAN_POINT ( 'NONE',  ( -68.29535452788744010, -292.3075627570773918, -199.9537009809486108 ) ) ;
#54301 = CARTESIAN_POINT ( 'NONE',  ( -113.1054644874674011, -282.6967792829082669, -269.9642705730184389 ) ) ;
#54302 = CARTESIAN_POINT ( 'NONE',  ( -27.85590764017713283, -292.5026065360077041, -193.9152860027418797 ) ) ;
#54303 = CARTESIAN_POINT ( 'NONE',  ( -88.67291715428244459, -290.1305208578724546, -322.2956310287819406 ) ) ;
#54304 = DIRECTION ( 'NONE',  ( 1.000000000000000000, 0.000000000000000000, 0.000000000000000000 ) ) ;
#54305 = CARTESIAN_POINT ( 'NONE',  ( 157.4851178187871312, 1.000000000000000000, 10.00000000000000000 ) ) ;
#54306 = CARTESIAN_POINT ( 'NONE',  ( 173.7762727166613956, 240.3961790201574331, -177.1038114315761050 ) ) ;
#54307 = CARTESIAN_POINT ( 'NONE',  ( -111.6886213027323294, -286.2891139365405024, -253.1784794286780027 ) ) ;
#54308 = CARTESIAN_POINT ( 'NONE',  ( -110.4542110544635705, -294.2666405000204577, -253.6410175316879361 ) ) ;
#54309 = ORIENTED_EDGE ( 'NONE', *, *, #24971, .T. ) ;
#54310 = CARTESIAN_POINT ( 'NONE',  ( 19.08279215259122452, -279.8113409422058453, -223.5388233256990418 ) ) ;
#54311 = CARTESIAN_POINT ( 'NONE',  ( -34.29618122368770372, -276.6815611411086024, -347.2797055033150855 ) ) ;
#54312 = CARTESIAN_POINT ( 'NONE',  ( -102.4183647061939837, -281.0459011251180641, -233.4144516712925679 ) ) ;
#54313 = CARTESIAN_POINT ( 'NONE',  ( 169.6295731601628347, 230.2267480612287329, -191.3574351880446045 ) ) ;
#54314 = CARTESIAN_POINT ( 'NONE',  ( -92.02482966979169987, -282.3891808533316521, -323.7311623510848904 ) ) ;
#54315 = CARTESIAN_POINT ( 'NONE',  ( -109.6150329445279112, -282.8132396817231324, -251.6953158487823430 ) ) ;
#54316 = CARTESIAN_POINT ( 'NONE',  ( -104.5247966912737070, -274.8730284687417225, -235.2228534304302343 ) ) ;
#54317 = CARTESIAN_POINT ( 'NONE',  ( -35.64290255593734713, -295.5226499768471058, -343.4154107262830280 ) ) ;
#54318 = VERTEX_POINT ( 'NONE', #44739 ) ;
#54319 = CARTESIAN_POINT ( 'NONE',  ( 22.21410783344179052, -291.6383679442908488, -227.2775563091246340 ) ) ;
#54320 = CARTESIAN_POINT ( 'NONE',  ( -41.37079839258058911, -277.7530114182702050, -347.1667514060834492 ) ) ;
#54321 = CARTESIAN_POINT ( 'NONE',  ( 34.84165639972377448, -275.4074030803654409, -259.3883461098668022 ) ) ;
#54322 = CARTESIAN_POINT ( 'NONE',  ( 13.76875386746906216, -273.6689094343150828, -213.1130992726049556 ) ) ;
#54323 = CYLINDRICAL_SURFACE ( 'NONE', #34096, 1.000000000000000888 ) ;
#54324 = CARTESIAN_POINT ( 'NONE',  ( -103.9237073279815462, -271.0102920859906703, -235.7266728840971552 ) ) ;
#54325 = CARTESIAN_POINT ( 'NONE',  ( 25.24255633223820894, -295.5618059826121566, -314.2224950278564393 ) ) ;
#54326 = EDGE_CURVE ( 'NONE', #75749, #47327, #66088, .T. ) ;
#54327 = CARTESIAN_POINT ( 'NONE',  ( 11.63197158325052172, -282.8906705383787994, 47.50000000000000711 ) ) ;
#54328 = VECTOR ( 'NONE', #27747, 1000.000000000000000 ) ;
#54329 = CARTESIAN_POINT ( 'NONE',  ( -43.39882518443393167, -263.1823801016103630, -501.4546314904750943 ) ) ;
#54330 = CARTESIAN_POINT ( 'NONE',  ( -18.64357965821731611, -283.8854354482718350, -341.2982047164005053 ) ) ;
#54331 = CARTESIAN_POINT ( 'NONE',  ( 26.98145658973689365, -282.7743815291684655, -229.8088093915696390 ) ) ;
#54332 = CARTESIAN_POINT ( 'NONE',  ( -107.8616777658547363, -283.6461190332594811, -289.6652264153267424 ) ) ;
#54333 = CARTESIAN_POINT ( 'NONE',  ( -40.56083621764730651, -275.4931399487513772, -344.1034791841074139 ) ) ;
#54334 = CARTESIAN_POINT ( 'NONE',  ( 23.61230036274744393, -283.9933043814972962, -312.7341672628170386 ) ) ;
#54335 = CARTESIAN_POINT ( 'NONE',  ( -106.9252270675567900, -276.7104583770554314, -294.7820326538454765 ) ) ;
#54336 = CARTESIAN_POINT ( 'NONE',  ( 35.14524295344944704, -276.4869002304594119, -259.3282821274389676 ) ) ;
#54337 = DIRECTION ( 'NONE',  ( 1.000000000000000000, 0.000000000000000000, -2.940294503956655304E-16 ) ) ;
#54338 = SHAPE_REPRESENTATION ( 'Reciprocating Rivet Punch Pin', ( #18940 ), #43137 ) ;
#54339 = CARTESIAN_POINT ( 'NONE',  ( -50.92115537272334791, -280.6856905532321775, -194.7320414623887643 ) ) ;
#54340 = ORIENTED_EDGE ( 'NONE', *, *, #89067, .F. ) ;
#54341 = DIRECTION ( 'NONE',  ( 0.000000000000000000, 0.000000000000000000, 1.000000000000000000 ) ) ;
#54342 = CARTESIAN_POINT ( 'NONE',  ( -112.5955659863347478, -286.5242158929484617, -261.5769758555161957 ) ) ;
#54343 = CARTESIAN_POINT ( 'NONE',  ( -35.65712385050216682, -294.2276797161182458, -343.5157222871457634 ) ) ;
#54344 = EDGE_CURVE ( 'NONE', #78327, #93327, #48802, .T. ) ;
#54345 = CARTESIAN_POINT ( 'NONE',  ( -105.0701169924137304, -289.4292898113963020, -306.7777945929239536 ) ) ;
#54346 = CARTESIAN_POINT ( 'NONE',  ( 36.64189138387394706, -285.8371288707806457, -273.8293602605959336 ) ) ;
#54348 = CARTESIAN_POINT ( 'NONE',  ( -111.3202212809849243, -288.7454923422922661, -273.9358544989065649 ) ) ;
#54347 = CARTESIAN_POINT ( 'NONE',  ( 34.28801370882838739, -285.9054185147584235, -253.4377257516967177 ) ) ;
#54349 = CARTESIAN_POINT ( 'NONE',  ( -65.45366311071562393, -284.6331225364976945, -338.1748484081325614 ) ) ;
#54350 = CARTESIAN_POINT ( 'NONE',  ( 34.14833287875688939, -273.8446070350688046, -293.0365635037624656 ) ) ;
#54351 = CARTESIAN_POINT ( 'NONE',  ( 38.77967236081282465, -285.8954683745651550, -265.8859058378374698 ) ) ;
#54352 = CARTESIAN_POINT ( 'NONE',  ( -79.52182682176520245, -299.4829905177365390, -208.2838452961748601 ) ) ;
#54353 = CARTESIAN_POINT ( 'NONE',  ( 19.17716402239479123, -286.2390077313106644, -319.9349797677945162 ) ) ;
#54354 = ADVANCED_FACE ( 'NONE', ( #45187 ), #47050, .F. ) ;
#54355 = CARTESIAN_POINT ( 'NONE',  ( 31.28661004284614222, -282.1517877656277733, -244.6508050043901505 ) ) ;
#54356 = CARTESIAN_POINT ( 'NONE',  ( -37.47221339726154099, -291.0539023684440849, -345.5404367147966695 ) ) ;
#54357 = DIRECTION ( 'NONE',  ( -0.000000000000000000, 1.000000000000000000, -0.000000000000000000 ) ) ;
#54358 = CARTESIAN_POINT ( 'NONE',  ( -97.11994273655210463, -297.8436128276508157, -316.5766555478507485 ) ) ;
#54359 = CARTESIAN_POINT ( 'NONE',  ( -71.83954586158834843, -277.5960702478371331, -203.7516071013835699 ) ) ;
#54360 = CARTESIAN_POINT ( 'NONE',  ( -27.85885903047549661, -291.3666758245070696, -194.0564273165381906 ) ) ;
#54361 = CARTESIAN_POINT ( 'NONE',  ( -108.9462434943731921, -295.1858563333981920, -252.4424377755413786 ) ) ;
#54362 = CARTESIAN_POINT ( 'NONE',  ( 20.91705214173948235, -279.6104835098763033, -225.5393043626210101 ) ) ;
#54363 = CARTESIAN_POINT ( 'NONE',  ( 18.37939749841876846, -272.9396768566480205, -220.9240605947728113 ) ) ;
#54364 = CARTESIAN_POINT ( 'NONE',  ( 19.22331240470157709, -295.5283291280866251, -317.2827850093944448 ) ) ;
#54365 = CARTESIAN_POINT ( 'NONE',  ( 39.58706461736020543, -296.0519495502701943, -270.3284710469133074 ) ) ;
#54366 = CARTESIAN_POINT ( 'NONE',  ( -107.5290224979771807, -271.5161465874575697, -240.0223143437607973 ) ) ;
#54367 = CARTESIAN_POINT ( 'NONE',  ( -3.697879230575534582, -292.8542783376716443, -338.5082465673480101 ) ) ;
#54368 = CARTESIAN_POINT ( 'NONE',  ( -63.02323098353827646, -293.1363140260699538, -201.3985637232659371 ) ) ;
#54369 = DIRECTION ( 'NONE',  ( -0.8946341770721975006, -0.4467993836324665180, 0.000000000000000000 ) ) ;
#54370 = CARTESIAN_POINT ( 'NONE',  ( 35.36859930742924263, -294.4676364044116781, -278.9192985079345135 ) ) ;
#54371 = CARTESIAN_POINT ( 'NONE',  ( 158.6539576904058606, 293.9636489450775230, 0.000000000000000000 ) ) ;
#54373 = CARTESIAN_POINT ( 'NONE',  ( -38.34229317417686644, -295.0650408441347849, -343.3542602190476032 ) ) ;
#54372 = CARTESIAN_POINT ( 'NONE',  ( -95.91029375534257895, -281.9222890578718648, -317.7958171708838790 ) ) ;
#54374 = CARTESIAN_POINT ( 'NONE',  ( 37.86552806408568017, -281.7595048671323639, -286.9408716284606271 ) ) ;
#54375 = CARTESIAN_POINT ( 'NONE',  ( -21.73442281157464606, -282.5240722037501087, -345.7412027941464316 ) ) ;
#54376 = CARTESIAN_POINT ( 'NONE',  ( 13.38017965774569440, -286.3408371401578165, -325.4525892238079905 ) ) ;
#54377 = DIRECTION ( 'NONE',  ( 0.000000000000000000, 0.000000000000000000, -1.000000000000000000 ) ) ;
#54378 = CARTESIAN_POINT ( 'NONE',  ( 35.93934562868398785, -279.7622950456687931, -249.0399271567522703 ) ) ;
#54379 = CARTESIAN_POINT ( 'NONE',  ( 33.75059532463390610, -286.8407465208177314, -299.2666853064187080 ) ) ;
#54380 = CARTESIAN_POINT ( 'NONE',  ( -48.18343439339133027, -293.9810843561368756, -432.7152727200224263 ) ) ;
#54381 = CARTESIAN_POINT ( 'NONE',  ( -31.51912926246497193, -296.5776929383341098, -343.9817338471044081 ) ) ;
#54382 = CARTESIAN_POINT ( 'NONE',  ( 20.38709532053276163, -277.6592569973349782, -320.4408157471359573 ) ) ;
#54383 = CARTESIAN_POINT ( 'NONE',  ( -79.06347333526062471, -279.1385904977764199, -210.4329849635005871 ) ) ;
#54384 = CARTESIAN_POINT ( 'NONE',  ( -33.54148808690165851, -292.2654278876781859, -193.4549518256146712 ) ) ;
#54385 = CARTESIAN_POINT ( 'NONE',  ( -30.37251406328121561, -281.0444921009496966, -345.5990382302692865 ) ) ;
#54386 = CARTESIAN_POINT ( 'NONE',  ( -91.86213878092823393, -279.8295787473639962, -321.9382570641489565 ) ) ;
#54388 = CARTESIAN_POINT ( 'NONE',  ( 32.56785208163888257, -292.8991055851751071, -292.1799850036206863 ) ) ;
#54387 = VECTOR ( 'NONE', #81869, 1000.000000000000000 ) ;
#54389 = CARTESIAN_POINT ( 'NONE',  ( -108.8970957867788769, -294.8438361496554876, -247.7208165099362134 ) ) ;
#54390 = ORIENTED_EDGE ( 'NONE', *, *, #91848, .T. ) ;
#54391 = CYLINDRICAL_SURFACE ( 'NONE', #34806, 0.5000000000000004441 ) ;
#54392 = CARTESIAN_POINT ( 'NONE',  ( 14.35539498686518911, -293.8090642734588300, -322.0597462178400292 ) ) ;
#54393 = CARTESIAN_POINT ( 'NONE',  ( 189.9243309297870610, 275.0000000000000568, 20.22542485937349355 ) ) ;
#54394 = AXIS2_PLACEMENT_3D ( 'NONE', #39435, #67889, #3012 ) ;
#54395 = CARTESIAN_POINT ( 'NONE',  ( -53.35057174420112602, -286.7666405000204577, -340.3538533559490702 ) ) ;
#54396 = CARTESIAN_POINT ( 'NONE',  ( -35.46697519860013159, -297.1338385394712986, -193.5967014325774755 ) ) ;
#54397 = CARTESIAN_POINT ( 'NONE',  ( 36.92993136920981811, -279.8819839520191408, -285.3287576796730036 ) ) ;
#54398 = CARTESIAN_POINT ( 'NONE',  ( -82.99511457280848958, -286.7575166729280340, -208.9023401924321774 ) ) ;
#54399 = CARTESIAN_POINT ( 'NONE',  ( -15.85367591066476756, -288.5997766288515436, -340.1797280768398650 ) ) ;
#54400 = CARTESIAN_POINT ( 'NONE',  ( -102.4606320305192497, -279.6067401586857386, -304.8608637575646867 ) ) ;
#54401 = CARTESIAN_POINT ( 'NONE',  ( -101.4224178539420365, -274.6496410711240515, -233.6509016872105917 ) ) ;
#54402 = CARTESIAN_POINT ( 'NONE',  ( -107.6028111018489568, -277.6265711124902964, -249.1359727553659411 ) ) ;
#54403 = ORIENTED_EDGE ( 'NONE', *, *, #49364, .T. ) ;
#54404 = CARTESIAN_POINT ( 'NONE',  ( -106.8423102469622279, -272.8103974973882941, -237.2149990907893482 ) ) ;
#54405 = CARTESIAN_POINT ( 'NONE',  ( -111.8089503080287699, -292.4970529479311381, -268.4486911278731895 ) ) ;
#54406 = CARTESIAN_POINT ( 'NONE',  ( 36.30409391824681364, -294.9041970755569650, -250.7471522297435911 ) ) ;
#54407 = CARTESIAN_POINT ( 'NONE',  ( 197.8536156918379447, 70.38469146215045669, -8.282373351500920577 ) ) ;
#54408 = EDGE_CURVE ( 'NONE', #60602, #12757, #22753, .T. ) ;
#54409 = CARTESIAN_POINT ( 'NONE',  ( -74.76096257510376120, -290.2159045468530394, -333.1746417710294850 ) ) ;
#54410 = FACE_OUTER_BOUND ( 'NONE', #60128, .T. ) ;
#54411 = ORIENTED_EDGE ( 'NONE', *, *, #81790, .F. ) ;
#54412 = CARTESIAN_POINT ( 'NONE',  ( -55.86352057578385200, -289.9558712258774449, -196.8410936523945338 ) ) ;
#54413 = CARTESIAN_POINT ( 'NONE',  ( -46.13167228009177734, -298.2768267962699156, -193.8857580223321122 ) ) ;
#54414 = CARTESIAN_POINT ( 'NONE',  ( -109.1636984043707059, -296.0441523720942314, -283.6094826944226952 ) ) ;
#54415 = DIRECTION ( 'NONE',  ( -0.000000000000000000, -0.000000000000000000, -1.000000000000000000 ) ) ;
#54416 = CARTESIAN_POINT ( 'NONE',  ( 195.8632375102449146, 25.05079320569620904, 14.11692515535455783 ) ) ;
#54417 = CARTESIAN_POINT ( 'NONE',  ( -86.91913933143823101, -291.2473279656440468, -328.4372740890796081 ) ) ;
#54418 = CARTESIAN_POINT ( 'NONE',  ( -88.52914483777347243, -287.9090924074130839, -206.2264541496106460 ) ) ;
#54419 = CARTESIAN_POINT ( 'NONE',  ( -109.1439830577171222, -286.2796852825553060, -291.4890497068415129 ) ) ;
#54420 = CARTESIAN_POINT ( 'NONE',  ( -57.32733597892497812, -271.7936214747699069, -198.1918778335514446 ) ) ;
#54421 = CARTESIAN_POINT ( 'NONE',  ( -95.75765809036667520, -275.1107692989325528, -224.2212213932562008 ) ) ;
#54422 = CARTESIAN_POINT ( 'NONE',  ( 24.55187252496682859, -291.0687826493541479, -229.0029281984327838 ) ) ;
#54423 = CARTESIAN_POINT ( 'NONE',  ( -112.5372564876072943, -280.2894757188504400, -280.0454992716609581 ) ) ;
#54424 = ORIENTED_EDGE ( 'NONE', *, *, #76676, .T. ) ;
#54425 = CARTESIAN_POINT ( 'NONE',  ( 11.97935973491609651, -281.6930745809910945, -324.3178202716776468 ) ) ;
#54426 = CARTESIAN_POINT ( 'NONE',  ( 33.90222610867350994, -276.9950082340621407, -298.8908951164094674 ) ) ;
#54427 = CARTESIAN_POINT ( 'NONE',  ( 19.84255179703608363, -279.6523162412574948, -219.3711039045785185 ) ) ;
#54428 = CARTESIAN_POINT ( 'NONE',  ( 178.0273201536632257, 252.5904144576495014, -164.6784170649348766 ) ) ;
#54429 = CARTESIAN_POINT ( 'NONE',  ( 28.29512180978152358, -275.9710213066081792, -230.4521396472545405 ) ) ;
#54430 = CARTESIAN_POINT ( 'NONE',  ( -85.38682883930376022, -274.9218266514497486, -211.0789675660428770 ) ) ;
#54431 = EDGE_CURVE ( 'NONE', #64642, #47196, #13662, .T. ) ;
#54432 = CARTESIAN_POINT ( 'NONE',  ( 39.58706461736021254, -296.0519495502702512, -270.3284710469133074 ) ) ;
#54433 = ORIENTED_EDGE ( 'NONE', *, *, #34294, .T. ) ;
#54434 = DIRECTION ( 'NONE',  ( 1.000000000000000000, 0.000000000000000000, 0.000000000000000000 ) ) ;
#54435 = CARTESIAN_POINT ( 'NONE',  ( -101.9089116334536840, -291.1591002118069014, -305.1861577145047022 ) ) ;
#54436 = CARTESIAN_POINT ( 'NONE',  ( 37.78033276558921472, -289.1663350957921921, -258.8442455734470968 ) ) ;
#54437 = CARTESIAN_POINT ( 'NONE',  ( -108.5248306026289953, -290.1206457123464020, -253.6676062462082655 ) ) ;
#54438 = CARTESIAN_POINT ( 'NONE',  ( -37.97564309066880384, -285.5520647543452810, -193.4252679523327458 ) ) ;
#54439 = CARTESIAN_POINT ( 'NONE',  ( 200.8419735307467420, 26.78103457774644269, 10.49999999999999822 ) ) ;
#54440 = CARTESIAN_POINT ( 'NONE',  ( 36.31959538717714508, -279.8930026078488140, -265.8385129279841408 ) ) ;
#54441 = CARTESIAN_POINT ( 'NONE',  ( 36.78451083480545947, -289.3492861351845136, -265.4823095329641092 ) ) ;
#54442 = CARTESIAN_POINT ( 'NONE',  ( -59.17181237061875265, -281.8195986827554975, -340.8005201523357641 ) ) ;
#54443 = CARTESIAN_POINT ( 'NONE',  ( -102.6014456462129090, -280.3252169892650159, -236.4507699486624404 ) ) ;
#54444 = CARTESIAN_POINT ( 'NONE',  ( -36.45914523175086686, -277.5331807899437990, -343.4298037444884812 ) ) ;
#54445 = CARTESIAN_POINT ( 'NONE',  ( -104.8135185261363347, -288.8757164180376549, -306.6318009042486210 ) ) ;
#54446 = CARTESIAN_POINT ( 'NONE',  ( -65.82702165380304393, -286.4917062697573442, -198.9835192167049058 ) ) ;
#54447 = CARTESIAN_POINT ( 'NONE',  ( 26.30293161275466218, -287.4737865011771873, -227.1069514626154557 ) ) ;
#54448 = CARTESIAN_POINT ( 'NONE',  ( -101.7702292538398723, -284.2498290624740775, -304.7901875457919232 ) ) ;
#54449 = VERTEX_POINT ( 'NONE', #31024 ) ;
#54450 = CARTESIAN_POINT ( 'NONE',  ( 159.4851178187871312, 15.00000000000000000, -7.000000000000000888 ) ) ;
#54451 = CARTESIAN_POINT ( 'NONE',  ( -106.5925894201528337, -292.0124647025996296, -301.2247297463323434 ) ) ;
#54452 = CARTESIAN_POINT ( 'NONE',  ( 21.89410770461774192, -292.8913413935417225, -318.8008619264896311 ) ) ;
#54453 = CARTESIAN_POINT ( 'NONE',  ( -16.56246095852513633, -273.3859277990574697, -200.0826597055976777 ) ) ;
#54454 = ADVANCED_FACE ( 'NONE', ( #47531 ), #9085, .T. ) ;
#54455 = CARTESIAN_POINT ( 'NONE',  ( -36.28418253748976952, -294.3878474433843166, -347.2650000588765238 ) ) ;
#54456 = VECTOR ( 'NONE', #30538, 1000.000000000000000 ) ;
#54457 = CARTESIAN_POINT ( 'NONE',  ( -64.30745914991398138, -290.1736620626411423, -201.7649851151369944 ) ) ;
#54458 = CARTESIAN_POINT ( 'NONE',  ( -38.37866671362825599, -293.3051844867461568, -344.3671901427292141 ) ) ;
#54459 = CARTESIAN_POINT ( 'NONE',  ( -110.7024287695699343, -291.7102320630364716, -273.9435572138833095 ) ) ;
#54460 = CARTESIAN_POINT ( 'NONE',  ( 195.4781563537916043, 250.0000000000000568, 15.50000000000000000 ) ) ;
#54461 = CARTESIAN_POINT ( 'NONE',  ( 37.41094597726377913, -291.6590403484484000, -278.7169887414202094 ) ) ;
#54462 = VECTOR ( 'NONE', #12840, 1000.000000000000000 ) ;
#54463 = CARTESIAN_POINT ( 'NONE',  ( 32.07424567187151609, -295.1803830892341693, -241.8280986703765905 ) ) ;
#54464 = CARTESIAN_POINT ( 'NONE',  ( -10.62713326415700088, -289.6363320438476308, -338.6045173212468171 ) ) ;
#54465 = CARTESIAN_POINT ( 'NONE',  ( -41.13573637961724216, -275.9846464159625725, -195.0503442723845637 ) ) ;
#54466 = CARTESIAN_POINT ( 'NONE',  ( -20.22981193432151770, -275.6320915079082852, -345.0827602815496107 ) ) ;
#54467 = CARTESIAN_POINT ( 'NONE',  ( -105.1063686738797287, -296.2196952535776973, -234.0252365674405439 ) ) ;
#54468 = CARTESIAN_POINT ( 'NONE',  ( 33.05518132158856304, -274.0910608151258998, -293.2139754746388007 ) ) ;
#54469 = CARTESIAN_POINT ( 'NONE',  ( -8.670559923868280450, -278.5101322999274771, -201.6641026272448300 ) ) ;
#54470 = CARTESIAN_POINT ( 'NONE',  ( 0.8058092377127793471, -275.7784532944953639, -207.6562694148844912 ) ) ;
#54471 = CARTESIAN_POINT ( 'NONE',  ( -108.9915789874954868, -276.6192475293553343, -296.4527298158090503 ) ) ;
#54472 = EDGE_CURVE ( 'NONE', #2308, #13829, #83505, .T. ) ;
#54473 = DIRECTION ( 'NONE',  ( 0.000000000000000000, 0.000000000000000000, -1.000000000000000000 ) ) ;
#54474 = CARTESIAN_POINT ( 'NONE',  ( -57.96005601167394161, -298.5817182397422584, -200.1650701792778762 ) ) ;
#54475 = CARTESIAN_POINT ( 'NONE',  ( 180.7149167944524493, -12.49482340714361506, 13.00000000000000178 ) ) ;
#54477 = CARTESIAN_POINT ( 'NONE',  ( -59.47362139256243552, -273.5909040891444306, -200.7439959945896817 ) ) ;
#54476 = CARTESIAN_POINT ( 'NONE',  ( -72.43082167610883459, -287.5342421131651918, -337.0625941492019138 ) ) ;
#54478 = CARTESIAN_POINT ( 'NONE',  ( 27.44479758920837043, -288.0991780399880895, -312.0732463744585630 ) ) ;
#54479 = CARTESIAN_POINT ( 'NONE',  ( -78.12880367227818112, -289.2509574530789109, -335.7084934262737193 ) ) ;
#54480 = CARTESIAN_POINT ( 'NONE',  ( -92.81001138722074018, -275.2592177801483331, -219.6144523142734215 ) ) ;
#54481 = CARTESIAN_POINT ( 'NONE',  ( -94.49876758437574154, -293.8822009918490608, -318.6831317049116024 ) ) ;
#54482 = CARTESIAN_POINT ( 'NONE',  ( 38.70998244283266132, -280.8867824533791122, -281.3292718194990698 ) ) ;
#54483 = CYLINDRICAL_SURFACE ( 'NONE', #33572, 0.5000000000000000000 ) ;
#54484 = CARTESIAN_POINT ( 'NONE',  ( -109.5562099720875864, -276.2909298093215966, -290.6578354480366215 ) ) ;
#54485 = CARTESIAN_POINT ( 'NONE',  ( 201.4395141301528724, 287.8627056969148725, -5.175264492474406453 ) ) ;
#54486 = CARTESIAN_POINT ( 'NONE',  ( -98.62265046143760117, -289.9053918361510682, -229.8735844226685856 ) ) ;
#54487 = DIRECTION ( 'NONE',  ( 0.000000000000000000, 1.000000000000000000, 0.000000000000000000 ) ) ;
#54488 = CARTESIAN_POINT ( 'NONE',  ( 161.2244399300530233, -11.64849832608277325, 10.00000000000000000 ) ) ;
#54489 = CARTESIAN_POINT ( 'NONE',  ( -36.14946984881695613, -290.0669091128396531, -195.3577723839173359 ) ) ;
#54490 = CARTESIAN_POINT ( 'NONE',  ( -13.86269615307618253, -275.8825680621578158, -200.5080999809406137 ) ) ;
#54491 = CARTESIAN_POINT ( 'NONE',  ( 17.41678598021902857, -283.7143677768175962, -323.7294654170661374 ) ) ;
#54493 = CARTESIAN_POINT ( 'NONE',  ( -101.7712277623508186, -284.0831758459888761, -304.7883187367004894 ) ) ;
#54492 = CARTESIAN_POINT ( 'NONE',  ( -112.9007917339342129, -270.6681687357510100, -267.5228849028574700 ) ) ;
#54494 = CARTESIAN_POINT ( 'NONE',  ( -1.450986670879202078, -275.9632052979118271, -206.1031571055587790 ) ) ;
#54495 = CARTESIAN_POINT ( 'NONE',  ( -40.79276897210233699, -274.8106091891630740, -197.2312705246400526 ) ) ;
#54496 = CARTESIAN_POINT ( 'NONE',  ( 24.30143081559814533, -284.1319473691979738, -313.1051977790644401 ) ) ;
#54497 = CARTESIAN_POINT ( 'NONE',  ( -110.1914158896640572, -271.5801148496640849, -262.1669135185482560 ) ) ;
#54498 = ORIENTED_EDGE ( 'NONE', *, *, #53722, .F. ) ;
#54499 = DIRECTION ( 'NONE',  ( -0.5000000000000046629, 0.8660254037844359321, 0.000000000000000000 ) ) ;
#54500 = CARTESIAN_POINT ( 'NONE',  ( -32.01462874864632369, -294.8200442288518843, -347.1898808266892615 ) ) ;
#54501 = CARTESIAN_POINT ( 'NONE',  ( -111.1202223974959509, -286.3814913097627368, -282.0311711577576830 ) ) ;
#54502 = DIRECTION ( 'NONE',  ( 0.000000000000000000, 0.000000000000000000, -1.000000000000000000 ) ) ;
#54503 = CARTESIAN_POINT ( 'NONE',  ( -55.56934967048407970, -271.3380690714491266, -190.3538533559490702 ) ) ;
#54504 = CARTESIAN_POINT ( 'NONE',  ( -48.48070493199901421, -276.3875361728109965, -346.4417467637877053 ) ) ;
#54505 = CARTESIAN_POINT ( 'NONE',  ( -111.1522676921088504, -288.7120185491118605, -289.3458983780992071 ) ) ;
#54506 = CARTESIAN_POINT ( 'NONE',  ( -36.16321116965146132, -284.5572351284840806, -344.0450301899877559 ) ) ;
#54507 = CARTESIAN_POINT ( 'NONE',  ( -105.1914927648264921, -279.9186217476672596, -300.0593613551778844 ) ) ;
#54508 = CARTESIAN_POINT ( 'NONE',  ( -75.82577573433958662, -286.9745526073546671, -204.2881945408871331 ) ) ;
#54509 = CARTESIAN_POINT ( 'NONE',  ( 25.34042337187527494, -282.9954566652615995, -229.0855679903297073 ) ) ;
#54510 = CARTESIAN_POINT ( 'NONE',  ( 18.08812233331095243, -274.9863233189198013, -216.8380205676778871 ) ) ;
#54511 = CARTESIAN_POINT ( 'NONE',  ( -51.31470074704450468, -277.0594005603667256, -346.0826820062148386 ) ) ;
#54512 = CARTESIAN_POINT ( 'NONE',  ( -12.50519009885741539, -296.6469471360258012, -340.5899450461357674 ) ) ;
#54513 = DIRECTION ( 'NONE',  ( 0.000000000000000000, -1.000000000000000000, 0.000000000000000000 ) ) ;
#54514 = CARTESIAN_POINT ( 'NONE',  ( 223.4306832106270804, -134.2391364535880882, 22.50000000000000000 ) ) ;
#54515 = CIRCLE ( 'NONE', #78745, 0.5000000000000004441 ) ;
#54516 = CARTESIAN_POINT ( 'NONE',  ( -43.17070068259021554, -296.1190206143008368, -194.7685192277762951 ) ) ;
#54517 = CARTESIAN_POINT ( 'NONE',  ( -101.9142347688244428, -277.5945949126103187, -304.5426365495230243 ) ) ;
#54518 = CARTESIAN_POINT ( 'NONE',  ( -75.63752434942367131, -298.6336778810543251, -203.8552832132004937 ) ) ;
#54519 = AXIS2_PLACEMENT_3D ( 'NONE', #39930, #18643, #32851 ) ;
#54520 = CARTESIAN_POINT ( 'NONE',  ( -35.93639475293624486, -287.8301596497616401, -196.3611238416436038 ) ) ;
#54521 = CARTESIAN_POINT ( 'NONE',  ( -97.71393025181423297, -297.4436454701123012, -317.0291111367592407 ) ) ;
#54522 = CARTESIAN_POINT ( 'NONE',  ( -27.78209149001932943, -296.1385359950452880, -346.4182321894500092 ) ) ;
#54523 = CARTESIAN_POINT ( 'NONE',  ( -111.7995127460078066, -292.6486687502030577, -262.8736240630379939 ) ) ;
#54524 = CARTESIAN_POINT ( 'NONE',  ( -35.59509969697922571, -278.0739276924878709, -195.5354518844400218 ) ) ;
#54525 = CARTESIAN_POINT ( 'NONE',  ( -96.77595910661851519, -281.0899245823202364, -225.5193859641550773 ) ) ;
#54526 = CARTESIAN_POINT ( 'NONE',  ( -108.7630797693000204, -270.8553139343745215, -248.4855661378616105 ) ) ;
#54527 = CARTESIAN_POINT ( 'NONE',  ( -5.945400681139366483, -284.5042479926262899, -339.3145650658788668 ) ) ;
#54528 = CARTESIAN_POINT ( 'NONE',  ( 34.01435421217547628, -286.2509634147783686, -253.4979098905831165 ) ) ;
#54529 = CARTESIAN_POINT ( 'NONE',  ( -76.26301331016580320, -209.3917711165195499, -356.8240937122167225 ) ) ;
#54530 = ORIENTED_EDGE ( 'NONE', *, *, #16849, .F. ) ;
#54531 = CARTESIAN_POINT ( 'NONE',  ( -37.27659351975641755, -285.7196708280350776, -197.3275608611384371 ) ) ;
#54532 = ORIENTED_EDGE ( 'NONE', *, *, #20481, .T. ) ;
#54533 = CARTESIAN_POINT ( 'NONE',  ( -61.12270646156451903, -284.4333553756609945, -343.3271794767043730 ) ) ;
#54534 = CARTESIAN_POINT ( 'NONE',  ( -21.93370400848765911, -274.5883638998539027, -198.9840828644169903 ) ) ;
#54535 = CARTESIAN_POINT ( 'NONE',  ( 26.81363734757852768, -285.7943436032209661, -228.5030077566260047 ) ) ;
#54536 = CARTESIAN_POINT ( 'NONE',  ( -7.639133801106644306, -281.3733196298504708, -199.5614249559657765 ) ) ;
#54537 = CARTESIAN_POINT ( 'NONE',  ( 73.43068321062709458, -134.2391364535880598, 0.000000000000000000 ) ) ;
#54538 = CARTESIAN_POINT ( 'NONE',  ( -113.6908671728898241, -280.0564305816117212, -271.6164854738045733 ) ) ;
#54539 = CARTESIAN_POINT ( 'NONE',  ( 37.52879818320447214, -282.1099233519890959, -288.3101705966004715 ) ) ;
#54540 = CARTESIAN_POINT ( 'NONE',  ( -92.08974858914540107, -287.4094976428775112, -313.9805196606274080 ) ) ;
#54541 = CARTESIAN_POINT ( 'NONE',  ( -77.26738670498112072, -208.9735159622803167, -357.2724075973424647 ) ) ;
#54542 = ORIENTED_EDGE ( 'NONE', *, *, #21877, .T. ) ;
#54543 = CARTESIAN_POINT ( 'NONE',  ( -60.05576592190065810, -275.7573956509355071, -199.0039877813583189 ) ) ;
#54544 = CARTESIAN_POINT ( 'NONE',  ( -13.59065996674749499, -91.27732092402939656, -359.7254001870301181 ) ) ;
#54545 = CARTESIAN_POINT ( 'NONE',  ( 33.54640980252191440, -279.2668085063594390, -246.8159353152754534 ) ) ;
#54546 = CARTESIAN_POINT ( 'NONE',  ( 38.59504438108795910, -295.3471959517924006, -273.1151776711053003 ) ) ;
#54547 = CARTESIAN_POINT ( 'NONE',  ( -106.9689028769844157, -295.6038704980115313, -292.7948782161178656 ) ) ;
#54548 = CARTESIAN_POINT ( 'NONE',  ( -53.37037148213816806, -291.3596647568022604, -195.0563583117382791 ) ) ;
#54549 = DIRECTION ( 'NONE',  ( -0.000000000000000000, -1.000000000000000000, 0.000000000000000000 ) ) ;
#54551 = CARTESIAN_POINT ( 'NONE',  ( 36.45495667822554964, -285.9611860073666776, -271.0638677363292004 ) ) ;
#54550 = CARTESIAN_POINT ( 'NONE',  ( -96.95920022519082693, -294.4813783000894887, -318.1768096104395909 ) ) ;
#54552 = CARTESIAN_POINT ( 'NONE',  ( 15.74248330177986688, -294.6735020686085136, -218.3940209165518240 ) ) ;
#54553 = CARTESIAN_POINT ( 'NONE',  ( -110.8837751754803804, -285.8598831551734065, -270.9297172159879210 ) ) ;
#54554 = VERTEX_POINT ( 'NONE', #67932 ) ;
#54555 = CARTESIAN_POINT ( 'NONE',  ( 1.570458592538932496, -293.4998677468823871, -204.1289002139018578 ) ) ;
#54556 = CARTESIAN_POINT ( 'NONE',  ( -38.88009359107142870, -283.5642802192047043, -343.4189600977773011 ) ) ;
#54557 = CARTESIAN_POINT ( 'NONE',  ( -55.98855466317340301, -294.0820598187446535, -344.6598631497901124 ) ) ;
#54558 = CARTESIAN_POINT ( 'NONE',  ( -100.5419534657935685, -290.7766098925367828, -314.0633696249525997 ) ) ;
#54559 = CARTESIAN_POINT ( 'NONE',  ( -98.30335177756714415, -291.6715516409488487, -223.4014985039431451 ) ) ;
#54560 = CARTESIAN_POINT ( 'NONE',  ( -66.32707632853670532, -289.6090687285297918, -337.4139987518576618 ) ) ;
#54561 = ORIENTED_EDGE ( 'NONE', *, *, #34825, .F. ) ;
#54562 = CARTESIAN_POINT ( 'NONE',  ( 113.5000000000000568, -296.0521521680024080, -400.5374811273811702 ) ) ;
#54563 = CARTESIAN_POINT ( 'NONE',  ( -110.7656478456406290, -298.1743065953174892, -289.1011075472248990 ) ) ;
#54564 = CARTESIAN_POINT ( 'NONE',  ( -113.9440573844913445, -271.3831319911222977, -267.4931300989931060 ) ) ;
#54565 = CARTESIAN_POINT ( 'NONE',  ( -35.64537022646563003, -279.1326649175781540, -197.1330287555149710 ) ) ;
#54566 = ORIENTED_EDGE ( 'NONE', *, *, #90249, .T. ) ;
#54567 = CARTESIAN_POINT ( 'NONE',  ( -3.847224832576078946, -273.9898579218531722, -201.0815712984729942 ) ) ;
#54568 = CARTESIAN_POINT ( 'NONE',  ( -65.82296942945141893, -296.1525263929442531, -202.3940299736871395 ) ) ;
#54569 = CARTESIAN_POINT ( 'NONE',  ( -43.28271581739778640, -278.9883950154219292, -344.3582112572414076 ) ) ;
#54570 = CARTESIAN_POINT ( 'NONE',  ( 3.631105760235500135, -272.7489587030858047, -208.3957567974503320 ) ) ;
#54571 = CARTESIAN_POINT ( 'NONE',  ( -96.72066180132647162, -297.1564465682660625, -313.5249958836847668 ) ) ;
#54572 = CARTESIAN_POINT ( 'NONE',  ( -50.02083663284555115, -298.9662226655478321, -198.1567859083824032 ) ) ;
#54573 = CARTESIAN_POINT ( 'NONE',  ( 128.9960186029002500, -299.5541904835127980, -195.3611179825600175 ) ) ;
#54574 = CARTESIAN_POINT ( 'NONE',  ( -113.5654007414033373, -298.1256511623388405, -272.4682174214288466 ) ) ;
#54575 = CARTESIAN_POINT ( 'NONE',  ( -91.96220046314745389, -271.2974590167983706, -218.4288306385668932 ) ) ;
#54576 = CARTESIAN_POINT ( 'NONE',  ( 19.41969872385966411, -293.5525080588010383, -224.2757582449652034 ) ) ;
#54577 = CARTESIAN_POINT ( 'NONE',  ( -82.07293585013043469, -290.0036531682835630, -211.8629982991163274 ) ) ;
#54578 = CARTESIAN_POINT ( 'NONE',  ( 28.56507200901022259, -300.8773574837633760, -195.3386412410832236 ) ) ;
#54579 = CARTESIAN_POINT ( 'NONE',  ( 28.44667063823031938, -275.5221888306387541, -230.3667112173299643 ) ) ;
#54580 = CARTESIAN_POINT ( 'NONE',  ( -110.3417791297764268, -272.7547376145998896, -267.6393759378285608 ) ) ;
#54581 = CARTESIAN_POINT ( 'NONE',  ( -30.34203013114005287, -284.9439093263915197, -345.3905217009919966 ) ) ;
#54582 = CARTESIAN_POINT ( 'NONE',  ( -4.391495585576476124, -281.3117872631973455, -339.4231938077035124 ) ) ;
#54583 = CARTESIAN_POINT ( 'NONE',  ( -74.05549271712872894, -276.8753756295446351, -337.9439202656499788 ) ) ;
#54584 = CARTESIAN_POINT ( 'NONE',  ( 207.2843595876404095, 1.043152431597805130, -7.415392722555414373 ) ) ;
#54585 = CARTESIAN_POINT ( 'NONE',  ( -104.7423399430342101, -284.1319670707478622, -241.7747436285103504 ) ) ;
#54586 = CARTESIAN_POINT ( 'NONE',  ( 36.85399159966266325, -279.7073047883271215, -282.4841003916467344 ) ) ;
#54587 = EDGE_CURVE ( 'NONE', #30213, #63820, #40849, .T. ) ;
#54588 = CARTESIAN_POINT ( 'NONE',  ( 10.02960774911761277, -274.9588272284195227, -326.6757173817206876 ) ) ;
#54589 = CARTESIAN_POINT ( 'NONE',  ( -93.88263849894434543, -279.8681280282063994, -319.6562693588560364 ) ) ;
#54590 = CARTESIAN_POINT ( 'NONE',  ( 153.3663770037547636, 20.33084388956512001, 12.12609372516293327 ) ) ;
#54591 = CARTESIAN_POINT ( 'NONE',  ( -23.56584007183121443, -296.4622326768405287, -194.3785059543251634 ) ) ;
#54592 = AXIS2_PLACEMENT_3D ( 'NONE', #60711, #17620, #46471 ) ;
#54593 = CARTESIAN_POINT ( 'NONE',  ( -108.9130038549150754, -280.2545261918359643, -293.4975626544832039 ) ) ;
#54594 = CARTESIAN_POINT ( 'NONE',  ( 156.5440870305766055, 214.9910457053126720, 17.21343741151179429 ) ) ;
#54595 = CARTESIAN_POINT ( 'NONE',  ( -112.8879512033866064, -286.5126017952944153, -267.1995143589419399 ) ) ;
#54596 = VERTEX_POINT ( 'NONE', #31483 ) ;
#54597 = CARTESIAN_POINT ( 'NONE',  ( 200.5815643859949944, 65.97596549932491428, 9.780880230328994784 ) ) ;
#54598 = CARTESIAN_POINT ( 'NONE',  ( 32.55958156416060234, -285.1967721939885791, -243.0395010916681997 ) ) ;
#54599 = CARTESIAN_POINT ( 'NONE',  ( 155.2898987420118431, 20.78850644404472092, 13.36622507082863187 ) ) ;
#54600 = CARTESIAN_POINT ( 'NONE',  ( -69.91400815895589460, -294.2860004362561313, -336.1347848688370732 ) ) ;
#54601 = CARTESIAN_POINT ( 'NONE',  ( -2.812602291530306609, -286.7306254631795923, -336.1341462130840227 ) ) ;
#54602 = CARTESIAN_POINT ( 'NONE',  ( 84.09003387609358526, 83.72762891241104910, -302.5758382668069544 ) ) ;
#54603 = CARTESIAN_POINT ( 'NONE',  ( -110.2490798380144383, -294.3254077210424384, -288.0083783456177002 ) ) ;
#54604 = CARTESIAN_POINT ( 'NONE',  ( -93.39713546299613256, -283.7440794876658288, -218.5101955514913357 ) ) ;
#54605 = CARTESIAN_POINT ( 'NONE',  ( 36.36593196416949780, -283.2004539263394349, -274.0523758527202176 ) ) ;
#54606 = CARTESIAN_POINT ( 'NONE',  ( -41.53592186549863641, -281.3440171400004033, -346.2835830417213288 ) ) ;
#54607 = CARTESIAN_POINT ( 'NONE',  ( -97.34890827293364168, -289.9726988779725048, -311.9539219315899459 ) ) ;
#54608 = CARTESIAN_POINT ( 'NONE',  ( -85.88638354005971109, -280.7891551208682017, -215.0548016337999115 ) ) ;
#54609 = CARTESIAN_POINT ( 'NONE',  ( 32.12671149447684371, -282.0490845942538840, -247.2506649447183236 ) ) ;
#54610 = CARTESIAN_POINT ( 'NONE',  ( 37.34171039266468739, -289.4037437172542013, -260.3214468990019554 ) ) ;
#54611 = ORIENTED_EDGE ( 'NONE', *, *, #14110, .F. ) ;
#54612 = CARTESIAN_POINT ( 'NONE',  ( -41.19277030543477736, -274.0050740280257173, -193.4052220642227269 ) ) ;
#54613 = CARTESIAN_POINT ( 'NONE',  ( -102.5730536940850328, -293.0184948177988531, -233.9682917852116475 ) ) ;
#54614 = DIRECTION ( 'NONE',  ( 0.000000000000000000, 0.000000000000000000, 1.000000000000000000 ) ) ;
#54615 = CARTESIAN_POINT ( 'NONE',  ( -115.3430155898818299, -293.2662352645559167, -252.5904736702033517 ) ) ;
#54616 = EDGE_LOOP ( 'NONE', ( #29304, #11520, #92861, #36943, #71109, #11485, #43709, #35197, #37390, #58866, #25012 ) ) ;
#54617 = CARTESIAN_POINT ( 'NONE',  ( 22.88311951804342925, -274.1649601480243632, -315.3388850242654371 ) ) ;
#54618 = CARTESIAN_POINT ( 'NONE',  ( 236.4625231464875128, -138.0407542764614846, 21.50000000000000000 ) ) ;
#54619 = CARTESIAN_POINT ( 'NONE',  ( -34.90089267273180695, -293.4218464418098051, -346.5220192127906671 ) ) ;
#54620 = CARTESIAN_POINT ( 'NONE',  ( -92.08900282526985848, -272.5918949972167979, -221.9191370594037949 ) ) ;
#54621 = CARTESIAN_POINT ( 'NONE',  ( -70.26496703914455111, -291.0142479948054870, -336.3051166776849072 ) ) ;
#54622 = CARTESIAN_POINT ( 'NONE',  ( -21.14492922431972133, -284.6018066323541120, -342.6332344950658921 ) ) ;
#54623 = CARTESIAN_POINT ( 'NONE',  ( -104.1040333734418226, -292.4629509315023483, -233.1939664755869330 ) ) ;
#54624 = CARTESIAN_POINT ( 'NONE',  ( -30.75651725961395044, -293.4487808718054112, -194.0857768963367675 ) ) ;
#54625 = CARTESIAN_POINT ( 'NONE',  ( -60.25695242213713243, -291.5800842411453004, -200.9979695402869027 ) ) ;
#54626 = CARTESIAN_POINT ( 'NONE',  ( -106.4501065661208230, -286.9345089984053061, -241.0894222994657810 ) ) ;
#54627 = CARTESIAN_POINT ( 'NONE',  ( -50.94171455630022649, -280.0496404243696702, -194.5716753665946044 ) ) ;
#54628 = CARTESIAN_POINT ( 'NONE',  ( -99.55094671785275295, -295.2092901966221348, -227.4510513698674288 ) ) ;
#54629 = CARTESIAN_POINT ( 'NONE',  ( 13.67920063654869445, -282.1939826511066371, -328.1024246120642260 ) ) ;
#54630 = CARTESIAN_POINT ( 'NONE',  ( 36.93511906904098652, -277.4284133489766191, -271.5820317081910957 ) ) ;
#54631 = CARTESIAN_POINT ( 'NONE',  ( -85.33152481854864391, -299.9090924074131408, -210.2361428286349110 ) ) ;
#54632 = CARTESIAN_POINT ( 'NONE',  ( -41.34328506424762395, -275.2415879886764287, -346.0331711370850485 ) ) ;
#54633 = CARTESIAN_POINT ( 'NONE',  ( 175.2296996224749250, 250.5000000000000568, -29.99999999999998224 ) ) ;
#54634 = CARTESIAN_POINT ( 'NONE',  ( -58.97232724401461468, -282.8472079639431058, -340.2004394190266225 ) ) ;
#54635 = CARTESIAN_POINT ( 'NONE',  ( -112.0180984976857275, -279.9718339427403180, -253.2893797217364238 ) ) ;
#54636 = CARTESIAN_POINT ( 'NONE',  ( 36.55464456235706905, -286.8727627748725695, -291.1975255861840992 ) ) ;
#54637 = CARTESIAN_POINT ( 'NONE',  ( -34.84524596328733992, -293.8440848399874312, -196.3898956588212172 ) ) ;
#54638 = CARTESIAN_POINT ( 'NONE',  ( 26.98454783646936761, -277.6943517093479272, -311.3074249825961033 ) ) ;
#54639 = EDGE_CURVE ( 'NONE', #18590, #21234, #39354, .T. ) ;
#54640 = CARTESIAN_POINT ( 'NONE',  ( 30.80340306003076378, -276.4165085691404897, -235.5826306243239401 ) ) ;
#54642 = EDGE_CURVE ( 'NONE', #41118, #46033, #67, .T. ) ;
#54641 = CARTESIAN_POINT ( 'NONE',  ( -51.28296348307339514, -277.0687124877008500, -342.0175285858742882 ) ) ;
#54643 = CARTESIAN_POINT ( 'NONE',  ( -98.67165023545506131, -297.9690220861425018, -313.2407827136157152 ) ) ;
#54644 = CARTESIAN_POINT ( 'NONE',  ( -105.1358189119283963, -282.9708252718825179, -238.5526307209429433 ) ) ;
#54645 = CARTESIAN_POINT ( 'NONE',  ( -30.69486334076684741, -291.8005915636979353, -193.6170196874747944 ) ) ;
#54646 = CARTESIAN_POINT ( 'NONE',  ( -31.86373137704978831, -290.5843758170571505, -346.4159714253527795 ) ) ;
#54647 = CARTESIAN_POINT ( 'NONE',  ( 32.09825129800050547, -292.1596630215785808, -246.7015338297873939 ) ) ;
#54648 = ORIENTED_EDGE ( 'NONE', *, *, #10597, .F. ) ;
#54649 = CARTESIAN_POINT ( 'NONE',  ( -74.37729085691879050, -290.1442795661108676, -203.5257133468976747 ) ) ;
#54650 = CARTESIAN_POINT ( 'NONE',  ( 16.75670112267849277, -292.5156325405050097, -221.2415604654017045 ) ) ;
#54651 = EDGE_LOOP ( 'NONE', ( #8915, #47920, #91180, #89127 ) ) ;
#54652 = CARTESIAN_POINT ( 'NONE',  ( -1.931177007002584656, -289.6739066750046163, -338.3874905371809518 ) ) ;
#54653 = CARTESIAN_POINT ( 'NONE',  ( -102.1766101747465996, -279.3434821536083064, -236.6575792824504560 ) ) ;
#54654 = CARTESIAN_POINT ( 'NONE',  ( -102.0481846402981176, -296.0142337675970339, -229.1960433260148591 ) ) ;
#54655 = CARTESIAN_POINT ( 'NONE',  ( -1.025030557997025360, -287.1727521185500223, -202.5790237529462274 ) ) ;
#54656 = CARTESIAN_POINT ( 'NONE',  ( 37.48486602947158275, -288.1122165336381045, -288.4924709483038328 ) ) ;
#54657 = CARTESIAN_POINT ( 'NONE',  ( -109.2145940201805132, -285.0564676951663614, -257.3921248235521944 ) ) ;
#54658 = CARTESIAN_POINT ( 'NONE',  ( -71.48678950958364453, -195.9896530787580389, -360.3036401658270620 ) ) ;
#54659 = CARTESIAN_POINT ( 'NONE',  ( -108.2218527567996915, -260.4523294004561649, -316.5612791343883146 ) ) ;
#54660 = CARTESIAN_POINT ( 'NONE',  ( 5.250456697231451919, -59.01702808322732352, -350.9678742460372405 ) ) ;
#54661 = VECTOR ( 'NONE', #1618, 1000.000000000000000 ) ;
#54662 = CARTESIAN_POINT ( 'NONE',  ( -5.227969495918243226, -273.6831247920401893, -204.6105902164035228 ) ) ;
#54663 = CARTESIAN_POINT ( 'NONE',  ( -8.630232360692120963, -275.5876997396466663, -337.8274976556004390 ) ) ;
#54664 = CARTESIAN_POINT ( 'NONE',  ( -37.60115747517003371, -297.5566405813652295, -193.4230936677248565 ) ) ;
#54665 = CARTESIAN_POINT ( 'NONE',  ( 154.5266617868613253, 204.3775580378999450, -214.7585744442969542 ) ) ;
#54666 = CARTESIAN_POINT ( 'NONE',  ( 19.49951877326586924, -274.9367919269741947, -321.5898398927589596 ) ) ;
#54667 = CARTESIAN_POINT ( 'NONE',  ( -94.57608344790115495, -274.9681035542974428, -223.4136971311261561 ) ) ;
#54668 = CARTESIAN_POINT ( 'NONE',  ( 98.65582398152450594, -300.6570902592916354, -193.5751751503145215 ) ) ;
#54669 = AXIS2_PLACEMENT_3D ( 'NONE', #68948, #11638, #10225 ) ;
#54670 = CARTESIAN_POINT ( 'NONE',  ( -61.26925297919074609, -289.8637906923214018, -339.3934340103310205 ) ) ;
#54671 = CARTESIAN_POINT ( 'NONE',  ( -70.72844725851523151, -296.2840863250205530, -339.5816944499152328 ) ) ;
#54672 = CARTESIAN_POINT ( 'NONE',  ( -113.1421496568406013, -296.8757144146825340, -283.8460706129978917 ) ) ;
#54673 = CARTESIAN_POINT ( 'NONE',  ( -75.65624939782556169, -295.7453008960374063, -332.5569577960851007 ) ) ;
#54674 = ORIENTED_EDGE ( 'NONE', *, *, #9906, .F. ) ;
#54675 = CARTESIAN_POINT ( 'NONE',  ( -83.95839471173226798, -279.6066080095891948, -329.8935246980554439 ) ) ;
#54676 = ORIENTED_EDGE ( 'NONE', *, *, #60013, .F. ) ;
#54677 = CARTESIAN_POINT ( 'NONE',  ( 39.12234881275100662, -280.9471874417193931, -261.3633933933106164 ) ) ;
#54678 = CARTESIAN_POINT ( 'NONE',  ( 18.49555896795527943, -277.1650203342973668, -317.7489745004397150 ) ) ;
#54679 = CARTESIAN_POINT ( 'NONE',  ( -5.686213211836077974, -278.4016907416234403, -339.4400884786396091 ) ) ;
#54680 = CARTESIAN_POINT ( 'NONE',  ( -83.87101026556891270, -275.7071893048811830, -329.7016322165442830 ) ) ;
#54681 = CARTESIAN_POINT ( 'NONE',  ( -64.59756155679460221, -274.1788316492083482, -202.5604116328183579 ) ) ;
#54682 = CARTESIAN_POINT ( 'NONE',  ( -41.88674800110077712, -296.5684808699012933, -196.9123776421947696 ) ) ;
#54683 = CARTESIAN_POINT ( 'NONE',  ( 175.2296996224750103, 133.0000000000000000, 0.000000000000000000 ) ) ;
#54684 = CARTESIAN_POINT ( 'NONE',  ( -108.4857863948629131, -278.5023390013022890, -286.7725164683772050 ) ) ;
#54685 = CARTESIAN_POINT ( 'NONE',  ( -29.04739533227477821, -287.6340839070055040, -346.4702190549190277 ) ) ;
#54686 = CARTESIAN_POINT ( 'NONE',  ( -84.56910444423637330, -275.4017879252262446, -212.0981543848764090 ) ) ;
#54687 = CARTESIAN_POINT ( 'NONE',  ( 195.7226947101956682, 20.87406718349393486, -14.32264105795935372 ) ) ;
#54688 = CARTESIAN_POINT ( 'NONE',  ( -110.4062734849154168, -289.8104668481442445, -265.7151985562770733 ) ) ;
#54689 = CARTESIAN_POINT ( 'NONE',  ( -97.09843596767852603, -283.2505527954193667, -318.7806284116109055 ) ) ;
#54690 = CARTESIAN_POINT ( 'NONE',  ( 32.94590736020091271, -279.4865240379141369, -247.0126652185127796 ) ) ;
#54692 = CARTESIAN_POINT ( 'NONE',  ( -88.67008483207021641, -283.4048497679304432, -216.4471947362969217 ) ) ;
#54691 = CARTESIAN_POINT ( 'NONE',  ( 15.69655556348369885, -279.3955606098330691, -219.2753789985103481 ) ) ;
#54693 = CARTESIAN_POINT ( 'NONE',  ( -6.530856881225692412, -288.4568769625128084, -201.9682219244134274 ) ) ;
#54694 = CARTESIAN_POINT ( 'NONE',  ( -77.04950660590047562, -280.7125181827636311, -208.5719192289845694 ) ) ;
#54695 = CARTESIAN_POINT ( 'NONE',  ( 196.7383257810085979, 24.47698789593438917, 11.00000000000000000 ) ) ;
#54696 = CARTESIAN_POINT ( 'NONE',  ( -52.99736190476249931, -293.8517713645351819, -196.9602246445333549 ) ) ;
#54697 = CARTESIAN_POINT ( 'NONE',  ( -112.7633383177375208, -276.6695023354861291, -280.0280531230036445 ) ) ;
#54698 = CARTESIAN_POINT ( 'NONE',  ( 30.37558207583533942, -276.5735138454250546, -298.0324111229830919 ) ) ;
#54699 = CARTESIAN_POINT ( 'NONE',  ( -3.690198383856922781, -284.6093846445712074, -337.5885544258872528 ) ) ;
#54700 = CARTESIAN_POINT ( 'NONE',  ( 196.2775035532951335, 71.85522536017060702, 11.57408223790024060 ) ) ;
#54701 = CARTESIAN_POINT ( 'NONE',  ( -110.5211717831488158, -292.2317317432538175, -289.2298020476632132 ) ) ;
#54702 = CARTESIAN_POINT ( 'NONE',  ( -109.3255128253985333, -294.2787991223954123, -291.5952737804996673 ) ) ;
#54703 = CARTESIAN_POINT ( 'NONE',  ( 20.17269628375615298, -286.0569673430740636, -219.3291220171019802 ) ) ;
#54704 = CARTESIAN_POINT ( 'NONE',  ( -107.3235106087011985, -289.2598391952108727, -246.9306545490687483 ) ) ;
#54705 = CARTESIAN_POINT ( 'NONE',  ( 175.2296996224750103, 249.5000000000000568, -12.00000000000000000 ) ) ;
#54706 = CARTESIAN_POINT ( 'NONE',  ( 35.87106203721491227, -274.1456349666021310, -263.3905188740209837 ) ) ;
#54707 = CARTESIAN_POINT ( 'NONE',  ( -73.93151162947731336, -293.6832694069670993, -334.9525351786377882 ) ) ;
#54708 = DIRECTION ( 'NONE',  ( -0.6421047760857900855, 0.000000000000000000, -0.7666168903225504261 ) ) ;
#54709 = CARTESIAN_POINT ( 'NONE',  ( -30.73780285809773716, -290.6139422068088152, -194.2884671063692110 ) ) ;
#54710 = CARTESIAN_POINT ( 'NONE',  ( -22.31665797051880062, -287.8477652845519401, -198.0543397047241569 ) ) ;
#54711 = CARTESIAN_POINT ( 'NONE',  ( 13.90356462351033962, -286.5852925128036759, -326.5385220232933534 ) ) ;
#54712 = CARTESIAN_POINT ( 'NONE',  ( -110.6815248929286639, -285.8982147470362634, -276.4146309748921340 ) ) ;
#54713 = DIRECTION ( 'NONE',  ( 0.000000000000000000, 0.000000000000000000, -1.000000000000000000 ) ) ;
#54714 = CARTESIAN_POINT ( 'NONE',  ( -11.97556138708707252, -287.1937924593620437, -201.7377929952737645 ) ) ;
#54715 = CARTESIAN_POINT ( 'NONE',  ( 33.93896361373181492, -295.8486607460680489, -294.9644553570703351 ) ) ;
#54716 = CARTESIAN_POINT ( 'NONE',  ( -67.16321444335588353, -275.5199345788036567, -339.7872764816617064 ) ) ;
#54717 = VECTOR ( 'NONE', #15928, 1000.000000000000000 ) ;
#54718 = CARTESIAN_POINT ( 'NONE',  ( 39.68627834990948600, -275.8955164503840933, -271.1671843719709614 ) ) ;
#54719 = AXIS2_PLACEMENT_3D ( 'NONE', #47364, #46897, #75798 ) ;
#54720 = CARTESIAN_POINT ( 'NONE',  ( -67.72683166957153844, -289.7364111817677212, -201.1656808762559763 ) ) ;
#54721 = CARTESIAN_POINT ( 'NONE',  ( -104.7935864188600590, -279.0331759875775788, -233.2229565335078973 ) ) ;
#54722 = CARTESIAN_POINT ( 'NONE',  ( -110.7553187964862502, -298.3569519150567544, -283.9331817824998438 ) ) ;
#54723 = CARTESIAN_POINT ( 'NONE',  ( -48.18343439339474088, -249.7038996752085040, -482.2249225752359507 ) ) ;
#54724 = DIRECTION ( 'NONE',  ( -1.000000000000000000, 0.000000000000000000, 0.000000000000000000 ) ) ;
#54725 = CARTESIAN_POINT ( 'NONE',  ( -109.1616785944288210, -276.9361692062703355, -251.5294449828613494 ) ) ;
#54726 = CARTESIAN_POINT ( 'NONE',  ( 14.35601586795831075, -280.3251422878600465, -324.6966202592768695 ) ) ;
#54727 = CARTESIAN_POINT ( 'NONE',  ( 169.9462594094670180, 250.0000000000000568, -23.92352941176469727 ) ) ;
#54728 = CARTESIAN_POINT ( 'NONE',  ( 33.08122092260052227, -273.6534324041895729, -240.8422559923055246 ) ) ;
#54729 = VECTOR ( 'NONE', #61615, 1000.000000000000000 ) ;
#54730 = CARTESIAN_POINT ( 'NONE',  ( 33.01444932175722613, -295.3600823442710634, -292.2864455125696281 ) ) ;
#54731 = CARTESIAN_POINT ( 'NONE',  ( -52.86852594743199063, -282.1668471298895611, -345.5180576599705660 ) ) ;
#54732 = CARTESIAN_POINT ( 'NONE',  ( -75.77135397721518473, -296.5197479846367514, -332.7625980591599841 ) ) ;
#54733 = CARTESIAN_POINT ( 'NONE',  ( -112.9051400078289760, -298.0191312508962937, -258.3003318703342757 ) ) ;
#54734 = CARTESIAN_POINT ( 'NONE',  ( -71.66312347702996988, -297.4186680807770813, -205.9183559838716064 ) ) ;
#54735 = CARTESIAN_POINT ( 'NONE',  ( -16.91160945744981703, -294.3160089787164111, -198.1433045205163239 ) ) ;
#54736 = CARTESIAN_POINT ( 'NONE',  ( 25.85292341809120842, -288.3012346597075179, -314.4463002195279273 ) ) ;
#54737 = CARTESIAN_POINT ( 'NONE',  ( 19.87168363016981232, -274.3740997330951927, -320.0489872838214183 ) ) ;
#54738 = CARTESIAN_POINT ( 'NONE',  ( 7.932796896963242084, -288.2861002955175991, -332.7102519098718290 ) ) ;
#54739 = CARTESIAN_POINT ( 'NONE',  ( 3.736705292930350808, -287.5433014349188170, -331.0520649069931665 ) ) ;
#54740 = CARTESIAN_POINT ( 'NONE',  ( -71.24479340915372916, -289.6044789287073513, -203.4471172219620314 ) ) ;
#54741 = EDGE_LOOP ( 'NONE', ( #78676, #45446, #63676, #22895 ) ) ;
#54742 = CARTESIAN_POINT ( 'NONE',  ( 165.2494399300530290, 8.542400036368780647, -9.000000000000001776 ) ) ;
#54743 = CARTESIAN_POINT ( 'NONE',  ( -48.07621344458673462, -288.6999170863115296, -342.6808395879009481 ) ) ;
#54744 = CARTESIAN_POINT ( 'NONE',  ( 207.8987101828041375, 29.19759012196911740, 13.45150321557463791 ) ) ;
#54745 = CARTESIAN_POINT ( 'NONE',  ( -108.8138128260671778, -285.8511689784494365, -242.2065480276230005 ) ) ;
#54746 = CARTESIAN_POINT ( 'NONE',  ( 36.06549682462953399, -292.3280940366882419, -247.9066385060554296 ) ) ;
#54747 = CARTESIAN_POINT ( 'NONE',  ( 25.60810134203713062, -282.5789186198248899, -227.3300239028076817 ) ) ;
#54748 = ADVANCED_FACE ( 'NONE', ( #60371 ), #52970, .T. ) ;
#54749 = CARTESIAN_POINT ( 'NONE',  ( -56.44978138196967876, -281.1262038345006431, -196.2242182885780721 ) ) ;
#54750 = CARTESIAN_POINT ( 'NONE',  ( -6.034869767349240632, -282.4622373114829088, -336.3209247320178292 ) ) ;
#54751 = CARTESIAN_POINT ( 'NONE',  ( -4.158893940830177272, -278.6149089234165785, -337.6353494535044888 ) ) ;
#54752 = CARTESIAN_POINT ( 'NONE',  ( -104.6029043052289040, -296.0649866144757993, -307.9525183963800146 ) ) ;
#54753 = CARTESIAN_POINT ( 'NONE',  ( -108.1231437001084288, -288.8801366316544659, -246.6580791891732645 ) ) ;
#54754 = CARTESIAN_POINT ( 'NONE',  ( -66.93155183245974627, -296.5753386398526459, -203.2752804489637413 ) ) ;
#54755 = VERTEX_POINT ( 'NONE', #18198 ) ;
#54756 = ORIENTED_EDGE ( 'NONE', *, *, #53943, .T. ) ;
#54757 = CARTESIAN_POINT ( 'NONE',  ( 139.6539576904058606, 275.0000000000000568, 10.50000000000000000 ) ) ;
#54758 = CARTESIAN_POINT ( 'NONE',  ( -109.4828344749282252, -286.2347031585719037, -288.7178861071425899 ) ) ;
#54759 = CARTESIAN_POINT ( 'NONE',  ( 17.35078598243592296, -295.3735180503437050, -324.1974729756229863 ) ) ;
#54760 = CARTESIAN_POINT ( 'NONE',  ( -83.71893170564314346, -286.0477156260857328, -213.7883059166572082 ) ) ;
#54761 = CARTESIAN_POINT ( 'NONE',  ( -6.679727891003104823, -275.7181059702332391, -340.7504931163030051 ) ) ;
#54762 = CARTESIAN_POINT ( 'NONE',  ( -90.72115765071453097, -291.9708459888942684, -214.9342829792792315 ) ) ;
#54763 = CARTESIAN_POINT ( 'NONE',  ( -62.76430338365177164, -283.8642871386332445, -198.9888774174734749 ) ) ;
#54764 = CARTESIAN_POINT ( 'NONE',  ( 23.95581675014300416, -293.2644875331943126, -223.7737893877462909 ) ) ;
#54765 = CARTESIAN_POINT ( 'NONE',  ( -68.76323214346719226, -289.8102807075879355, -336.2760238285457035 ) ) ;
#54766 = B_SPLINE_CURVE_WITH_KNOTS ( 'NONE', 3,
 ( #12579, #92555, #77921, #91628, #5945, #34356, #32940, #26781 ),
 .UNSPECIFIED., .F., .F.,
 ( 4, 2, 2, 4 ),
 ( 0.000000000000000000, 0.0004363303908676402477, 0.0008726607817352804953, 0.001745321563470476857 ),
 .UNSPECIFIED. ) ;
#54767 = CARTESIAN_POINT ( 'NONE',  ( 202.9738562182569694, 293.9636489450776367, -54.00000000000000000 ) ) ;
#54768 = LINE ( 'NONE', #45791, #88600 ) ;
#54769 = CARTESIAN_POINT ( 'NONE',  ( -88.26448419966551739, -229.6996826356688359, -344.4427272830038760 ) ) ;
#54770 = CARTESIAN_POINT ( 'NONE',  ( -91.92415337550016829, -285.3341001775988843, -323.6852546341170864 ) ) ;
#54771 = CARTESIAN_POINT ( 'NONE',  ( -114.2704648735229114, -282.0523547857346784, -270.3284710469133074 ) ) ;
#54772 = ORIENTED_EDGE ( 'NONE', *, *, #29167, .F. ) ;
#54773 = CARTESIAN_POINT ( 'NONE',  ( 35.73595927994151822, -280.5569496626930004, -276.7918812229924015 ) ) ;
#54774 = CARTESIAN_POINT ( 'NONE',  ( -2.738418744867219257, -276.2740244478974887, -339.1388427879324468 ) ) ;
#54775 = CARTESIAN_POINT ( 'NONE',  ( -57.63422218619935222, -281.7897016551495994, -198.3316658654249807 ) ) ;
#54776 = CARTESIAN_POINT ( 'NONE',  ( -107.0711107231528842, -266.7388540463169875, -306.2465019403078372 ) ) ;
#54777 = CARTESIAN_POINT ( 'NONE',  ( 36.03897685995190869, -279.8571293983528676, -249.0096524390684749 ) ) ;
#54778 = CARTESIAN_POINT ( 'NONE',  ( -82.45301188824893757, -283.4527504973215173, -210.8899791761965616 ) ) ;
#54779 = CARTESIAN_POINT ( 'NONE',  ( 96.93211984402050518, -301.4714976373853119, -194.3347991198949956 ) ) ;
#54780 = CARTESIAN_POINT ( 'NONE',  ( -97.23022912848335864, -296.4614522508908294, -312.2102820830003225 ) ) ;
#54781 = ORIENTED_EDGE ( 'NONE', *, *, #57468, .F. ) ;
#54782 = CARTESIAN_POINT ( 'NONE',  ( -30.74614965458419036, -290.8220931753748459, -197.1645183896307572 ) ) ;
#54783 = CARTESIAN_POINT ( 'NONE',  ( -48.47102471743825447, -277.8415477745168687, -346.5033817274929220 ) ) ;
#54784 = CARTESIAN_POINT ( 'NONE',  ( 35.64290476491508031, -275.5323758985769018, -268.8619686860586739 ) ) ;
#54785 = CARTESIAN_POINT ( 'NONE',  ( 2.270159155090923253, -273.4900990414959097, -204.6923041232815024 ) ) ;
#54786 = DIRECTION ( 'NONE',  ( 0.000000000000000000, 0.000000000000000000, 1.000000000000000000 ) ) ;
#54787 = CARTESIAN_POINT ( 'NONE',  ( -11.83557922115861949, -272.3838909394409598, -199.7769930510949905 ) ) ;
#54788 = CARTESIAN_POINT ( 'NONE',  ( 85.55100297371598117, -296.0521521680024080, -417.1172536214571096 ) ) ;
#54789 = AXIS2_PLACEMENT_3D ( 'NONE', #39421, #88230, #23386 ) ;
#54790 = DIRECTION ( 'NONE',  ( -1.000000000000000000, 0.000000000000000000, 0.000000000000000000 ) ) ;
#54791 = AXIS2_PLACEMENT_3D ( 'NONE', #3148, #17373, #32030 ) ;
#54792 = CARTESIAN_POINT ( 'NONE',  ( 3.574097049783933500, -283.5674610968012530, -331.2511711115135427 ) ) ;
#54793 = CARTESIAN_POINT ( 'NONE',  ( 22.61733212670093351, -283.9443848728290050, -317.0607173630778561 ) ) ;
#54794 = CARTESIAN_POINT ( 'NONE',  ( -94.19609121023967191, -284.5498958438442969, -224.3905375875953041 ) ) ;
#54795 = CARTESIAN_POINT ( 'NONE',  ( -74.43278093372407511, -275.9541996346974315, -334.1630939716773696 ) ) ;
#54796 = CARTESIAN_POINT ( 'NONE',  ( -37.52009564963651655, -284.9148594880118708, -344.6087466678422970 ) ) ;
#54797 = CARTESIAN_POINT ( 'NONE',  ( -64.60750629945529511, -275.8944384777469168, -338.8790562822850916 ) ) ;
#54798 = DIRECTION ( 'NONE',  ( -1.000000000000000000, -0.000000000000000000, -0.000000000000000000 ) ) ;
#54799 = CARTESIAN_POINT ( 'NONE',  ( 23.30033620924232807, -276.0611079736791567, -229.1467452166400562 ) ) ;
#54800 = AXIS2_PLACEMENT_3D ( 'NONE', #59576, #29757, #67602 ) ;
#54801 = CARTESIAN_POINT ( 'NONE',  ( 196.9906426852887193, 73.09784627861046147, -12.30894099459319513 ) ) ;
#54802 = CIRCLE ( 'NONE', #66915, 0.5000000000000004441 ) ;
#54803 = CARTESIAN_POINT ( 'NONE',  ( -92.96394086728045636, -280.0819476193443620, -217.2725849413230321 ) ) ;
#54804 = EDGE_LOOP ( 'NONE', ( #25543, #52432, #71585, #74255 ) ) ;
#54805 = DIRECTION ( 'NONE',  ( 0.000000000000000000, 0.000000000000000000, -1.000000000000000000 ) ) ;
#54806 = CARTESIAN_POINT ( 'NONE',  ( -65.44162544547695859, -287.5491189129509166, -199.9859797679958433 ) ) ;
#54807 = CARTESIAN_POINT ( 'NONE',  ( -78.04805593058895852, -294.8116770066197319, -331.2137146232465170 ) ) ;
#54808 = CARTESIAN_POINT ( 'NONE',  ( -74.38550402990404109, -288.8800144851840059, -337.7636094896698182 ) ) ;
#54809 = CARTESIAN_POINT ( 'NONE',  ( 21.15514057784789514, -285.1621201716123437, -225.0169491875583390 ) ) ;
#54811 = CARTESIAN_POINT ( 'NONE',  ( -109.6575680285130971, -288.5862398488591793, -286.1804893596330430 ) ) ;
#54810 = CARTESIAN_POINT ( 'NONE',  ( 22.48110275398108016, -285.5316811332732527, -227.4195240120962467 ) ) ;
#54812 = CARTESIAN_POINT ( 'NONE',  ( -103.8517444957814888, -286.1755457617657044, -239.1995692458752387 ) ) ;
#54813 = CARTESIAN_POINT ( 'NONE',  ( 21.92161414251100737, -274.1823983569975098, -316.3477975349532016 ) ) ;
#54814 = CARTESIAN_POINT ( 'NONE',  ( 19.70156358983043532, -285.2598003058698737, -219.7608652349659337 ) ) ;
#54815 = CARTESIAN_POINT ( 'NONE',  ( -35.90254134505045158, -300.0703241510347539, -195.3606186102793174 ) ) ;
#54816 = CARTESIAN_POINT ( 'NONE',  ( 35.01258594108399791, -285.8140253493967293, -290.7770059657278807 ) ) ;
#54817 = CARTESIAN_POINT ( 'NONE',  ( -37.01928345502811624, -280.9975414598524708, -197.1265325981078718 ) ) ;
#54818 = CARTESIAN_POINT ( 'NONE',  ( 2.236991035479711787, -290.5239512990511912, -334.3248930398124799 ) ) ;
#54819 = DIRECTION ( 'NONE',  ( -0.000000000000000000, -0.000000000000000000, -1.000000000000000000 ) ) ;
#54820 = DIRECTION ( 'NONE',  ( 0.000000000000000000, 0.000000000000000000, 1.000000000000000000 ) ) ;
#54821 = CARTESIAN_POINT ( 'NONE',  ( -76.31807526952506748, -297.4886794633707723, -335.1533949307752778 ) ) ;
#54822 = CARTESIAN_POINT ( 'NONE',  ( -41.12734230361837007, -278.0043305825820994, -195.4567151489958974 ) ) ;
#54823 = CARTESIAN_POINT ( 'NONE',  ( 6.412687804880273568, -291.8273387019003167, -207.1969481020532555 ) ) ;
#54824 = CARTESIAN_POINT ( 'NONE',  ( -95.91167455816636789, -295.5770976640273489, -225.4406616544906967 ) ) ;
#54825 = CARTESIAN_POINT ( 'NONE',  ( 35.91915802245630118, -280.3214849789204663, -276.8109756124551950 ) ) ;
#54826 = CARTESIAN_POINT ( 'NONE',  ( 30.40655649460581245, -273.2227079598729347, -239.3901362487319204 ) ) ;
#54827 = CARTESIAN_POINT ( 'NONE',  ( 34.81170932346955738, -295.0503653960419115, -284.3299756189863956 ) ) ;
#54828 = CARTESIAN_POINT ( 'NONE',  ( -54.42813229853332757, -297.7662352645559167, -345.3683826091709648 ) ) ;
#54829 = CARTESIAN_POINT ( 'NONE',  ( -110.9480689593987677, -295.2885518450696054, -250.0461612900226100 ) ) ;
#54830 = CARTESIAN_POINT ( 'NONE',  ( 0.02243465603823597068, -292.8018751581251422, -336.5417622517857126 ) ) ;
#54831 = CARTESIAN_POINT ( 'NONE',  ( -108.2890523582798608, -291.7190814596109476, -290.0896631170522255 ) ) ;
#54832 = DIRECTION ( 'NONE',  ( 0.000000000000000000, 0.000000000000000000, -1.000000000000000000 ) ) ;
#54833 = CARTESIAN_POINT ( 'NONE',  ( -37.56067507498378433, -292.8522121039181343, -197.1874975497974276 ) ) ;
#54834 = DIRECTION ( 'NONE',  ( 0.000000000000000000, 1.000000000000000000, 0.000000000000000000 ) ) ;
#54836 = CARTESIAN_POINT ( 'NONE',  ( 22.58793393945703798, -292.9709258747196259, -228.6564952919479481 ) ) ;
#54835 = CARTESIAN_POINT ( 'NONE',  ( -68.52923924434824698, -281.4800017822921063, -338.9736539246545135 ) ) ;
#54837 = CARTESIAN_POINT ( 'NONE',  ( -35.33602872409019113, -280.0766431042238764, -193.3741071519398815 ) ) ;
#54838 = CARTESIAN_POINT ( 'NONE',  ( -63.90870195292774980, -283.0560537942198494, -342.6102612683880011 ) ) ;
#54839 = CARTESIAN_POINT ( 'NONE',  ( -59.24958166259710879, -287.3360734146154414, -341.9699411778946683 ) ) ;
#54840 = CARTESIAN_POINT ( 'NONE',  ( 195.7510731661265595, -143.7221692137691775, 21.50000000000000000 ) ) ;
#54841 = CARTESIAN_POINT ( 'NONE',  ( -69.65103336461976369, -278.1144435353747326, -201.2178877335352354 ) ) ;
#54842 = CARTESIAN_POINT ( 'NONE',  ( 25.59014520486699240, -287.0550844105828219, -314.2823501210327208 ) ) ;
#54843 = DIRECTION ( 'NONE',  ( 0.000000000000000000, 0.000000000000000000, 1.000000000000000000 ) ) ;
#54844 = CARTESIAN_POINT ( 'NONE',  ( 35.50030252792328156, -294.9965954621784476, -258.4296724919660164 ) ) ;
#54845 = CARTESIAN_POINT ( 'NONE',  ( -56.75665513531810547, -278.7228511356416334, -344.3188293972524434 ) ) ;
#54846 = CARTESIAN_POINT ( 'NONE',  ( -81.29722343276812069, -279.1027718753659883, -211.9881145877385507 ) ) ;
#54847 = CARTESIAN_POINT ( 'NONE',  ( 39.23730353364649659, -293.8255316677272617, -278.8927593026595559 ) ) ;
#54848 = CARTESIAN_POINT ( 'NONE',  ( -89.46287041735449463, -281.8589296416707271, -325.1384387384256911 ) ) ;
#54849 = EDGE_CURVE ( 'NONE', #52994, #24040, #75686, .T. ) ;
#54850 = CARTESIAN_POINT ( 'NONE',  ( 21.18905228942488961, -291.9947771703691615, -226.3434002977374462 ) ) ;
#54851 = CIRCLE ( 'NONE', #14063, 25.50000000000000355 ) ;
#54852 = CARTESIAN_POINT ( 'NONE',  ( -103.4776497130817887, -295.0225600436410787, -234.8810185756578335 ) ) ;
#54853 = ORIENTED_EDGE ( 'NONE', *, *, #3472, .T. ) ;
#54854 = DIRECTION ( 'NONE',  ( -0.000000000000000000, -0.000000000000000000, -1.000000000000000000 ) ) ;
#54855 = AXIS2_PLACEMENT_3D ( 'NONE', #49567, #27812, #85550 ) ;
#54856 = CARTESIAN_POINT ( 'NONE',  ( 16.19997211966036588, -293.7737300012386186, -320.0730659892619201 ) ) ;
#54857 = CARTESIAN_POINT ( 'NONE',  ( 206.6110726073805210, 0.01288801604375346306, -7.290233312756247308 ) ) ;
#54858 = CARTESIAN_POINT ( 'NONE',  ( -53.28691492658257545, -289.3380690714490129, -200.3538533559491555 ) ) ;
#54859 = CARTESIAN_POINT ( 'NONE',  ( -113.3829859678191383, -271.8922269560968061, -258.9585404145392431 ) ) ;
#54860 = CARTESIAN_POINT ( 'NONE',  ( 14.33642407780962458, -278.9084983517965384, -214.8847126262412530 ) ) ;
#54861 = CIRCLE ( 'NONE', #6498, 21.95310499597075804 ) ;
#54862 = CARTESIAN_POINT ( 'NONE',  ( 9.495554926013772601, -287.9963515147975954, -209.8667396451806155 ) ) ;
#54863 = CARTESIAN_POINT ( 'NONE',  ( 20.35615608039524460, -288.0155285575916082, -315.1022395295304932 ) ) ;
#54864 = AXIS2_PLACEMENT_3D ( 'NONE', #32398, #83029, #55582 ) ;
#54865 = CARTESIAN_POINT ( 'NONE',  ( -39.15560843221825849, -278.5954508057097314, -344.0321264650893340 ) ) ;
#54866 = CARTESIAN_POINT ( 'NONE',  ( -107.3396433796828973, -294.9120854657339237, -244.2866028964509724 ) ) ;
#54867 = CARTESIAN_POINT ( 'NONE',  ( -86.79376813557587411, -299.1131192690993998, -215.2932781742513555 ) ) ;
#54868 = CARTESIAN_POINT ( 'NONE',  ( -97.21846944380278899, -276.7573155943226766, -312.8317798170293713 ) ) ;
#54869 = EDGE_LOOP ( 'NONE', ( #13888, #76823, #93003, #92775 ) ) ;
#54870 = CARTESIAN_POINT ( 'NONE',  ( -35.46828848052000183, -297.7417277859903493, -193.3823643072163634 ) ) ;
#54871 = CARTESIAN_POINT ( 'NONE',  ( -61.70364572987922003, -291.2913674300612570, -340.7017876074841638 ) ) ;
#54872 = CARTESIAN_POINT ( 'NONE',  ( 38.42833708171294660, -295.0440275860132715, -261.7953929749143640 ) ) ;
#54873 = CARTESIAN_POINT ( 'NONE',  ( 202.9738562182569694, 291.9636489450776367, -53.99999999998589573 ) ) ;
#54874 = EDGE_CURVE ( 'NONE', #28339, #32344, #37881, .T. ) ;
#54875 = CARTESIAN_POINT ( 'NONE',  ( -105.8090278388222174, -291.5465239389963585, -244.6026428687626151 ) ) ;
#54876 = CARTESIAN_POINT ( 'NONE',  ( -43.53958015783998547, -248.2612498862057180, -461.0541023492486943 ) ) ;
#54877 = VERTEX_POINT ( 'NONE', #39950 ) ;
#54878 = CARTESIAN_POINT ( 'NONE',  ( -101.4692718031482741, -297.7627846410916277, -227.8993312254676766 ) ) ;
#54879 = CARTESIAN_POINT ( 'NONE',  ( -98.19807390327306962, -289.3017715993170782, -225.2083922436063972 ) ) ;
#54880 = CARTESIAN_POINT ( 'NONE',  ( -37.61184835695555506, -298.3821352816740955, -193.3827358768863007 ) ) ;
#54881 = CARTESIAN_POINT ( 'NONE',  ( 197.1159755554518256, 25.84677204156019314, 12.26097734572891795 ) ) ;
#54882 = CARTESIAN_POINT ( 'NONE',  ( 195.3593974516954006, 25.91226055734827582, 14.82602457198997747 ) ) ;
#54883 = CARTESIAN_POINT ( 'NONE',  ( 19.12434464653457766, -289.7762823793407847, -321.7059557083352956 ) ) ;
#54884 = CARTESIAN_POINT ( 'NONE',  ( -111.2586520408596868, -286.6233781216988064, -305.9938812882205070 ) ) ;
#54885 = CARTESIAN_POINT ( 'NONE',  ( -55.21838311417347001, -287.8219893343974718, -197.6407794336381585 ) ) ;
#54886 = CARTESIAN_POINT ( 'NONE',  ( -67.83553264365225743, -288.0193613775954873, -340.4234650214762610 ) ) ;
#54887 = CARTESIAN_POINT ( 'NONE',  ( -63.93500251437468762, -271.7044068885694514, -200.3985586211792054 ) ) ;
#54888 = CARTESIAN_POINT ( 'NONE',  ( -21.65393943413130984, -276.1749814039736179, -197.5929356546862152 ) ) ;
#54889 = CARTESIAN_POINT ( 'NONE',  ( -96.10205377780953029, -288.0003926761864932, -316.0822143136607565 ) ) ;
#54890 = CARTESIAN_POINT ( 'NONE',  ( -101.0453745609532774, -279.8645374037464535, -311.4707963328471010 ) ) ;
#54891 = CIRCLE ( 'NONE', #83608, 0.5000000000000004441 ) ;
#54892 = ORIENTED_EDGE ( 'NONE', *, *, #42128, .F. ) ;
#54893 = ADVANCED_FACE ( 'NONE', ( #45651 ), #13734, .T. ) ;
#54895 = CARTESIAN_POINT ( 'NONE',  ( 7.211006969742085992, -280.0259070666188563, -212.3406256531423537 ) ) ;
#54894 = CARTESIAN_POINT ( 'NONE',  ( -24.87639109164146589, -280.2156146946252306, -198.4332647501296094 ) ) ;
#54896 = CARTESIAN_POINT ( 'NONE',  ( 0.9048563303069437902, -277.6343780841357329, -336.8946121901996094 ) ) ;
#54897 = CARTESIAN_POINT ( 'NONE',  ( 38.27340845060322749, -280.5022611584698211, -282.7052584524505505 ) ) ;
#54898 = CARTESIAN_POINT ( 'NONE',  ( 200.9738562182569694, 293.6303156117443791, -53.99999999999359090 ) ) ;
#54899 = CARTESIAN_POINT ( 'NONE',  ( 38.90534220976931579, -276.6106470413136549, -279.7073161796139402 ) ) ;
#54900 = CARTESIAN_POINT ( 'NONE',  ( -96.41178290437866849, -274.7268709476192043, -222.0351007514593675 ) ) ;
#54901 = CARTESIAN_POINT ( 'NONE',  ( 10.59707575819634329, -295.1948066931273615, -210.1954327657594490 ) ) ;
#54902 = ORIENTED_EDGE ( 'NONE', *, *, #43587, .F. ) ;
#54903 = CARTESIAN_POINT ( 'NONE',  ( 165.2424497756046549, 250.0000000000000568, 22.91843887563435445 ) ) ;
#54904 = CARTESIAN_POINT ( 'NONE',  ( 16.19083254556992912, -287.9141173076805558, -220.2577290444759512 ) ) ;
#54905 = CARTESIAN_POINT ( 'NONE',  ( 13.93663136718700457, -290.1050081977143691, -326.5083411736892458 ) ) ;
#54906 = CARTESIAN_POINT ( 'NONE',  ( -107.8263138186721051, -289.6427314543595344, -289.9336064591886952 ) ) ;
#54907 = CARTESIAN_POINT ( 'NONE',  ( -60.48543178116287322, -285.2676230270463407, -196.9305610713836927 ) ) ;
#54908 = CARTESIAN_POINT ( 'NONE',  ( 200.2110226547167429, 26.62113606806761013, 10.50000000000112799 ) ) ;
#54909 = CARTESIAN_POINT ( 'NONE',  ( -8.196856329979501865, -281.0638363648741915, -338.1624343157080261 ) ) ;
#54910 = CARTESIAN_POINT ( 'NONE',  ( 26.77464060336084017, -289.9187617785838142, -307.8788395695208919 ) ) ;
#54911 = CARTESIAN_POINT ( 'NONE',  ( -83.24154654482278204, -282.1735572530329819, -328.0799892161239200 ) ) ;
#54912 = CARTESIAN_POINT ( 'NONE',  ( -109.2437993338436826, -279.6680353039263309, -285.5707073681669499 ) ) ;
#54913 = CARTESIAN_POINT ( 'NONE',  ( 7.623196754547683973, -276.9120515657534725, -328.0115805298017904 ) ) ;
#54914 = CARTESIAN_POINT ( 'NONE',  ( -113.2704483345547288, -289.4794351917847166, -259.8326481741513589 ) ) ;
#54915 = CARTESIAN_POINT ( 'NONE',  ( -67.13590330410211493, -286.4741778705596289, -199.5341155198975116 ) ) ;
#54916 = CARTESIAN_POINT ( 'NONE',  ( -95.77393617394825753, -285.7210728215443964, -220.2292246856990516 ) ) ;
#54917 = CARTESIAN_POINT ( 'NONE',  ( 33.65064803186798770, -281.9438259724282716, -287.4168490108671108 ) ) ;
#54918 = EDGE_LOOP ( 'NONE', ( #20772, #48747, #35899, #1578 ) ) ;
#54919 = CARTESIAN_POINT ( 'NONE',  ( 208.6208076322478746, 32.98517505407394168, 9.000000000000001776 ) ) ;
#54920 = CARTESIAN_POINT ( 'NONE',  ( -113.0164057037154777, -292.3656190973205753, -274.0549525888752669 ) ) ;
#54921 = VECTOR ( 'NONE', #93602, 1000.000000000000000 ) ;
#54922 = CARTESIAN_POINT ( 'NONE',  ( -61.51677111319927604, -290.4294952290104561, -197.7183827159624343 ) ) ;
#54923 = CARTESIAN_POINT ( 'NONE',  ( 29.30513440849346196, -274.2014525121342672, -239.8804020983503165 ) ) ;
#54924 = CARTESIAN_POINT ( 'NONE',  ( -114.2359538504407652, -295.9103309086441413, -269.5952650262510133 ) ) ;
#54925 = CARTESIAN_POINT ( 'NONE',  ( -5.726795965617193396, -290.9554803908608278, -203.7799019042589350 ) ) ;
#54926 = CARTESIAN_POINT ( 'NONE',  ( -94.74246341223364709, -294.1395260104930571, -317.1049815984326870 ) ) ;
#54927 = AXIS2_PLACEMENT_3D ( 'NONE', #2557, #23855, #24313 ) ;
#54928 = CARTESIAN_POINT ( 'NONE',  ( -56.15263018620973412, -290.5048547564448995, -341.3595668081164263 ) ) ;
#54929 = DIRECTION ( 'NONE',  ( -1.000000000000000000, 0.000000000000000000, 0.000000000000000000 ) ) ;
#54930 = CIRCLE ( 'NONE', #62531, 5.000000000000000888 ) ;
#54931 = CARTESIAN_POINT ( 'NONE',  ( -112.1934414860052840, -292.6128376651122949, -265.6475777042275013 ) ) ;
#54932 = CARTESIAN_POINT ( 'NONE',  ( -9.174023103086078379, -290.4194269143868610, -200.6717328614652160 ) ) ;
#54933 = CARTESIAN_POINT ( 'NONE',  ( -75.05734836781165598, -297.5546916495771939, -335.2027861620937301 ) ) ;
#54934 = CARTESIAN_POINT ( 'NONE',  ( -91.70390561886109992, -286.1946121870005868, -221.2135908675137728 ) ) ;
#54935 = CARTESIAN_POINT ( 'NONE',  ( 3.258994510386305166, -296.5085695020325147, -333.6807072992319831 ) ) ;
#54936 = VECTOR ( 'NONE', #49029, 1000.000000000000000 ) ;
#54937 = CARTESIAN_POINT ( 'NONE',  ( -13.60501259672264496, -276.3386887066903341, -198.8420543268857159 ) ) ;
#54938 = CARTESIAN_POINT ( 'NONE',  ( -8.050736783225303839, -275.4718456513494971, -341.1570214346750163 ) ) ;
#54939 = CARTESIAN_POINT ( 'NONE',  ( -43.26708147556938400, -297.1764333316074840, -193.6983029191631829 ) ) ;
#54940 = CARTESIAN_POINT ( 'NONE',  ( 36.65648359150822699, -273.7725179426865907, -268.8635141839382641 ) ) ;
#54941 = CARTESIAN_POINT ( 'NONE',  ( -43.85315350263300616, -278.0491970760363074, -196.1552225057391752 ) ) ;
#54942 = CARTESIAN_POINT ( 'NONE',  ( -76.79050176104948378, -274.7160357706691229, -208.4666711062203888 ) ) ;
#54943 = CARTESIAN_POINT ( 'NONE',  ( 2.129285921777238411, -273.1445538854864026, -204.9344601681925155 ) ) ;
#54944 = AXIS2_PLACEMENT_3D ( 'NONE', #8593, #87654, #72549 ) ;
#54945 = DIRECTION ( 'NONE',  ( 1.000000000000000000, -0.000000000000000000, 0.000000000000000000 ) ) ;
#54946 = CARTESIAN_POINT ( 'NONE',  ( -71.74996550566946496, -298.3880240043511094, -205.7816262832244263 ) ) ;
#54947 = DIRECTION ( 'NONE',  ( 0.000000000000000000, 0.000000000000000000, 1.000000000000000000 ) ) ;
#54948 = B_SPLINE_CURVE_WITH_KNOTS ( 'NONE', 3,
 ( #16517, #30259, #30730, #59151, #38748, #73363 ),
 .UNSPECIFIED., .F., .F.,
 ( 4, 2, 4 ),
 ( -4.472146915482244616E-06, 0.0003332253989338073027, 0.0006709229447830969287 ),
 .UNSPECIFIED. ) ;
#54950 = CARTESIAN_POINT ( 'NONE',  ( 9.486706258851251405, -274.5501558829931810, -214.2940245204525240 ) ) ;
#54949 = CARTESIAN_POINT ( 'NONE',  ( -40.29998282908324825, -287.1092485472597104, -345.6710339318566412 ) ) ;
#54951 = CIRCLE ( 'NONE', #14092, 0.4999999999999999445 ) ;
#54952 = CARTESIAN_POINT ( 'NONE',  ( 3.180135298615699657, -288.5241132358754044, -335.8987058422258656 ) ) ;
#54953 = CARTESIAN_POINT ( 'NONE',  ( -36.09144325118830210, -288.7036326836868625, -347.3429271837919146 ) ) ;
#54954 = CARTESIAN_POINT ( 'NONE',  ( -86.41075002089942814, -299.3551486533382331, -213.1028438763793815 ) ) ;
#54955 = CARTESIAN_POINT ( 'NONE',  ( -50.82594392346678092, -293.2246655479536912, -343.9695658193610370 ) ) ;
#54956 = CARTESIAN_POINT ( 'NONE',  ( 30.92898429233507684, -281.2047961234276272, -305.6211870235620154 ) ) ;
#54957 = LINE ( 'NONE', #83834, #30541 ) ;
#54958 = CARTESIAN_POINT ( 'NONE',  ( 22.31120660474435624, -278.9296226006674146, -224.8811695122272738 ) ) ;
#54959 = AXIS2_PLACEMENT_3D ( 'NONE', #82352, #37849, #2367 ) ;
#54960 = CARTESIAN_POINT ( 'NONE',  ( 0.000000000000000000, 0.000000000000000000, -9.000000000000001776 ) ) ;
#54961 = CARTESIAN_POINT ( 'NONE',  ( -15.74940643767814841, -287.5615481272288889, -340.5633772645647355 ) ) ;
#54962 = CARTESIAN_POINT ( 'NONE',  ( 139.1539576904058606, 250.5000000000000568, 10.50000000000000000 ) ) ;
#54963 = DIRECTION ( 'NONE',  ( 0.000000000000000000, 1.000000000000000000, -0.000000000000000000 ) ) ;
#54964 = CARTESIAN_POINT ( 'NONE',  ( -69.86239269815402508, -289.6238236197082188, -202.7643578217271170 ) ) ;
#54965 = CARTESIAN_POINT ( 'NONE',  ( -69.81374712839919994, -275.1366480142143587, -204.2077059900510392 ) ) ;
#54966 = CARTESIAN_POINT ( 'NONE',  ( 36.41147801202088630, -282.7247469650839093, -250.3346821671716498 ) ) ;
#54968 = CARTESIAN_POINT ( 'NONE',  ( -110.0957674051256845, -284.4731720123492664, -276.3482453945421753 ) ) ;
#54967 = CARTESIAN_POINT ( 'NONE',  ( -62.27649911082106371, -295.7495263444196780, -199.2509035166758338 ) ) ;
#54969 = CARTESIAN_POINT ( 'NONE',  ( -67.31398096410767096, -275.0765042358539745, -203.1384047884904760 ) ) ;
#54970 = CARTESIAN_POINT ( 'NONE',  ( 32.21214304518407090, -276.0526193022728876, -247.5075887888366992 ) ) ;
#54971 = CARTESIAN_POINT ( 'NONE',  ( -65.79332031218706334, -285.4244470023178337, -339.7687797464978416 ) ) ;
#54972 = EDGE_CURVE ( 'NONE', #66639, #21957, #30334, .T. ) ;
#54973 = CARTESIAN_POINT ( 'NONE',  ( -106.5939053662181664, -271.7909678117702583, -246.3120401825525221 ) ) ;
#54974 = ORIENTED_EDGE ( 'NONE', *, *, #17688, .F. ) ;
#54975 = CARTESIAN_POINT ( 'NONE',  ( 204.7092198302316035, 294.9664581756286452, -54.00000000004281731 ) ) ;
#54976 = CARTESIAN_POINT ( 'NONE',  ( 37.42245399029074804, -293.1550338909091806, -251.9404430900545435 ) ) ;
#54977 = CARTESIAN_POINT ( 'NONE',  ( -75.58395531270943479, -287.5190959269237965, -206.2566975345147284 ) ) ;
#54978 = CARTESIAN_POINT ( 'NONE',  ( -147.0026986695707762, -210.7421749798627388, 21.50000000000000000 ) ) ;
#54979 = CARTESIAN_POINT ( 'NONE',  ( 40.64545035920995986, -279.2666405000204009, -288.1938231032136741 ) ) ;
#54980 = CARTESIAN_POINT ( 'NONE',  ( -114.0490556539642597, -277.8055653820600241, -265.8733091314261401 ) ) ;
#54981 = CARTESIAN_POINT ( 'NONE',  ( -112.3494774162785035, -288.7814145140571327, -283.8615341361522155 ) ) ;
#54982 = CARTESIAN_POINT ( 'NONE',  ( -98.09304339416746643, -285.4960014812526197, -312.1631152127524160 ) ) ;
#54983 = CARTESIAN_POINT ( 'NONE',  ( -67.19106464212329399, -279.2091295583560964, -338.0884348761078968 ) ) ;
#54984 = CARTESIAN_POINT ( 'NONE',  ( -112.4227553300736275, -286.1597201042796996, -255.8924558512456429 ) ) ;
#54985 = CARTESIAN_POINT ( 'NONE',  ( -74.00839501187840597, -282.3454516190755044, -334.0011452165243213 ) ) ;
#54986 = CARTESIAN_POINT ( 'NONE',  ( -68.15052461716483378, -281.6477724934836147, -201.9671904972286995 ) ) ;
#54987 = CARTESIAN_POINT ( 'NONE',  ( -46.88310250723962724, -274.1008436232017402, -193.9545629945613427 ) ) ;
#54988 = CARTESIAN_POINT ( 'NONE',  ( -37.12909664450568670, -276.8828453939410679, -347.3738831291669271 ) ) ;
#54990 = CARTESIAN_POINT ( 'NONE',  ( -87.44143037816654385, -297.6778042941705280, -325.4186444838368857 ) ) ;
#54989 = VECTOR ( 'NONE', #31087, 1000.000000000000000 ) ;
#54991 = DIRECTION ( 'NONE',  ( 0.000000000000000000, 0.000000000000000000, -1.000000000000000000 ) ) ;
#54992 = EDGE_CURVE ( 'NONE', #24992, #33695, #34873, .T. ) ;
#54993 = ADVANCED_FACE ( 'NONE', ( #75951 ), #11083, .T. ) ;
#54994 = CARTESIAN_POINT ( 'NONE',  ( 189.4188515237862589, 293.9636489450775798, -40.00000000000000711 ) ) ;
#54995 = CARTESIAN_POINT ( 'NONE',  ( -112.1658791884912461, -294.8440539516494709, -258.3775054057362013 ) ) ;
#54996 = CARTESIAN_POINT ( 'NONE',  ( 7.613327878650325786, -275.9275156067258763, -328.0192763208009410 ) ) ;
#54997 = AXIS2_PLACEMENT_3D ( 'NONE', #50034, #56229, #57628 ) ;
#54998 = CARTESIAN_POINT ( 'NONE',  ( -96.63852159007261378, -274.4118757709899796, -221.8442972438961931 ) ) ;
#54999 = CARTESIAN_POINT ( 'NONE',  ( 36.46424283905096786, -289.3927457632027540, -276.5439795133319762 ) ) ;
#55000 = CARTESIAN_POINT ( 'NONE',  ( -93.16889471955472857, -297.3564947689035307, -322.3998925472031374 ) ) ;
#55001 = CARTESIAN_POINT ( 'NONE',  ( -3.390892033970570374, -295.8190153851442119, -339.0440637491524285 ) ) ;
#55002 = CARTESIAN_POINT ( 'NONE',  ( -82.86398811087624949, -293.4285347695969790, -210.9006660024705297 ) ) ;
#55003 = CARTESIAN_POINT ( 'NONE',  ( -7.239164970448359604, -278.4477156171212755, -201.8353064887004393 ) ) ;
#55004 = CIRCLE ( 'NONE', #58077, 0.5000000000000004441 ) ;
#55005 = CARTESIAN_POINT ( 'NONE',  ( -66.65891021632147329, -281.5852767898416573, -201.9234150036206472 ) ) ;
#55006 = CARTESIAN_POINT ( 'NONE',  ( -111.2369820726292602, -294.5103544024182725, -279.7639477784231872 ) ) ;
#55007 = CARTESIAN_POINT ( 'NONE',  ( -104.6753602359658970, -285.9562541416623276, -305.2099924881246125 ) ) ;
#55008 = CARTESIAN_POINT ( 'NONE',  ( 35.06235889184210919, -286.6243781957236934, -281.9248511678536033 ) ) ;
#55009 = CARTESIAN_POINT ( 'NONE',  ( -105.9390882850879336, -263.2164998017994435, -317.4572233070413745 ) ) ;
#55010 = VERTEX_POINT ( 'NONE', #54633 ) ;
#55011 = CARTESIAN_POINT ( 'NONE',  ( -67.55257157191294937, -285.3112430140916445, -203.8826197033241385 ) ) ;
#55012 = ORIENTED_EDGE ( 'NONE', *, *, #73993, .F. ) ;
#55013 = CARTESIAN_POINT ( 'NONE',  ( -5.570976448279924220, -283.7236297573737147, -340.1616453998773864 ) ) ;
#55014 = TOROIDAL_SURFACE ( 'NONE', #23317, 1.500000000000001776, 0.5000000000000000000 ) ;
#55015 = CARTESIAN_POINT ( 'NONE',  ( -92.93263885425096760, -273.5588659936238400, -222.9948510194683706 ) ) ;
#55016 = CARTESIAN_POINT ( 'NONE',  ( 1.334521340504313036, -285.3516813282454336, -204.2235567117757853 ) ) ;
#55017 = CIRCLE ( 'NONE', #76180, 24.00000000000000355 ) ;
#55018 = CARTESIAN_POINT ( 'NONE',  ( -36.76639190577337502, -281.0004650638578028, -193.5855615632846991 ) ) ;
#55019 = CARTESIAN_POINT ( 'NONE',  ( 195.5463244018911269, 20.93879963055986693, -14.58213394506753602 ) ) ;
#55020 = CARTESIAN_POINT ( 'NONE',  ( -111.7302002237050544, -280.2868291554520397, -253.3593883797751118 ) ) ;
#55021 = CARTESIAN_POINT ( 'NONE',  ( 25.09262785313039146, -282.4829049339294897, -315.4134738469486479 ) ) ;
#55022 = CARTESIAN_POINT ( 'NONE',  ( -102.0172624299487154, -282.4809262143061233, -239.1787733560258289 ) ) ;
#55023 = CARTESIAN_POINT ( 'NONE',  ( -113.0733666116212106, -274.4133621447950873, -270.3848156438984915 ) ) ;
#55024 = ORIENTED_EDGE ( 'NONE', *, *, #16173, .T. ) ;
#55025 = CARTESIAN_POINT ( 'NONE',  ( 25.31494228580528727, -276.9991902721702104, -229.4444516038402924 ) ) ;
#55026 = CARTESIAN_POINT ( 'NONE',  ( 83.91869577041705952, 83.53290714828214902, -302.0006688339001926 ) ) ;
#55027 = CIRCLE ( 'NONE', #79247, 2.000000000000000000 ) ;
#55028 = CARTESIAN_POINT ( 'NONE',  ( 10.34629288835905925, -278.7336583536934995, -212.8680968326108882 ) ) ;
#55029 = CARTESIAN_POINT ( 'NONE',  ( 29.99047499235947001, -294.8505367082642579, -235.0292724524110781 ) ) ;
#55030 = CARTESIAN_POINT ( 'NONE',  ( -41.05267997585957573, -294.4486358492787303, -343.3813824908961578 ) ) ;
#55031 = CARTESIAN_POINT ( 'NONE',  ( -88.60381308502861941, -290.8630468635778357, -212.9875815893325637 ) ) ;
#55032 = FACE_OUTER_BOUND ( 'NONE', #53654, .T. ) ;
#55034 = CARTESIAN_POINT ( 'NONE',  ( 25.64399040087455006, -285.4278823042268414, -231.9001871203971064 ) ) ;
#55033 = CARTESIAN_POINT ( 'NONE',  ( -97.81931182513881140, -294.4987277959338599, -317.0629892348457020 ) ) ;
#55035 = CARTESIAN_POINT ( 'NONE',  ( 30.63039618845291656, -295.8073729279712438, -300.2050386357032039 ) ) ;
#55036 = CARTESIAN_POINT ( 'NONE',  ( 31.85814902199712861, -286.5643272006735742, -295.1123675489823199 ) ) ;
#55037 = CARTESIAN_POINT ( 'NONE',  ( -83.97361805691599557, -286.7113696298605419, -213.4908662941040234 ) ) ;
#55038 = CARTESIAN_POINT ( 'NONE',  ( 30.68483988825011366, -294.0317792577080809, -234.6769264103842829 ) ) ;
#55039 = CARTESIAN_POINT ( 'NONE',  ( -32.13506353297257334, -283.4770510601232445, -343.2368984386381499 ) ) ;
#55040 = CARTESIAN_POINT ( 'NONE',  ( -111.5876131819561721, -295.1093106901842589, -289.2702317953996953 ) ) ;
#55041 = AXIS2_PLACEMENT_3D ( 'NONE', #66642, #74200, #1769 ) ;
#55042 = CARTESIAN_POINT ( 'NONE',  ( -109.3261651164391424, -291.6973232722439775, -243.3320156031787747 ) ) ;
#55043 = CARTESIAN_POINT ( 'NONE',  ( -111.9364526678255203, -291.2810858828339065, -251.4626154007349896 ) ) ;
#55044 = CARTESIAN_POINT ( 'NONE',  ( 21.96293194122219461, -288.3138876279226110, -312.9282487249849396 ) ) ;
#55045 = ORIENTED_EDGE ( 'NONE', *, *, #71944, .F. ) ;
#55046 = DIRECTION ( 'NONE',  ( 0.000000000000000000, 0.000000000000000000, 1.000000000000000000 ) ) ;
#55047 = CARTESIAN_POINT ( 'NONE',  ( -112.9988147667955189, -298.3500086414654220, -275.2831235803675440 ) ) ;
#55048 = CARTESIAN_POINT ( 'NONE',  ( -112.4015799369000206, -295.4242340436867948, -255.4846087154301699 ) ) ;
#55049 = CARTESIAN_POINT ( 'NONE',  ( -32.93692382291894916, -279.1677519355563390, -197.2584067186867287 ) ) ;
#55050 = EDGE_LOOP ( 'NONE', ( #90574, #62159, #62699 ) ) ;
#55051 = CARTESIAN_POINT ( 'NONE',  ( 26.09738068237256314, -274.4845862887783596, -226.8060521823317401 ) ) ;
#55052 = CARTESIAN_POINT ( 'NONE',  ( -100.4809364185774143, -295.5511897397036023, -232.2600215203199809 ) ) ;
#55053 = CARTESIAN_POINT ( 'NONE',  ( -26.82347436592075596, -278.7773891892311440, -343.8473915668690779 ) ) ;
#55054 = CARTESIAN_POINT ( 'NONE',  ( 35.92235194768895923, -273.8510113750921278, -282.6395878273263520 ) ) ;
#55055 = CARTESIAN_POINT ( 'NONE',  ( -103.1172240140658403, -297.3167534111528880, -303.0444805387761562 ) ) ;
#55056 = CARTESIAN_POINT ( 'NONE',  ( -79.91869786696278766, -298.5404709321466044, -210.6834392714524711 ) ) ;
#55057 = DIRECTION ( 'NONE',  ( -0.000000000000000000, 1.000000000000000000, 0.000000000000000000 ) ) ;
#55058 = CARTESIAN_POINT ( 'NONE',  ( -104.5576414103637575, -298.6222694634119534, -234.3540368884742122 ) ) ;
#55059 = CARTESIAN_POINT ( 'NONE',  ( -37.57576512040230909, -296.0490714457672539, -195.1948114014585940 ) ) ;
#55060 = CARTESIAN_POINT ( 'NONE',  ( -66.61249707010439636, -292.3097151932946076, -203.3752006952508680 ) ) ;
#55061 = CARTESIAN_POINT ( 'NONE',  ( -109.5202016453131932, -288.9383771518809567, -284.7657633322738775 ) ) ;
#55062 = CARTESIAN_POINT ( 'NONE',  ( 208.1093360985927347, 29.46709201141245060, 14.78642201437206261 ) ) ;
#55063 = CARTESIAN_POINT ( 'NONE',  ( 34.12942102622687912, -276.4077785896535602, -298.9899697542564923 ) ) ;
#55064 = CARTESIAN_POINT ( 'NONE',  ( -99.28160066503373571, -273.2520370819111690, -231.7288940500819194 ) ) ;
#55065 = CARTESIAN_POINT ( 'NONE',  ( 20.68760796642643385, -282.8716505531958205, -222.2881920403038407 ) ) ;
#55066 = CARTESIAN_POINT ( 'NONE',  ( -5.675020661157632595, -281.3291717171906043, -340.0067903960325566 ) ) ;
#55067 = CARTESIAN_POINT ( 'NONE',  ( -22.96610244330243589, -276.2216018292771764, -345.9576354803714366 ) ) ;
#55068 = CARTESIAN_POINT ( 'NONE',  ( -106.3294106731240731, -283.4240847983955405, -294.8697389306987020 ) ) ;
#55069 = CARTESIAN_POINT ( 'NONE',  ( 37.78658544189189428, -279.5827599667654226, -272.7630195029399829 ) ) ;
#55070 = EDGE_CURVE ( 'NONE', #31130, #17753, #40872, .T. ) ;
#55071 = CARTESIAN_POINT ( 'NONE',  ( -89.64833776897799567, -271.8711971205275404, -218.5982879261818539 ) ) ;
#55072 = CARTESIAN_POINT ( 'NONE',  ( -67.33731659946909076, -279.4456402257029026, -339.1153919793142677 ) ) ;
#55073 = FACE_OUTER_BOUND ( 'NONE', #31835, .T. ) ;
#55074 = CARTESIAN_POINT ( 'NONE',  ( 209.2568086740256206, 34.98978593258856051, 12.00000000000000000 ) ) ;
#55075 = CARTESIAN_POINT ( 'NONE',  ( -59.82656767513203988, -296.0047597183929042, -197.7225550755167944 ) ) ;
#55076 = AXIS2_PLACEMENT_3D ( 'NONE', #38033, #14899, #74037 ) ;
#55077 = CARTESIAN_POINT ( 'NONE',  ( -110.9920390383823161, -280.3590449780327845, -285.4464746146342691 ) ) ;
#55078 = CARTESIAN_POINT ( 'NONE',  ( 18.79913333761682281, -272.8596833547986193, -220.5527788359568717 ) ) ;
#55079 = CARTESIAN_POINT ( 'NONE',  ( 164.5772123382336360, 215.0000000000000568, 23.16839473634451352 ) ) ;
#55080 = CARTESIAN_POINT ( 'NONE',  ( -100.2072239040783614, -285.9089413896007841, -312.3744031281288471 ) ) ;
#55081 = VERTEX_POINT ( 'NONE', #11556 ) ;
#55082 = AXIS2_PLACEMENT_3D ( 'NONE', #76732, #90433, #48770 ) ;
#55083 = CARTESIAN_POINT ( 'NONE',  ( 201.2104617360081704, 60.19600395700751250, 9.999999999999998224 ) ) ;
#55084 = CARTESIAN_POINT ( 'NONE',  ( 37.52703297763829227, -285.6191223741221847, -275.5897078622135723 ) ) ;
#55085 = CARTESIAN_POINT ( 'NONE',  ( -48.18343439339133027, -248.4123448508205172, -502.6442049081569508 ) ) ;
#55086 = CARTESIAN_POINT ( 'NONE',  ( 6.286712081043673628, -293.2400247341555541, -329.4472578727649079 ) ) ;
#55087 = CARTESIAN_POINT ( 'NONE',  ( 8.728284001572998108, -286.5524324248123662, -328.5712720771620070 ) ) ;
#55088 = CARTESIAN_POINT ( 'NONE',  ( -96.12512592106646991, -239.9971452530988358, -342.0757611934672582 ) ) ;
#55089 = CARTESIAN_POINT ( 'NONE',  ( -91.47217133725644089, -295.2819183495281550, -218.3744672509484133 ) ) ;
#55090 = CARTESIAN_POINT ( 'NONE',  ( -3.776712206258508342, -284.9668114387247329, -201.8186270729092087 ) ) ;
#55091 = CARTESIAN_POINT ( 'NONE',  ( 32.72982709204060825, -282.8462518437090694, -247.0394153964454347 ) ) ;
#55092 = CARTESIAN_POINT ( 'NONE',  ( 28.86780280704394386, -280.2834824471888737, -307.7547008041527192 ) ) ;
#55093 = CARTESIAN_POINT ( 'NONE',  ( -8.218492891473735185, -288.6599682130220117, -337.3542252515497921 ) ) ;
#55094 = CONICAL_SURFACE ( 'NONE', #59643, 1.898405138727909947, 0.09862129276975308001 ) ;
#55095 = TOROIDAL_SURFACE ( 'NONE', #50567, 1.000000000000000000, 0.5000000000000000000 ) ;
#55096 = CARTESIAN_POINT ( 'NONE',  ( -51.96203921225311007, -281.2867868616741021, -198.1867062476765113 ) ) ;
#55097 = CARTESIAN_POINT ( 'NONE',  ( 0.4746802127685552097, -281.3725421214461448, -207.6724285456314476 ) ) ;
#55098 = CARTESIAN_POINT ( 'NONE',  ( 38.05711380274217248, -289.5466105002838617, -271.5007028480964095 ) ) ;
#55099 = EDGE_LOOP ( 'NONE', ( #45437, #78128, #1450, #21046 ) ) ;
#55100 = CIRCLE ( 'NONE', #79318, 5.654241149514405151 ) ;
#55101 = CARTESIAN_POINT ( 'NONE',  ( -46.88099868354511557, -273.9341904422645939, -193.9543003347235413 ) ) ;
#55102 = CARTESIAN_POINT ( 'NONE',  ( -85.73257901406893211, -291.7052918818141052, -327.2639039531634921 ) ) ;
#55103 = CARTESIAN_POINT ( 'NONE',  ( 207.8064396648212551, 36.74001737686529623, 13.57731244650625690 ) ) ;
#55104 = CARTESIAN_POINT ( 'NONE',  ( -99.86837403722181250, -298.4090924074129703, -320.2651865833026363 ) ) ;
#55105 = ORIENTED_EDGE ( 'NONE', *, *, #25741, .F. ) ;
#55106 = CARTESIAN_POINT ( 'NONE',  ( 36.37920228237386056, -273.7399587383893049, -285.0327565243341041 ) ) ;
#55107 = VERTEX_POINT ( 'NONE', #85401 ) ;
#55108 = CARTESIAN_POINT ( 'NONE',  ( 151.9709352735115147, -299.5541904835127980, -197.2582414438974183 ) ) ;
#55109 = CARTESIAN_POINT ( 'NONE',  ( -110.0427152187716615, -294.6617036427807079, -293.2303160266133091 ) ) ;
#55110 = CARTESIAN_POINT ( 'NONE',  ( -57.91611124994465598, -297.2867469880741851, -200.2563246479271868 ) ) ;
#55111 = CARTESIAN_POINT ( 'NONE',  ( 23.33163633881805055, -289.6495488696513121, -312.2098436545985010 ) ) ;
#55112 = CIRCLE ( 'NONE', #14311, 2.000000000000000000 ) ;
#55113 = CARTESIAN_POINT ( 'NONE',  ( -81.20895526196396474, -285.4172873167271405, -330.0372665317050291 ) ) ;
#55114 = CARTESIAN_POINT ( 'NONE',  ( -90.39002824820366300, -292.7445804157604812, -215.2923836465211878 ) ) ;
#55115 = CARTESIAN_POINT ( 'NONE',  ( -71.67008800354003029, -290.8114184341671375, -338.7340662914699578 ) ) ;
#55116 = CARTESIAN_POINT ( 'NONE',  ( -84.93619388626592581, -287.3962458661115988, -212.3301429755593688 ) ) ;
#55117 = CARTESIAN_POINT ( 'NONE',  ( -96.81878921080129885, -279.3759210904946144, -221.4378955750481452 ) ) ;
#55118 = CARTESIAN_POINT ( 'NONE',  ( -109.4317407034382796, -294.9238296613741568, -247.5529225358245924 ) ) ;
#55119 = CARTESIAN_POINT ( 'NONE',  ( 19.78208454764835622, -282.0872807508259825, -322.0712179649178211 ) ) ;
#55120 = CARTESIAN_POINT ( 'NONE',  ( 22.46244029927251873, -276.8065720072918907, -226.3800962795182272 ) ) ;
#55121 = CARTESIAN_POINT ( 'NONE',  ( -6.941161984400275209, -279.1233781216987495, -333.4151289067050357 ) ) ;
#55122 = B_SPLINE_CURVE_WITH_KNOTS ( 'NONE', 3,
 ( #31073, #67051, #73237, #66136 ),
 .UNSPECIFIED., .F., .F.,
 ( 4, 4 ),
 ( 0.000000000000000000, 0.001235754004288067880 ),
 .UNSPECIFIED. ) ;
#55123 = CARTESIAN_POINT ( 'NONE',  ( -103.9019338409810018, -276.2157459506518649, -306.5556032828854995 ) ) ;
#55124 = DIRECTION ( 'NONE',  ( 0.000000000000000000, 1.000000000000000000, 0.000000000000000000 ) ) ;
#55125 = CARTESIAN_POINT ( 'NONE',  ( 29.03120913537884817, -280.6467076401698932, -239.7009358238125571 ) ) ;
#55126 = CARTESIAN_POINT ( 'NONE',  ( -113.8153468472678469, -279.8131504042410143, -265.9125142601948824 ) ) ;
#55127 = CARTESIAN_POINT ( 'NONE',  ( -106.4620324521435037, -284.0406938643907893, -236.9665095601148721 ) ) ;
#55128 = CARTESIAN_POINT ( 'NONE',  ( 19.23693497491149174, -294.6436100630608053, -222.6449565105515660 ) ) ;
#55129 = CARTESIAN_POINT ( 'NONE',  ( 38.51879647238281024, -277.0547134257152493, -262.6409225931761853 ) ) ;
#55130 = CARTESIAN_POINT ( 'NONE',  ( -0.2989814327212445000, -275.8492501569752449, -203.4049401091162395 ) ) ;
#55131 = CYLINDRICAL_SURFACE ( 'NONE', #87707, 24.00000000000001066 ) ;
#55132 = CARTESIAN_POINT ( 'NONE',  ( -24.33168797528820448, -276.7148708051191761, -342.2438959058888486 ) ) ;
#55133 = CARTESIAN_POINT ( 'NONE',  ( -108.4568213082627892, -298.8558147294182277, -246.9014283893224047 ) ) ;
#55134 = CARTESIAN_POINT ( 'NONE',  ( -72.00537838965749415, -283.5925013780081940, -204.0402476723845950 ) ) ;
#55135 = CARTESIAN_POINT ( 'NONE',  ( 39.42030021258337058, -293.1466395762262209, -264.5870730265211250 ) ) ;
#55136 = CARTESIAN_POINT ( 'NONE',  ( 37.23628636940647141, -288.9538419730869805, -254.6594656673554766 ) ) ;
#55137 = EDGE_CURVE ( 'NONE', #60346, #68064, #1609, .T. ) ;
#55138 = CARTESIAN_POINT ( 'NONE',  ( 20.43497337705931471, -291.8389277840722684, -225.2178247258592023 ) ) ;
#55139 = ORIENTED_EDGE ( 'NONE', *, *, #51429, .F. ) ;
#55140 = CARTESIAN_POINT ( 'NONE',  ( -36.36750755057224183, -290.6388760579702648, -193.9436219705045232 ) ) ;
#55141 = CARTESIAN_POINT ( 'NONE',  ( -12.24895511555226513, -292.0543827685047518, -201.7328722968619275 ) ) ;
#55142 = EDGE_LOOP ( 'NONE', ( #79487, #321, #2261, #81784 ) ) ;
#55143 = CARTESIAN_POINT ( 'NONE',  ( 36.39020323517412692, -288.3641411897697822, -249.0753066624780274 ) ) ;
#55144 = CARTESIAN_POINT ( 'NONE',  ( -110.1800361393731862, -278.9535340963604426, -265.1973699433982006 ) ) ;
#55145 = ADVANCED_FACE ( 'NONE', ( #27645 ), #27171, .F. ) ;
#55146 = CARTESIAN_POINT ( 'NONE',  ( -41.94082350121679781, -294.0290266843757649, -346.9661620694162707 ) ) ;
#55147 = CARTESIAN_POINT ( 'NONE',  ( -105.3458319326085046, -285.6689643164045265, -234.3479059576969519 ) ) ;
#55148 = CARTESIAN_POINT ( 'NONE',  ( 38.53529940281632804, -287.7221113214654906, -257.3057220293805472 ) ) ;
#55149 = CARTESIAN_POINT ( 'NONE',  ( -24.05748596012324114, -283.2110619448767466, -342.1637442620149159 ) ) ;
#55150 = CARTESIAN_POINT ( 'NONE',  ( 199.7395823140011828, 289.5256457063815105, -97.52092915841859622 ) ) ;
#55151 = CARTESIAN_POINT ( 'NONE',  ( 101.7873421534306999, 116.6550764272915472, -281.9818386274820909 ) ) ;
#55152 = CARTESIAN_POINT ( 'NONE',  ( 63.99139254834007318, 46.87924742655182087, -315.4201083341205845 ) ) ;
#55153 = CARTESIAN_POINT ( 'NONE',  ( 34.78657350390782454, -274.5870674316201416, -258.0345504581135856 ) ) ;
#55154 = CARTESIAN_POINT ( 'NONE',  ( -3.737971832439035413, -275.5181263251067776, -335.5149015954532388 ) ) ;
#55155 = CARTESIAN_POINT ( 'NONE',  ( -62.81875398917058106, -297.2368315542349819, -197.7632762122106556 ) ) ;
#55156 = CARTESIAN_POINT ( 'NONE',  ( -110.3257684885215753, -272.2967757702207905, -283.7855995824492652 ) ) ;
#55157 = CARTESIAN_POINT ( 'NONE',  ( 39.12969167563818473, -274.2832489175389696, -274.0370798290085759 ) ) ;
#55158 = CARTESIAN_POINT ( 'NONE',  ( -93.69976746502780429, -274.9854953453994426, -222.3650707476377022 ) ) ;
#55159 = ORIENTED_EDGE ( 'NONE', *, *, #4833, .F. ) ;
#55160 = CARTESIAN_POINT ( 'NONE',  ( 7.805039230333843392, -299.5456763218493847, -193.5893858898706412 ) ) ;
#55161 = CARTESIAN_POINT ( 'NONE',  ( 31.02996916658182514, -287.6993974261896483, -244.4636616652207692 ) ) ;
#55162 = CARTESIAN_POINT ( 'NONE',  ( -84.07886516745874417, -296.4786911568550067, -331.4183278053247932 ) ) ;
#55163 = CARTESIAN_POINT ( 'NONE',  ( -102.2678288998948517, -297.5859989288934457, -229.0800726243258509 ) ) ;
#55164 = CARTESIAN_POINT ( 'NONE',  ( 20.52450394613299167, -294.3453701634355753, -314.8844214141962539 ) ) ;
#55165 = ORIENTED_EDGE ( 'NONE', *, *, #28287, .F. ) ;
#55166 = AXIS2_PLACEMENT_3D ( 'NONE', #22707, #1867, #22260 ) ;
#55167 = CARTESIAN_POINT ( 'NONE',  ( 35.50400189142177254, -277.7290717748321640, -290.4797439349166552 ) ) ;
#55168 = VERTEX_POINT ( 'NONE', #33808 ) ;
#55169 = CARTESIAN_POINT ( 'NONE',  ( 22.83111133083752975, -280.4171768318689146, -222.3947883097530109 ) ) ;
#55170 = PRODUCT_DEFINITION_CONTEXT ( 'detailed design', #57215, 'design' ) ;
#55171 = CARTESIAN_POINT ( 'NONE',  ( -64.40898970142997371, -278.3554151877087293, -338.4647322349119918 ) ) ;
#55172 = CARTESIAN_POINT ( 'NONE',  ( 37.73811906032817376, -277.4648157605892607, -282.3964475737441262 ) ) ;
#55173 = CARTESIAN_POINT ( 'NONE',  ( -109.8645536581271642, -276.3101747354804161, -290.8267604190215252 ) ) ;
#55174 = CARTESIAN_POINT ( 'NONE',  ( -71.72026397244610507, -298.2366291088175672, -205.8332807532226241 ) ) ;
#55175 = TOROIDAL_SURFACE ( 'NONE', #32531, 5.654241149514406040, 0.5000000000000000000 ) ;
#55176 = CARTESIAN_POINT ( 'NONE',  ( -53.29465604947596091, -293.8353422073069510, -342.2527766614713300 ) ) ;
#55177 = DIRECTION ( 'NONE',  ( 0.9167375550253600291, 0.000000000000000000, -0.3994899938748465162 ) ) ;
#55178 = CARTESIAN_POINT ( 'NONE',  ( 36.11508859233749291, -281.7567971005397567, -247.4782183821648118 ) ) ;
#55179 = CARTESIAN_POINT ( 'NONE',  ( -89.08432308948820832, -277.9712187743338632, -321.9275661965899644 ) ) ;
#55180 = CIRCLE ( 'NONE', #38534, 0.5000000000000004441 ) ;
#55181 = CARTESIAN_POINT ( 'NONE',  ( -8.435081188999458135, -287.3664129927677777, -341.2110567234966538 ) ) ;
#55182 = CARTESIAN_POINT ( 'NONE',  ( -2.260155546028384421, -276.5166566964427943, -204.0717079610543294 ) ) ;
#55183 = CARTESIAN_POINT ( 'NONE',  ( 196.8803347170859865, 24.42324672360809856, 12.49999999999999289 ) ) ;
#55184 = CARTESIAN_POINT ( 'NONE',  ( -39.97410885093962207, -288.2831062310106631, -343.5249103598009128 ) ) ;
#55185 = CARTESIAN_POINT ( 'NONE',  ( -102.4277797940218591, -284.4377262680526428, -229.4085231909915592 ) ) ;
#55186 = CARTESIAN_POINT ( 'NONE',  ( 16.00510946426042125, -279.0607456820833931, -218.9839609021265687 ) ) ;
#55188 = CARTESIAN_POINT ( 'NONE',  ( -109.4949100655157395, -282.3950161994323480, -288.6703641864324368 ) ) ;
#55187 = CARTESIAN_POINT ( 'NONE',  ( 3.042385127813834966, -279.1804755766375479, -208.7816694181454693 ) ) ;
#55189 = CARTESIAN_POINT ( 'NONE',  ( 0.8113929982533748531, -288.5607796618269845, -205.7313282214225296 ) ) ;
#55190 = CARTESIAN_POINT ( 'NONE',  ( -110.7488192859057392, -279.7893912150559572, -267.9102303766407545 ) ) ;
#55191 = FACE_BOUND ( 'NONE', #49171, .T. ) ;
#55192 = CARTESIAN_POINT ( 'NONE',  ( -78.51822587480140214, -293.4984325618755179, -207.6133449737126853 ) ) ;
#55193 = CARTESIAN_POINT ( 'NONE',  ( -86.45751392806090507, -275.9628475672048467, -328.4093815558453002 ) ) ;
#55194 = CARTESIAN_POINT ( 'NONE',  ( -32.40540072151409845, -277.6398290439803418, -343.3462319723126370 ) ) ;
#55195 = CARTESIAN_POINT ( 'NONE',  ( -105.3361541654581117, -286.1318357357983473, -302.4045672914245984 ) ) ;
#55196 = EDGE_CURVE ( 'NONE', #20929, #24375, #69322, .T. ) ;
#55197 = EDGE_CURVE ( 'NONE', #33611, #55253, #54515, .T. ) ;
#55198 = CARTESIAN_POINT ( 'NONE',  ( 196.7837483607274294, 69.56983351252434034, 10.93883090039470396 ) ) ;
#55199 = CARTESIAN_POINT ( 'NONE',  ( -112.6746729194045855, -292.3895489858472843, -276.8546433482543421 ) ) ;
#55200 = CARTESIAN_POINT ( 'NONE',  ( -96.92632140702052368, -295.1757803319283084, -224.7917452346152913 ) ) ;
#55201 = CARTESIAN_POINT ( 'NONE',  ( 35.79092297157611569, -287.0464164546436905, -293.9360678017284840 ) ) ;
#55202 = FACE_OUTER_BOUND ( 'NONE', #84663, .T. ) ;
#55203 = CARTESIAN_POINT ( 'NONE',  ( 34.60755553167483356, -274.0398199433121249, -255.3146863642739675 ) ) ;
#55204 = CARTESIAN_POINT ( 'NONE',  ( 2.208194918090676584, -292.6563584883252815, -333.2445250748014018 ) ) ;
#55205 = DIRECTION ( 'NONE',  ( 1.000000000000000000, -1.124465274301078034E-16, -0.000000000000000000 ) ) ;
#55206 = DIRECTION ( 'NONE',  ( 0.000000000000000000, 1.000000000000000000, 0.000000000000000000 ) ) ;
#55207 = CARTESIAN_POINT ( 'NONE',  ( -36.36759647675409468, -290.5440417597841929, -194.0477511856339277 ) ) ;
#55208 = CARTESIAN_POINT ( 'NONE',  ( -79.78585596363124921, -287.0681116616775626, -209.9250792897136648 ) ) ;
#55209 = CARTESIAN_POINT ( 'NONE',  ( 37.67091937069337604, -285.9497574773290012, -282.8081316248267854 ) ) ;
#55210 = CARTESIAN_POINT ( 'NONE',  ( -79.66286394741386800, -286.8932837217631686, -210.0964393025636241 ) ) ;
#55211 = DIRECTION ( 'NONE',  ( -1.000000000000000000, 0.000000000000000000, 0.000000000000000000 ) ) ;
#55212 = CARTESIAN_POINT ( 'NONE',  ( -70.06380692778058972, -286.4125189212716123, -204.9111776814588950 ) ) ;
#55213 = CARTESIAN_POINT ( 'NONE',  ( 33.88938516473130846, -295.2135217279840163, -245.6159439202195074 ) ) ;
#55214 = CARTESIAN_POINT ( 'NONE',  ( 25.74204973801777996, -273.0746986587453762, -228.7707981888274560 ) ) ;
#55215 = CARTESIAN_POINT ( 'NONE',  ( 39.60248571057819333, -275.9314387767858534, -274.0387203528847522 ) ) ;
#55216 = CARTESIAN_POINT ( 'NONE',  ( -34.98044797458204869, -290.1614090621051787, -194.8251137098301626 ) ) ;
#55217 = CARTESIAN_POINT ( 'NONE',  ( -88.93144521210125220, -279.3505833085660583, -213.1990833602177986 ) ) ;
#55218 = CARTESIAN_POINT ( 'NONE',  ( -58.85880352909613578, -297.3117773647936701, -341.8374151835903945 ) ) ;
#55219 = CARTESIAN_POINT ( 'NONE',  ( -43.54160339317392214, -248.0334966641273127, -472.6442049081569508 ) ) ;
#55220 = CARTESIAN_POINT ( 'NONE',  ( 123.4306832106270946, -178.2391364535880882, 4.999999999999990230 ) ) ;
#55221 = CARTESIAN_POINT ( 'NONE',  ( -68.97210693730590947, -284.3120884346226944, -204.0090065468893954 ) ) ;
#55222 = CARTESIAN_POINT ( 'NONE',  ( -79.35017544545200963, -275.7650988312102527, -331.6295543714248879 ) ) ;
#55223 = CARTESIAN_POINT ( 'NONE',  ( 21.32717738862364953, -278.9096077384258479, -223.6184964271196804 ) ) ;
#55224 = CARTESIAN_POINT ( 'NONE',  ( 140.6539576904058606, 275.0000000000000568, -11.50000000000000000 ) ) ;
#55225 = CARTESIAN_POINT ( 'NONE',  ( 4.499316900309763056, -273.0851240053311244, -206.4859018074274672 ) ) ;
#55226 = CARTESIAN_POINT ( 'NONE',  ( -101.9508798439227490, -277.4355544977078694, -304.5597519363249717 ) ) ;
#55227 = CARTESIAN_POINT ( 'NONE',  ( -39.69193781160541334, -296.6022915896484164, -344.0295160471929421 ) ) ;
#55228 = CARTESIAN_POINT ( 'NONE',  ( -6.342656464704358399, -279.3702204652519185, -200.2002566725798545 ) ) ;
#55229 = CARTESIAN_POINT ( 'NONE',  ( -50.50176172447309852, -296.1656045496982301, -342.4043079885302632 ) ) ;
#55230 = CARTESIAN_POINT ( 'NONE',  ( -40.43718541074416351, -299.3293050105615976, -193.8651226438979620 ) ) ;
#55231 = CARTESIAN_POINT ( 'NONE',  ( -99.29617458852614220, -272.7521564427878502, -231.7123071202326514 ) ) ;
#55232 = CARTESIAN_POINT ( 'NONE',  ( -71.14431879194852115, -293.6060966457828272, -203.4105121301606971 ) ) ;
#55233 = CARTESIAN_POINT ( 'NONE',  ( -87.75154436182388906, -285.5374847025777854, -212.0853087964289898 ) ) ;
#55234 = CARTESIAN_POINT ( 'NONE',  ( 34.56529314332229319, -273.3844938012794046, -246.3274069948136002 ) ) ;
#55235 = CARTESIAN_POINT ( 'NONE',  ( -57.29294578360175905, -289.1358991989440597, -344.7865657775103614 ) ) ;
#55236 = CARTESIAN_POINT ( 'NONE',  ( -35.65024809727083266, -282.0533365829164154, -195.7227977055770509 ) ) ;
#55237 = CARTESIAN_POINT ( 'NONE',  ( 30.69935905039540458, -286.9738217597354151, -297.5869968447987048 ) ) ;
#55238 = CARTESIAN_POINT ( 'NONE',  ( -34.99674505633289812, -290.0814155857904666, -195.3849731050563605 ) ) ;
#55239 = VERTEX_POINT ( 'NONE', #26708 ) ;
#55240 = CARTESIAN_POINT ( 'NONE',  ( 196.7899183121812712, 289.3460118731243824, -81.74456998406768093 ) ) ;
#55241 = CARTESIAN_POINT ( 'NONE',  ( -18.46364438118356688, -288.3100947372988685, -340.9942502644269666 ) ) ;
#55242 = CARTESIAN_POINT ( 'NONE',  ( -4.254362200211457612, -283.5678479515829054, -339.6435096994434844 ) ) ;
#55243 = CARTESIAN_POINT ( 'NONE',  ( -72.05511189597812916, -290.6632161082450807, -201.8790591540609398 ) ) ;
#55244 = CARTESIAN_POINT ( 'NONE',  ( -5.299128797975815708, -282.0669317393888491, -201.2256419900265598 ) ) ;
#55245 = CARTESIAN_POINT ( 'NONE',  ( 37.49873848970126744, -282.6666377438206155, -254.4174803007550167 ) ) ;
#55246 = CARTESIAN_POINT ( 'NONE',  ( 23.68369767749559429, -280.8289655848830080, -230.2087408335016505 ) ) ;
#55247 = CARTESIAN_POINT ( 'NONE',  ( -31.20066297429009339, -276.1298694293079734, -195.5999559729321220 ) ) ;
#55248 = CARTESIAN_POINT ( 'NONE',  ( -24.90781296383362431, -294.8978862385354205, -346.4046464121967119 ) ) ;
#55249 = CARTESIAN_POINT ( 'NONE',  ( -95.39914207738490859, -287.9233282611938876, -317.2778553081587916 ) ) ;
#55250 = AXIS2_PLACEMENT_3D ( 'NONE', #89927, #76208, #48239 ) ;
#55251 = CARTESIAN_POINT ( 'NONE',  ( -107.5719997283207903, -271.6300053544314324, -248.8602684521627282 ) ) ;
#55252 = ORIENTED_EDGE ( 'NONE', *, *, #46092, .T. ) ;
#55253 = VERTEX_POINT ( 'NONE', #55596 ) ;
#55254 = CARTESIAN_POINT ( 'NONE',  ( -90.71201026400952117, -287.2088148994744756, -218.3937290401748328 ) ) ;
#55255 = CARTESIAN_POINT ( 'NONE',  ( 30.63473698249595500, -295.0917375002918561, -305.8674062517867469 ) ) ;
#55256 = CARTESIAN_POINT ( 'NONE',  ( -1.194397296101256334, -283.2102950782972925, -333.9005952094517511 ) ) ;
#55257 = CARTESIAN_POINT ( 'NONE',  ( -39.96694815735507689, -276.1431006282817862, -347.0939478457625569 ) ) ;
#55258 = CARTESIAN_POINT ( 'NONE',  ( -81.87810640496687142, -292.1141240881958083, -207.6728311799460016 ) ) ;
#55259 = CARTESIAN_POINT ( 'NONE',  ( -89.02603870617329562, -283.4748625758033995, -214.8909160566551293 ) ) ;
#55260 = CARTESIAN_POINT ( 'NONE',  ( -7.202393667223206286, -292.7700831896556792, -199.5134292724765430 ) ) ;
#55261 = CARTESIAN_POINT ( 'NONE',  ( -61.25793261280417568, -289.7047503125992307, -339.3546054323115868 ) ) ;
#55262 = DIRECTION ( 'NONE',  ( -0.000000000000000000, -1.000000000000000000, -0.000000000000000000 ) ) ;
#55263 = CARTESIAN_POINT ( 'NONE',  ( 175.2296996224750103, 250.0000000000000568, 0.000000000000000000 ) ) ;
#55264 = CARTESIAN_POINT ( 'NONE',  ( 167.8059441758928472, 229.7153237395507972, -189.9420329269269416 ) ) ;
#55265 = CARTESIAN_POINT ( 'NONE',  ( -37.29506492478459023, -284.5716569555509068, -346.6807208086726177 ) ) ;
#55266 = CARTESIAN_POINT ( 'NONE',  ( -37.30987171927208834, -289.5523547857347353, -195.3611179825600175 ) ) ;
#55267 = ORIENTED_EDGE ( 'NONE', *, *, #18425, .T. ) ;
#55268 = CARTESIAN_POINT ( 'NONE',  ( 32.27446765197596790, -280.1668841413159612, -247.2267995581915727 ) ) ;
#55269 = CARTESIAN_POINT ( 'NONE',  ( 38.16080181485249057, -275.4065684828328244, -285.3650005456399867 ) ) ;
#55270 = CARTESIAN_POINT ( 'NONE',  ( -54.94823617926331849, -281.8255670592818660, -197.5749555423474533 ) ) ;
#55271 = CARTESIAN_POINT ( 'NONE',  ( -81.50230589449645890, -220.2296791547506700, -350.8044924647537073 ) ) ;
#55272 = CARTESIAN_POINT ( 'NONE',  ( -6.451800663324420704, -279.0246754427579390, -200.4583245473610020 ) ) ;
#55273 = CARTESIAN_POINT ( 'NONE',  ( -111.1280896718952107, -282.4223460673914019, -281.9813032666788217 ) ) ;
#55274 = CARTESIAN_POINT ( 'NONE',  ( -48.83908960011165590, -299.6679201047492143, -195.1963459988544400 ) ) ;
#55275 = CARTESIAN_POINT ( 'NONE',  ( 35.76960033030849928, -294.0496810488389201, -270.7540019450332807 ) ) ;
#55277 = EDGE_LOOP ( 'NONE', ( #17290, #27942, #76646, #49560 ) ) ;
#55276 = EDGE_CURVE ( 'NONE', #68989, #41691, #46478, .T. ) ;
#55278 = CARTESIAN_POINT ( 'NONE',  ( -109.1891674642713070, -289.4396237952916522, -254.8955136647435040 ) ) ;
#55279 = CARTESIAN_POINT ( 'NONE',  ( 30.45711740953998614, -276.6744201618842567, -306.7590124399724800 ) ) ;
#55280 = CARTESIAN_POINT ( 'NONE',  ( 32.86001859858366458, -275.2853248856216055, -250.1625354613445893 ) ) ;
#55281 = CARTESIAN_POINT ( 'NONE',  ( -109.8052759601073944, -271.7903385465658062, -245.2509071705767383 ) ) ;
#55282 = CARTESIAN_POINT ( 'NONE',  ( 185.4166944662902665, 214.7015631973135044, 22.87680765314684095 ) ) ;
#55283 = CARTESIAN_POINT ( 'NONE',  ( 156.5191989162425727, 214.5000000000000568, 16.58062614384861178 ) ) ;
#55284 = DIRECTION ( 'NONE',  ( -1.000000000000000000, 0.000000000000000000, 0.000000000000000000 ) ) ;
#55285 = CARTESIAN_POINT ( 'NONE',  ( -43.46191054614098448, -256.7101074799442131, -495.8041560030679307 ) ) ;
#55286 = CARTESIAN_POINT ( 'NONE',  ( -3.466371752806750806, -283.6736478335483298, -335.3881683580153208 ) ) ;
#55287 = CARTESIAN_POINT ( 'NONE',  ( 38.60768600563889663, -283.3424564320947070, -272.7411930432493250 ) ) ;
#55288 = CARTESIAN_POINT ( 'NONE',  ( -93.50570327252459890, -283.2377208077950854, -317.1531837555374409 ) ) ;
#55289 = CARTESIAN_POINT ( 'NONE',  ( 3.388257622749063724, -273.0092043281540555, -208.7572761759778643 ) ) ;
#55290 = CARTESIAN_POINT ( 'NONE',  ( 10.04713895627643439, -282.5733485460163479, -213.1525185080326708 ) ) ;
#55291 = CARTESIAN_POINT ( 'NONE',  ( 33.55967941179866898, -274.2957006032791583, -290.4995933792133656 ) ) ;
#55292 = DIRECTION ( 'NONE',  ( -1.000000000000000000, 0.000000000000000000, 0.000000000000000000 ) ) ;
#55293 = CARTESIAN_POINT ( 'NONE',  ( -11.39362029786622799, -275.4778510705780263, -201.7435684218430936 ) ) ;
#55294 = CARTESIAN_POINT ( 'NONE',  ( 195.5052121915463772, 42.19797087126539736, 12.84284333379224208 ) ) ;
#55295 = EDGE_CURVE ( 'NONE', #7087, #80534, #63188, .T. ) ;
#55296 = CARTESIAN_POINT ( 'NONE',  ( -97.57669682175375669, -279.9946897548765037, -222.6546824133990015 ) ) ;
#55297 = EDGE_LOOP ( 'NONE', ( #70500, #29083, #3927, #63793 ) ) ;
#55298 = EDGE_LOOP ( 'NONE', ( #45832, #20313, #58803, #65803, #32396, #93187 ) ) ;
#55299 = CARTESIAN_POINT ( 'NONE',  ( 175.2296996224750103, 249.5000000000000568, 0.000000000000000000 ) ) ;
#55300 = CARTESIAN_POINT ( 'NONE',  ( -70.54661140398212638, -287.4794191280940936, -202.2601682680719364 ) ) ;
#55301 = CARTESIAN_POINT ( 'NONE',  ( -31.59985972116005470, -294.1751196669293904, -343.3471563650673488 ) ) ;
#55302 = CARTESIAN_POINT ( 'NONE',  ( -91.53259236698066559, -289.1475959591082301, -324.9948077552997461 ) ) ;
#55303 = CARTESIAN_POINT ( 'NONE',  ( 18.55601828459433378, -285.1099397020633432, -221.8490669909610062 ) ) ;
#55305 = CARTESIAN_POINT ( 'NONE',  ( -111.3809146095826890, -288.8173498665217949, -268.4130287025081429 ) ) ;
#55304 = CARTESIAN_POINT ( 'NONE',  ( 33.24023254658363413, -285.8530342012565484, -249.4943870940143142 ) ) ;
#55306 = CARTESIAN_POINT ( 'NONE',  ( -108.4169941214110082, -285.9976925225175819, -252.0462854792802716 ) ) ;
#55307 = CARTESIAN_POINT ( 'NONE',  ( 24.40541982995617687, -274.1300837368632415, -313.0220095974415813 ) ) ;
#55308 = CARTESIAN_POINT ( 'NONE',  ( 36.94434838036111302, -285.7368933597451814, -253.3318863082909616 ) ) ;
#55309 = CARTESIAN_POINT ( 'NONE',  ( -30.73134238605511115, -300.1350572960299132, -195.3588556004923760 ) ) ;
#55310 = CARTESIAN_POINT ( 'NONE',  ( 8.708165461508302840, -284.6815505871022083, -210.9520420542893930 ) ) ;
#55311 = PRODUCT_DEFINITION_FORMATION_WITH_SPECIFIED_SOURCE ( 'ANY', '', #73213, .NOT_KNOWN. ) ;
#55312 = CARTESIAN_POINT ( 'NONE',  ( 23.87263430292015798, -281.9367189436453032, -230.0675252828383748 ) ) ;
#55313 = CARTESIAN_POINT ( 'NONE',  ( 4.557036507022792726, -290.4882716850171960, -332.7672418238798286 ) ) ;
#55314 = DIRECTION ( 'NONE',  ( 0.5000000000000032196, -0.8660254037844368202, 0.000000000000000000 ) ) ;
#55315 = ADVANCED_FACE ( 'NONE', ( #21003 ), #9159, .T. ) ;
#55316 = CARTESIAN_POINT ( 'NONE',  ( 196.5149767539403172, 40.96976812506227361, 12.79486244754526147 ) ) ;
#55317 = CARTESIAN_POINT ( 'NONE',  ( -19.60119479712524537, -296.7460420116595401, -343.8628447275620488 ) ) ;
#55318 = AXIS2_PLACEMENT_3D ( 'NONE', #29188, #67035, #36285 ) ;
#55319 = CARTESIAN_POINT ( 'NONE',  ( -92.75787182491727378, -277.2574126697149381, -219.8235224304492306 ) ) ;
#55320 = CARTESIAN_POINT ( 'NONE',  ( -4.663514487870281222, -291.6689447383485572, -200.8176423392138190 ) ) ;
#55321 = CARTESIAN_POINT ( 'NONE',  ( -106.7464311612196326, -294.6196705321012246, -295.5998168102003092 ) ) ;
#55322 = CARTESIAN_POINT ( 'NONE',  ( 34.71086766197497298, -280.4275378467136193, -284.9043988270296950 ) ) ;
#55323 = CARTESIAN_POINT ( 'NONE',  ( 20.12582473539187333, -272.9744513515419726, -223.0451821115256905 ) ) ;
#55324 = CARTESIAN_POINT ( 'NONE',  ( 2.493830814584487854, -293.9132260496983804, -208.5402229044700846 ) ) ;
#55325 = CARTESIAN_POINT ( 'NONE',  ( -37.37352853689063892, -294.5519495502701943, -195.3611179825600175 ) ) ;
#55326 = CARTESIAN_POINT ( 'NONE',  ( -105.3486530527257798, -294.5810064334737604, -305.0862719101137372 ) ) ;
#55327 = CARTESIAN_POINT ( 'NONE',  ( 24.05411970751454831, -292.3944528033189840, -315.1549753035525896 ) ) ;
#55328 = CARTESIAN_POINT ( 'NONE',  ( -95.40435885385358006, -291.3452768561692210, -315.5932223192789365 ) ) ;
#55329 = CARTESIAN_POINT ( 'NONE',  ( 195.7510731661265595, -143.7221692137691775, 22.50000000000000000 ) ) ;
#55330 = CARTESIAN_POINT ( 'NONE',  ( -104.8560228691733869, -291.7338019572545136, -242.0438180668773498 ) ) ;
#55331 = FACE_OUTER_BOUND ( 'NONE', #92142, .T. ) ;
#55333 = CARTESIAN_POINT ( 'NONE',  ( 16.73817998885948199, -292.8488599158071111, -221.2526383744979341 ) ) ;
#55332 = CARTESIAN_POINT ( 'NONE',  ( 5.958818695645231145, -280.4886725278546464, -332.0972052273217514 ) ) ;
#55334 = CARTESIAN_POINT ( 'NONE',  ( 21.06610096577867353, -280.8747130857748857, -220.1660874738981875 ) ) ;
#55335 = CARTESIAN_POINT ( 'NONE',  ( -61.22914353509621321, -283.0206303925972406, -343.5955716834060922 ) ) ;
#55336 = CARTESIAN_POINT ( 'NONE',  ( 19.19427307647419312, -286.2343163782348938, -319.4663365697116433 ) ) ;
#55337 = CARTESIAN_POINT ( 'NONE',  ( -96.10855236157496506, -282.0635665716423546, -315.7395940009587321 ) ) ;
#55338 = CARTESIAN_POINT ( 'NONE',  ( 27.27464862055146355, -279.4946470173169359, -229.6734459171293850 ) ) ;
#55339 = CARTESIAN_POINT ( 'NONE',  ( 18.13742591029376072, -285.7448594641809336, -217.3358698804441929 ) ) ;
#55340 = CARTESIAN_POINT ( 'NONE',  ( 195.6816644507675562, 41.22368217153885439, 14.37939295600229528 ) ) ;
#55341 = CARTESIAN_POINT ( 'NONE',  ( 19.95413491869341271, -294.5010696573632458, -223.8263267928029734 ) ) ;
#55342 = CARTESIAN_POINT ( 'NONE',  ( -72.55288886850765095, -278.9342408450827406, -338.1900018433767627 ) ) ;
#55343 = CARTESIAN_POINT ( 'NONE',  ( -74.02756898543130148, -277.2208424048024540, -333.4977516667271402 ) ) ;
#55344 = CARTESIAN_POINT ( 'NONE',  ( -94.71272277688144925, -291.4154704905947710, -219.0038812505702026 ) ) ;
#55345 = CARTESIAN_POINT ( 'NONE',  ( -58.11478627734786073, -281.3982086140009073, -343.0640047461504309 ) ) ;
#55346 = CARTESIAN_POINT ( 'NONE',  ( 25.05460489774092991, -292.0829286742416571, -231.9228130497185987 ) ) ;
#55347 = CARTESIAN_POINT ( 'NONE',  ( -109.6701956138007858, -294.2968592608739300, -290.2002054543653458 ) ) ;
#55348 = EDGE_LOOP ( 'NONE', ( #48601, #2815, #79528, #82159, #39457, #19070 ) ) ;
#55349 = DIRECTION ( 'NONE',  ( 0.000000000000000000, 0.000000000000000000, 1.000000000000000000 ) ) ;
#55350 = CARTESIAN_POINT ( 'NONE',  ( 29.54387913903637397, -293.4549884766422565, -299.7602289822567059 ) ) ;
#55351 = LINE ( 'NONE', #83267, #48958 ) ;
#55352 = CARTESIAN_POINT ( 'NONE',  ( 30.89617123739170168, -291.2666405000203440, -285.9686137636504668 ) ) ;
#55353 = CARTESIAN_POINT ( 'NONE',  ( -107.9251138741139897, -272.1384861262200729, -239.8598332598646152 ) ) ;
#55354 = CARTESIAN_POINT ( 'NONE',  ( 21.92416627033979992, -279.0493296385649842, -223.1402444176585789 ) ) ;
#55355 = CARTESIAN_POINT ( 'NONE',  ( -23.88918542111262866, -287.5355938107643965, -194.9923905869694920 ) ) ;
#55356 = CARTESIAN_POINT ( 'NONE',  ( -8.252996814476444953, -286.2773262934074410, -203.4070490691913449 ) ) ;
#55357 = CARTESIAN_POINT ( 'NONE',  ( -99.75206561250479353, -279.5350699662603802, -309.6438209995825446 ) ) ;
#55358 = CARTESIAN_POINT ( 'NONE',  ( -96.93231070470670829, -293.9544938519271113, -315.3355578255349769 ) ) ;
#55359 = CARTESIAN_POINT ( 'NONE',  ( -92.93723497903441455, -297.6243472131266117, -319.2191830237677550 ) ) ;
#55360 = CARTESIAN_POINT ( 'NONE',  ( -107.9964031095898918, -277.6089295595630801, -250.4388713354596803 ) ) ;
#55361 = ORIENTED_EDGE ( 'NONE', *, *, #39899, .F. ) ;
#55362 = CARTESIAN_POINT ( 'NONE',  ( -36.89275367695309171, -297.7243499385728569, -193.3822863192873456 ) ) ;
#55363 = CARTESIAN_POINT ( 'NONE',  ( -110.5916268880976503, -292.3008018687873459, -283.6186603410305338 ) ) ;
#55364 = CARTESIAN_POINT ( 'NONE',  ( 17.00541833075179809, -295.8938911368153413, -323.8480890900463010 ) ) ;
#55365 = DIRECTION ( 'NONE',  ( -0.000000000000000000, -0.000000000000000000, 1.000000000000000000 ) ) ;
#55366 = CARTESIAN_POINT ( 'NONE',  ( -18.43915824921367985, -289.4536710904361598, -341.0295460219195434 ) ) ;
#55367 = CARTESIAN_POINT ( 'NONE',  ( -43.49966619312522909, -252.6696169169302948, -448.1023075023964566 ) ) ;
#55368 = CARTESIAN_POINT ( 'NONE',  ( 36.96103337391910060, -280.8530205513092142, -289.6464493976515087 ) ) ;
#55369 = CARTESIAN_POINT ( 'NONE',  ( -102.2348291789772929, -297.7450393017512624, -229.1034570158358861 ) ) ;
#55370 = CARTESIAN_POINT ( 'NONE',  ( -78.89682229393353907, -289.6384780114020145, -206.9464056147878921 ) ) ;
#55371 = CARTESIAN_POINT ( 'NONE',  ( -60.14587605445937868, -298.0978450219084834, -196.7820501921080165 ) ) ;
#55372 = LINE ( 'NONE', #46828, #64291 ) ;
#55373 = CARTESIAN_POINT ( 'NONE',  ( 219.8344101925596021, 35.72494958537217968, -7.000000000000000888 ) ) ;
#55374 = CARTESIAN_POINT ( 'NONE',  ( 196.2268097803946318, 25.02946980243403985, 13.57081821020089585 ) ) ;
#55375 = CARTESIAN_POINT ( 'NONE',  ( -62.51647696985671132, -290.8938532166030200, -342.4512751567758642 ) ) ;
#55376 = CARTESIAN_POINT ( 'NONE',  ( -88.52914483777347243, -281.9090924074130839, -206.2264541496106460 ) ) ;
#55377 = CARTESIAN_POINT ( 'NONE',  ( 22.80078898073362481, -280.2581365725688443, -222.4215643263058553 ) ) ;
#55378 = CARTESIAN_POINT ( 'NONE',  ( -98.07732992441323461, -287.1488889442275081, -226.6218406911590648 ) ) ;
#55379 = CARTESIAN_POINT ( 'NONE',  ( 26.65425886802522371, -285.5741825527417177, -228.6103871548034476 ) ) ;
#55380 = CARTESIAN_POINT ( 'NONE',  ( -72.75333861237710664, -271.5822585228652883, -204.3788530085386412 ) ) ;
#55381 = CARTESIAN_POINT ( 'NONE',  ( -75.02300922096350178, -275.4666289778325563, -206.1030072348783051 ) ) ;
#55382 = CARTESIAN_POINT ( 'NONE',  ( -111.2216220126953345, -288.5140864063913568, -279.4754659901390141 ) ) ;
#55383 = CARTESIAN_POINT ( 'NONE',  ( -112.0230213362468987, -280.5748415217224760, -257.5937476853273438 ) ) ;
#55384 = AXIS2_PLACEMENT_3D ( 'NONE', #38225, #72383, #7500 ) ;
#55385 = ORIENTED_EDGE ( 'NONE', *, *, #23208, .T. ) ;
#55387 = CARTESIAN_POINT ( 'NONE',  ( 22.20133182572669384, -280.3091536364263447, -227.9521564990508864 ) ) ;
#55386 = CARTESIAN_POINT ( 'NONE',  ( 21.32897384886098990, -280.9428830652790907, -226.9033205156976010 ) ) ;
#55388 = CARTESIAN_POINT ( 'NONE',  ( -7.990171337955164432, -277.7562238104093240, -341.2271656127474557 ) ) ;
#55389 = CARTESIAN_POINT ( 'NONE',  ( -22.62733913665131880, -279.0312568105371156, -195.1307060878413324 ) ) ;
#55390 = CARTESIAN_POINT ( 'NONE',  ( 177.9932344209848623, 252.8631895712235576, -164.8680862452318934 ) ) ;
#55391 = CARTESIAN_POINT ( 'NONE',  ( 39.31859167701078661, -276.4317044675041757, -265.4428702740854078 ) ) ;
#55392 = CARTESIAN_POINT ( 'NONE',  ( -35.86075138741976787, -299.4956160365115352, -193.9499916391053773 ) ) ;
#55393 = ORIENTED_EDGE ( 'NONE', *, *, #6101, .F. ) ;
#55394 = CARTESIAN_POINT ( 'NONE',  ( 156.1711712139736505, 21.00000000000000000, -14.59590564729795226 ) ) ;
#55395 = CARTESIAN_POINT ( 'NONE',  ( 1.486910614065003466, -289.5994750476927493, -332.5428280042053757 ) ) ;
#55396 = CARTESIAN_POINT ( 'NONE',  ( 15.99091625240357395, -290.0692590247060139, -324.5601440855464830 ) ) ;
#55397 = CARTESIAN_POINT ( 'NONE',  ( -101.7368629529239428, -289.4282941926513786, -305.0684018471576451 ) ) ;
#55398 = CARTESIAN_POINT ( 'NONE',  ( -83.23414282389853724, -284.9502863602965022, -208.5418669721679521 ) ) ;
#55399 = CARTESIAN_POINT ( 'NONE',  ( 6.793877929583397979, -58.98313164763600724, -354.7002343187792803 ) ) ;
#55400 = CARTESIAN_POINT ( 'NONE',  ( -3.269961521395382764, -280.9942813555045404, -335.8394410721698478 ) ) ;
#55401 = CARTESIAN_POINT ( 'NONE',  ( 32.12216389915990078, -289.0672458292703482, -244.0314622169746315 ) ) ;
#55402 = CARTESIAN_POINT ( 'NONE',  ( -71.74959689872466129, -281.9954652854672190, -335.5286282438998455 ) ) ;
#55403 = CARTESIAN_POINT ( 'NONE',  ( -107.5830224914130753, -279.5808595420816687, -292.1508377993539511 ) ) ;
#55404 = CARTESIAN_POINT ( 'NONE',  ( -91.00879535272413534, -278.3323750928786353, -320.0112203473791510 ) ) ;
#55405 = CARTESIAN_POINT ( 'NONE',  ( -98.72023481205707185, -288.7339307275170199, -316.2160364199178844 ) ) ;
#55406 = CARTESIAN_POINT ( 'NONE',  ( -110.0685433276176042, -285.0418659927611316, -295.1596078263626737 ) ) ;
#55407 = CARTESIAN_POINT ( 'NONE',  ( -109.2432041649214085, -284.6959570722593753, -297.8902037638685556 ) ) ;
#55408 = CARTESIAN_POINT ( 'NONE',  ( 32.96001963823315606, -281.9787327190362021, -290.0249986376510947 ) ) ;
#55409 = VERTEX_POINT ( 'NONE', #48942 ) ;
#55410 = CARTESIAN_POINT ( 'NONE',  ( 193.6552470326849402, 275.5000000000000568, 16.89672165344822119 ) ) ;
#55411 = CARTESIAN_POINT ( 'NONE',  ( -111.6517927650008914, -292.2239280562962449, -285.2022837483743274 ) ) ;
#55412 = CARTESIAN_POINT ( 'NONE',  ( -94.33269609112210219, -289.9338557518891548, -219.3187370387785791 ) ) ;
#55413 = CARTESIAN_POINT ( 'NONE',  ( 34.85964460119316755, -274.4486703780240759, -258.0238429230757333 ) ) ;
#55414 = EDGE_CURVE ( 'NONE', #79053, #2187, #6157, .T. ) ;
#55415 = CARTESIAN_POINT ( 'NONE',  ( -61.56733123551180853, -294.7072671766154599, -343.3991914521322997 ) ) ;
#55416 = CARTESIAN_POINT ( 'NONE',  ( -68.07283883817619596, -290.1210344938378398, -203.3673712090817105 ) ) ;
#55417 = CARTESIAN_POINT ( 'NONE',  ( -56.08122799540302594, -293.5365395150099062, -342.0159378641242256 ) ) ;
#55418 = CARTESIAN_POINT ( 'NONE',  ( -23.69638451457892003, -290.0791089596519328, -342.5306143589440921 ) ) ;
#55419 = CARTESIAN_POINT ( 'NONE',  ( -110.9666534002643488, -292.7367265566448395, -255.9984047818169586 ) ) ;
#55420 = CARTESIAN_POINT ( 'NONE',  ( 19.02128324634172074, -290.8620007670184577, -220.6099585487555714 ) ) ;
#55421 = CARTESIAN_POINT ( 'NONE',  ( -70.20133459584216951, -297.4852658003967463, -337.7935247217671417 ) ) ;
#55422 = CARTESIAN_POINT ( 'NONE',  ( -83.80637592691429916, -286.3375077704160390, -213.6874246577449981 ) ) ;
#55423 = CARTESIAN_POINT ( 'NONE',  ( -52.88466988958912651, -297.2509308156264751, -343.9564859629384159 ) ) ;
#55424 = CARTESIAN_POINT ( 'NONE',  ( -21.72089202138068131, -276.2313206908625602, -196.6427542333496206 ) ) ;
#55425 = CARTESIAN_POINT ( 'NONE',  ( -68.10340025477833592, -296.8556995106122258, -199.8922526633819814 ) ) ;
#55426 = CARTESIAN_POINT ( 'NONE',  ( 30.06808866905312527, -274.1982649241995205, -300.9208036039907483 ) ) ;
#55427 = CARTESIAN_POINT ( 'NONE',  ( 16.31396394556751872, -278.9007586467985220, -218.6891601031146877 ) ) ;
#55428 = CARTESIAN_POINT ( 'NONE',  ( 9.305168264481828544, -299.9632585043001995, -196.8572638878959538 ) ) ;
#55429 = CARTESIAN_POINT ( 'NONE',  ( 33.17682165268007566, -273.7482668069132501, -240.8008472706179930 ) ) ;
#55430 = EDGE_CURVE ( 'NONE', #70449, #70176, #74194, .T. ) ;
#55431 = CARTESIAN_POINT ( 'NONE',  ( -109.4585590065431688, -297.7849363789778749, -285.0707624594489289 ) ) ;
#55432 = CARTESIAN_POINT ( 'NONE',  ( 222.4306832106270804, -134.2391364535880882, 22.50000000000000000 ) ) ;
#55433 = CARTESIAN_POINT ( 'NONE',  ( -107.9942599148068609, -297.6058988385121893, -251.3176196582970192 ) ) ;
#55434 = CARTESIAN_POINT ( 'NONE',  ( 208.4306832106271088, 0.04196010845015941959, 7.500000000000013323 ) ) ;
#55436 = CARTESIAN_POINT ( 'NONE',  ( -55.29366199708200469, -297.8148464622946676, -199.5505777150535494 ) ) ;
#55435 = CARTESIAN_POINT ( 'NONE',  ( 28.90443694933325602, -286.0482791524841559, -306.3847482653974339 ) ) ;
#55437 = CARTESIAN_POINT ( 'NONE',  ( -26.62110565877075530, -286.1848046337939877, -194.0575773621118287 ) ) ;
#55438 = CARTESIAN_POINT ( 'NONE',  ( -1.814256152264956734, -288.2611825443088378, -338.6512711244930074 ) ) ;
#55439 = CARTESIAN_POINT ( 'NONE',  ( -100.1920628284645289, -299.0910493277199294, -228.7655196365475376 ) ) ;
#55440 = CARTESIAN_POINT ( 'NONE',  ( 36.64678441054144287, -291.7006130137693276, -281.9104802602840323 ) ) ;
#55441 = CARTESIAN_POINT ( 'NONE',  ( 39.02349030844789013, -280.6367521027814860, -261.3790149900602842 ) ) ;
#55442 = PLANE ( 'NONE',  #19927 ) ;
#55443 = CARTESIAN_POINT ( 'NONE',  ( -107.9032732156323533, -276.2207428459387302, -295.9286849696143236 ) ) ;
#55444 = LINE ( 'NONE', #93171, #76185 ) ;
#55446 = EDGE_CURVE ( 'NONE', #34536, #33107, #84795, .T. ) ;
#55445 = CARTESIAN_POINT ( 'NONE',  ( -31.85691627504873225, -287.7764633198391948, -343.6038714961763390 ) ) ;
#55447 = CARTESIAN_POINT ( 'NONE',  ( 191.4749582765727212, 14.19731191252289015, 10.00000000000000000 ) ) ;
#55448 = CARTESIAN_POINT ( 'NONE',  ( -23.43874908825920755, -286.8743885594022913, -344.1143560153843168 ) ) ;
#55449 = CARTESIAN_POINT ( 'NONE',  ( -90.63755955995070224, -298.8816266153137917, -219.2390458299260558 ) ) ;
#55450 = CARTESIAN_POINT ( 'NONE',  ( -1.891271080300872987, -284.0171449996391857, -338.0506546526542024 ) ) ;
#55452 = CARTESIAN_POINT ( 'NONE',  ( 24.13044094101882564, -282.0979335365723273, -309.8263178026162450 ) ) ;
#55451 = CARTESIAN_POINT ( 'NONE',  ( -101.4834919000621198, -271.1644893416909667, -230.4218547814903957 ) ) ;
#55453 = CARTESIAN_POINT ( 'NONE',  ( -72.20275711917136618, -275.0071378488802907, -205.4962965694338664 ) ) ;
#55454 = CARTESIAN_POINT ( 'NONE',  ( -9.624544997989836759, -282.4144454984723325, -200.6706598049773334 ) ) ;
#55455 = CARTESIAN_POINT ( 'NONE',  ( -89.45227716404559715, -272.2167422993282457, -218.7984004980284567 ) ) ;
#55456 = ORIENTED_EDGE ( 'NONE', *, *, #24948, .T. ) ;
#55457 = CARTESIAN_POINT ( 'NONE',  ( 204.8711143770183014, 294.6098302808098879, -54.00000000003475265 ) ) ;
#55458 = CARTESIAN_POINT ( 'NONE',  ( -69.50601791590636935, -287.6066210947611808, -202.9875059202372540 ) ) ;
#55459 = DIRECTION ( 'NONE',  ( -1.000000000000000000, 0.000000000000000000, -0.000000000000000000 ) ) ;
#55461 = AXIS2_PLACEMENT_3D ( 'NONE', #52901, #7957, #878 ) ;
#55460 = CARTESIAN_POINT ( 'NONE',  ( 44.71564893372296723, -273.0523547857346784, -270.3937649182068412 ) ) ;
#55462 = CARTESIAN_POINT ( 'NONE',  ( -71.50825514478027856, -276.6891662247812178, -339.1855710464828348 ) ) ;
#55463 = CARTESIAN_POINT ( 'NONE',  ( -75.28321270252008901, -287.9490731754092394, -336.4435062504490475 ) ) ;
#55464 = CARTESIAN_POINT ( 'NONE',  ( -66.81929725816203813, -284.9656697739501965, -337.9157592584721783 ) ) ;
#55465 =( BOUNDED_CURVE ( )  B_SPLINE_CURVE ( 2, ( #82439, #11405, #41677, #35544, #63507, #42139, #43102, #86170, #21321, #85250, #18, #35056, #91866, #85711, #48310, #84761, #20397, #93283, #28896, #56387, #27979, #42615, #34131, #84294, #71533, #77211, #63035, #34597, #12339, #41186, #19444, #56869, #5262, #92335, #77688, #14244, #70125, #5722, #27020, #13767, #49727, #6189, #6666, #55909, #63975, #50192, #19911, #27490, #79094, #35996, #78163, #71057, #48782, #78624, #64457, #28435, #12839, #70595, #72009, #57328, #7126, #49268, #20856, #64915, #13301, #92816, #65372, #66286, #952, #29830, #50675, #23648, #1399, #80463, #58713, #65844, #86633, #22703, #8952, #87557, #51128, #30286, #15151, #43557, #72453, #51577, #21801, #59173, #79561, #37832, #88018, #15611, #29370, #14704, #483, #44483, #72909, #8498, #36457, #8034, #22255, #74292, #58262, #23173, #16084, #36930, #73388, #37376, #52056, #80939, #44937, #80011, #73838, #9416, #66738, #1864, #87105, #38302, #30755, #44011, #59657, #88501, #67217 ),
 .UNSPECIFIED., .F., .F. ) 
 B_SPLINE_CURVE_WITH_KNOTS ( ( 3, 2, 2, 2, 2, 2, 2, 2, 2, 2, 2, 2, 2, 2, 2, 2, 2, 2, 2, 2, 2, 2, 2, 2, 2, 2, 2, 2, 2, 2, 2, 2, 2, 2, 2, 2, 2, 2, 2, 2, 2, 2, 2, 2, 2, 2, 2, 2, 2, 2, 2, 2, 2, 2, 2, 2, 2, 2, 2, 2, 2, 3 ),
 ( -0.05135551144988961814, 0.000000000000000000, 0.01428571428571429047, 0.02857142857142856707, 0.04285714285714285754, 0.05714285714285713413, 0.07142857142857142461, 0.08571428571428571508, 0.09999999999999997780, 0.1142857142857142960, 0.1285714285714285587, 0.1428571428571428492, 0.1571428571428571397, 0.1714285714285714302, 0.1857142857142857206, 0.2000000000000000389, 0.2142857142857142738, 0.2285714285714285643, 0.2428571428571429103, 0.2571428571428571175, 0.2714285714285714635, 0.2857142857142856984, 0.3000000000000000444, 0.3142857142857142794, 0.3285714285714286254, 0.3428571428571428603, 0.3571428571428572063, 0.3714285714285714413, 0.3857142857142857872, 0.4000000000000000222, 0.4142857142857143682, 0.4285714285714286031, 0.4428571428571428381, 0.4571428571428571841, 0.4714285714285714191, 0.4857142857142857650, 0.5000000000000000000, 0.5142857142857142350, 0.5285714285714285809, 0.5428571428571428159, 0.5571428571428571619, 0.5714285714285713969, 0.5857142857142857428, 0.5999999999999999778, 0.6142857142857143238, 0.6285714285714285587, 0.6428571428571429047, 0.6571428571428571397, 0.6714285714285713746, 0.6857142857142857206, 0.6999999999999999556, 0.7142857142857143016, 0.7285714285714285365, 0.7428571428571428825, 0.7571428571428571175, 0.7714285714285714635, 0.7857142857142856984, 0.8000000000000000444, 0.8142857142857142794, 0.8285714285714287364, 0.8428571428571428603, 0.8500000000000000888 ),
 .UNSPECIFIED. ) 
 CURVE ( )  GEOMETRIC_REPRESENTATION_ITEM ( )  RATIONAL_B_SPLINE_CURVE ( ( 1.000000000000000000, 1.000000000000000000, 1.000000000000000000, 0.9749279121818236193, 1.000000000000000000, 0.9749279121818236193, 1.000000000000000000, 0.9749279121818236193, 1.000000000000000000, 0.9749279121818236193, 1.000000000000000000, 0.9749279121818236193, 1.000000000000000000, 0.9749279121818236193, 1.000000000000000000, 0.9749279121818236193, 1.000000000000000000, 0.9749279121818236193, 1.000000000000000000, 0.9749279121818236193, 1.000000000000000000, 0.9749279121818236193, 1.000000000000000000, 0.9749279121818236193, 1.000000000000000000, 0.9749279121818236193, 1.000000000000000000, 0.9749279121818236193, 1.000000000000000000, 0.9749279121818236193, 1.000000000000000000, 0.9749279121818236193, 1.000000000000000000, 0.9749279121818236193, 1.000000000000000000, 0.9749279121818236193, 1.000000000000000000, 0.9749279121818236193, 1.000000000000000000, 0.9749279121818236193, 1.000000000000000000, 0.9749279121818236193, 1.000000000000000000, 0.9749279121818236193, 1.000000000000000000, 0.9749279121818236193, 1.000000000000000000, 0.9749279121818236193, 1.000000000000000000, 0.9749279121818236193, 1.000000000000000000, 0.9749279121818236193, 1.000000000000000000, 0.9749279121818236193, 1.000000000000000000, 0.9749279121818236193, 1.000000000000000000, 0.9749279121818236193, 1.000000000000000000, 0.9749279121818236193, 1.000000000000000000, 0.9749279121818236193, 1.000000000000000000, 0.9749279121818236193, 1.000000000000000000, 0.9749279121818236193, 1.000000000000000000, 0.9749279121818236193, 1.000000000000000000, 0.9749279121818236193, 1.000000000000000000, 0.9749279121818236193, 1.000000000000000000, 0.9749279121818236193, 1.000000000000000000, 0.9749279121818236193, 1.000000000000000000, 0.9749279121818236193, 1.000000000000000000, 0.9749279121818236193, 1.000000000000000000, 0.9749279121818236193, 1.000000000000000000, 0.9749279121818236193, 1.000000000000000000, 0.9749279121818236193, 1.000000000000000000, 0.9749279121818236193, 1.000000000000000000, 0.9749279121818236193, 1.000000000000000000, 0.9749279121818236193, 1.000000000000000000, 0.9749279121818236193, 1.000000000000000000, 0.9749279121818236193, 1.000000000000000000, 0.9749279121818236193, 1.000000000000000000, 0.9749279121818236193, 1.000000000000000000, 0.9749279121818236193, 1.000000000000000000, 0.9749279121818236193, 1.000000000000000000, 0.9749279121818236193, 1.000000000000000000, 0.9749279121818236193, 1.000000000000000000, 0.9749279121818236193, 1.000000000000000000, 0.9749279121818236193, 1.000000000000000000, 0.9749279121818236193, 1.000000000000000000, 0.9749279121818236193, 1.000000000000000000, 0.9749279121818236193, 1.000000000000000000, 0.9749279121818236193, 1.000000000000000000, 0.9874639560909115321, 0.9874639560909117542 ) ) 
 REPRESENTATION_ITEM ( '' )  );
#55466 = CARTESIAN_POINT ( 'NONE',  ( 3.594608448287563096, -278.0913826659201504, -331.7668103410704816 ) ) ;
#55467 = CARTESIAN_POINT ( 'NONE',  ( -107.6775978405456016, -285.5928995964299588, -300.3538581988019587 ) ) ;
#55468 = CARTESIAN_POINT ( 'NONE',  ( -10.84667839444351856, -281.4938731697979506, -338.8630986575993802 ) ) ;
#55469 = CARTESIAN_POINT ( 'NONE',  ( 18.53634522016949404, -282.8556198287805046, -220.3346779906016764 ) ) ;
#55470 = CARTESIAN_POINT ( 'NONE',  ( -35.52591442282115963, -274.2409939280164508, -193.3694003170991209 ) ) ;
#55471 = CARTESIAN_POINT ( 'NONE',  ( -11.86818737651423916, -276.5629683692066578, -343.0813416925631145 ) ) ;
#55472 =( BOUNDED_SURFACE ( )  B_SPLINE_SURFACE ( 3, 2, ( 
 ( #74509, #51438, #3476 ),
 ( #81604, #9640, #25254 ),
 ( #16752, #39903, #68824 ),
 ( #3954, #15011, #45607 ),
 ( #43870, #38527, #7890 ),
 ( #84866, #34237, #47482 ) ),
 .UNSPECIFIED., .F., .F., .F. ) 
 B_SPLINE_SURFACE_WITH_KNOTS ( ( 4, 2, 4 ),
 ( 3, 3 ),
 ( -1.292368989602721285E-16, 0.001862880473700399137, 0.003725760947400927510 ),
 ( 0.000000000000000000, 1.000000000000000000 ),
 .UNSPECIFIED. ) 
 GEOMETRIC_REPRESENTATION_ITEM ( )  RATIONAL_B_SPLINE_SURFACE ( (
 ( 1.000000000000000000, 0.7071067811865238140, 1.000000000000000000),
 ( 1.000000000000000000, 0.7252627170954408786, 1.000000000000000000),
 ( 1.000000000000000000, 0.7411712618955165199, 1.000000000000000000),
 ( 1.000000000000000000, 0.7689234021729055568, 1.000000000000000000),
 ( 1.000000000000000000, 0.7808378870534314897, 1.000000000000000000),
 ( 1.000000000000000000, 0.7905694150420944366, 1.000000000000000000) ) ) 
 REPRESENTATION_ITEM ( '' )  SURFACE ( )  );
#55473 = CARTESIAN_POINT ( 'NONE',  ( -102.7205993646781934, -297.9958500886361890, -305.9548495919689799 ) ) ;
#55474 = CARTESIAN_POINT ( 'NONE',  ( 138.6539576904058606, 275.0000000000000568, -10.49999999999999822 ) ) ;
#55475 = LINE ( 'NONE', #19474, #87375 ) ;
#55476 = CARTESIAN_POINT ( 'NONE',  ( -107.7320901837979932, -295.0546827823979470, -242.1934993061658190 ) ) ;
#55477 = CARTESIAN_POINT ( 'NONE',  ( 34.43512935225187022, -274.8800081481237498, -256.7201799077768669 ) ) ;
#55478 = CARTESIAN_POINT ( 'NONE',  ( -14.93625191785613460, -299.4061590513995839, -193.6662267349441890 ) ) ;
#55479 = CARTESIAN_POINT ( 'NONE',  ( 31.91498412446033939, -288.9669872684551706, -244.1112805909705230 ) ) ;
#55480 = CARTESIAN_POINT ( 'NONE',  ( 25.94760616720495960, -295.6389878986219060, -312.9894121227993082 ) ) ;
#55481 = CARTESIAN_POINT ( 'NONE',  ( 26.19104245480922444, -295.3239925013591005, -313.1583064233602158 ) ) ;
#55482 = CARTESIAN_POINT ( 'NONE',  ( -101.8722935725086955, -292.0435366293702373, -308.3554825400511845 ) ) ;
#55483 = CARTESIAN_POINT ( 'NONE',  ( -3.496160583036511671, -278.4997593273849930, -203.6047763549147760 ) ) ;
#55484 = CARTESIAN_POINT ( 'NONE',  ( -106.8678382121186416, -280.8223266964639038, -243.6190552837798293 ) ) ;
#55485 = CARTESIAN_POINT ( 'NONE',  ( -76.43470201132666375, -293.6588031990233389, -333.7698735089981028 ) ) ;
#55486 = CARTESIAN_POINT ( 'NONE',  ( -27.50855455054090726, -284.7890556680354166, -345.5376198938438392 ) ) ;
#55487 = CARTESIAN_POINT ( 'NONE',  ( -106.8208824783783228, -283.7836976823479063, -246.8170190287729895 ) ) ;
#55488 = CARTESIAN_POINT ( 'NONE',  ( 66.71607493782951792, 46.51903866668713761, -318.0724619622529872 ) ) ;
#55489 = ORIENTED_EDGE ( 'NONE', *, *, #90062, .F. ) ;
#55490 = CARTESIAN_POINT ( 'NONE',  ( -73.56243245377845597, -285.2240150428240213, -206.9419965642647412 ) ) ;
#55491 = ORIENTED_EDGE ( 'NONE', *, *, #27827, .F. ) ;
#55492 = TOROIDAL_SURFACE ( 'NONE', #47890, 2.500000000000009770, 0.5000000000000000000 ) ;
#55493 = CARTESIAN_POINT ( 'NONE',  ( 13.48624932932764153, -283.4401334733751128, -327.8601380250025841 ) ) ;
#55494 = CARTESIAN_POINT ( 'NONE',  ( -35.39401571080843922, -274.4105157603730731, -197.3534446868073360 ) ) ;
#55495 = CARTESIAN_POINT ( 'NONE',  ( -65.71594498117595151, -284.4841220575337388, -199.1929026543034524 ) ) ;
#55496 = CARTESIAN_POINT ( 'NONE',  ( -41.00918210546713993, -280.9483383741807643, -193.6709142031657223 ) ) ;
#55497 = CARTESIAN_POINT ( 'NONE',  ( 9.339199855150265961, -212.1443419142231051, 22.50000000000000000 ) ) ;
#55498 = CARTESIAN_POINT ( 'NONE',  ( -14.77608751163456624, -278.2852054993145430, -343.3102098040038754 ) ) ;
#55499 = CARTESIAN_POINT ( 'NONE',  ( -45.27112193987900923, -280.6057585057944266, -193.8200478499758219 ) ) ;
#55500 = CARTESIAN_POINT ( 'NONE',  ( 7.450504543161054372, -278.1952119285919025, -214.2458315076590907 ) ) ;
#55501 = CARTESIAN_POINT ( 'NONE',  ( 122.6214869821080811, 149.1237144905377932, -263.6315619574343145 ) ) ;
#55502 = ORIENTED_EDGE ( 'NONE', *, *, #92308, .F. ) ;
#55503 = CARTESIAN_POINT ( 'NONE',  ( 16.75491512059070942, -276.8239737314698345, -218.5794173880239271 ) ) ;
#55504 = CARTESIAN_POINT ( 'NONE',  ( 138.3973862054802737, 180.7445933655617978, -241.2771218006182039 ) ) ;
#55505 = CARTESIAN_POINT ( 'NONE',  ( -108.7944505226338947, -276.8518797301865106, -248.7659503619966870 ) ) ;
#55506 = CARTESIAN_POINT ( 'NONE',  ( 32.38553520393038099, -294.9222933365073800, -240.1603454029673230 ) ) ;
#55507 = CARTESIAN_POINT ( 'NONE',  ( -108.0703058816943383, -295.6565544052842824, -288.8864808610924797 ) ) ;
#55508 = CARTESIAN_POINT ( 'NONE',  ( -73.39932000544710888, -291.0946126367481952, -202.3802468904231944 ) ) ;
#55509 = FACE_OUTER_BOUND ( 'NONE', #40887, .T. ) ;
#55511 = CARTESIAN_POINT ( 'NONE',  ( 35.06513564341257450, -286.1391030515925422, -284.6983745206543972 ) ) ;
#55510 = CARTESIAN_POINT ( 'NONE',  ( -113.0156614526297290, -295.2614842633988701, -259.6808898944332213 ) ) ;
#55512 = CARTESIAN_POINT ( 'NONE',  ( 26.87280497923282852, -295.9150488210141248, -307.6084375127143176 ) ) ;
#55513 = CARTESIAN_POINT ( 'NONE',  ( -89.23069155448426670, -285.1159819910635633, -322.4784343670461340 ) ) ;
#55514 = ORIENTED_EDGE ( 'NONE', *, *, #75328, .F. ) ;
#55515 = CARTESIAN_POINT ( 'NONE',  ( -64.31738168574405279, -292.6499734411429472, -198.4362540265437929 ) ) ;
#55516 = CARTESIAN_POINT ( 'NONE',  ( 9.953300776215803225, -282.8724606098635945, -326.1158162903707307 ) ) ;
#55517 = CARTESIAN_POINT ( 'NONE',  ( -110.8387786517707809, -295.0743203415212861, -291.9988081994144977 ) ) ;
#55518 = CARTESIAN_POINT ( 'NONE',  ( -111.4796996524113268, -291.6089736175756002, -250.1191914034936588 ) ) ;
#55519 = CARTESIAN_POINT ( 'NONE',  ( -62.73741867947213535, -289.8662440842581987, -343.0437894202646021 ) ) ;
#55520 = CARTESIAN_POINT ( 'NONE',  ( 16.01241423388361440, -288.4360963772322748, -320.2581557606845877 ) ) ;
#55521 = ORIENTED_EDGE ( 'NONE', *, *, #21095, .T. ) ;
#55522 = CARTESIAN_POINT ( 'NONE',  ( 169.2744399300530347, 8.542400036368780647, 10.00000000000000000 ) ) ;
#55523 = CARTESIAN_POINT ( 'NONE',  ( -87.76542100751417763, -297.6078110243569768, -326.9801367653643069 ) ) ;
#55524 = CARTESIAN_POINT ( 'NONE',  ( -106.0629662370787543, -295.6715756371194175, -236.7354454123922949 ) ) ;
#55525 = CARTESIAN_POINT ( 'NONE',  ( 31.29500917669439275, -280.2695869896268164, -244.6732345817005978 ) ) ;
#55526 = VERTEX_POINT ( 'NONE', #84444 ) ;
#55527 = EDGE_CURVE ( 'NONE', #88648, #41136, #1682, .T. ) ;
#55528 = CARTESIAN_POINT ( 'NONE',  ( 36.52854623391771582, -274.7877249209018373, -248.6641078151613726 ) ) ;
#55529 = CARTESIAN_POINT ( 'NONE',  ( -93.25796935765919216, -295.7091383813242942, -222.3408959508808493 ) ) ;
#55530 = CARTESIAN_POINT ( 'NONE',  ( -16.00353612843884576, -278.6338251294960742, -341.5174078355344136 ) ) ;
#55531 = CARTESIAN_POINT ( 'NONE',  ( -38.07112242273067437, -272.1825007806498320, -196.1294978547597054 ) ) ;
#55532 = CARTESIAN_POINT ( 'NONE',  ( -97.50008032437499139, -297.1740657082341386, -312.4098967690163136 ) ) ;
#55533 = CARTESIAN_POINT ( 'NONE',  ( -65.70495337640026889, -298.7518997724627070, -202.7611776031480417 ) ) ;
#55534 = FACE_OUTER_BOUND ( 'NONE', #41508, .T. ) ;
#55535 = CARTESIAN_POINT ( 'NONE',  ( -88.05763163336409605, -297.3475653679960828, -327.3030695434280801 ) ) ;
#55536 = CARTESIAN_POINT ( 'NONE',  ( -4.388251233285046737, -296.4635845200466520, -195.2056462083211841 ) ) ;
#55537 = CARTESIAN_POINT ( 'NONE',  ( -88.00720874947627692, -291.9722842573880257, -217.5948646665382853 ) ) ;
#55538 = CARTESIAN_POINT ( 'NONE',  ( -84.19030521499225017, -289.9677289119507577, -213.6109363365657714 ) ) ;
#55539 = DIRECTION ( 'NONE',  ( -0.000000000000000000, -1.000000000000000000, -0.000000000000000000 ) ) ;
#55540 = CARTESIAN_POINT ( 'NONE',  ( 25.27316682631609268, -275.4515324645817600, -225.6294632512385192 ) ) ;
#55541 = CARTESIAN_POINT ( 'NONE',  ( -96.90244113493012890, -297.4751434899372953, -228.1165252217108446 ) ) ;
#55542 = CARTESIAN_POINT ( 'NONE',  ( 0.5251509340085595001, -282.5336657128820548, -205.1518274706764089 ) ) ;
#55543 = CARTESIAN_POINT ( 'NONE',  ( 21.60154766256311731, -279.5771174516640372, -221.5862083013473978 ) ) ;
#55544 = CARTESIAN_POINT ( 'NONE',  ( -82.49314110336433714, -276.9996492523249572, -332.6078862854157592 ) ) ;
#55545 = CARTESIAN_POINT ( 'NONE',  ( 22.71148703111292377, -281.3304858494317386, -312.1488726383479388 ) ) ;
#55546 = CARTESIAN_POINT ( 'NONE',  ( 29.43646660842806995, -280.0076609225698689, -304.8677096843214827 ) ) ;
#55547 = ADVANCED_FACE ( 'NONE', ( #92018 ), #51550, .T. ) ;
#55548 = CARTESIAN_POINT ( 'NONE',  ( 17.73855798917262305, -273.4344786995096115, -221.4845631202330765 ) ) ;
#55549 = CARTESIAN_POINT ( 'NONE',  ( -91.90764182733370546, -281.2742061657593808, -218.8322374065569988 ) ) ;
#55550 = CARTESIAN_POINT ( 'NONE',  ( 156.4851178187871312, 15.00000000000000000, 7.000000000000000888 ) ) ;
#55551 = LINE ( 'NONE', #5370, #26154 ) ;
#55552 = CARTESIAN_POINT ( 'NONE',  ( 18.48403035578103015, -296.9817873043560894, -194.3908963028880237 ) ) ;
#55553 = CARTESIAN_POINT ( 'NONE',  ( -111.2321641310948763, -290.8238438703999691, -248.7001085550341202 ) ) ;
#55554 = EDGE_CURVE ( 'NONE', #5766, #85835, #47991, .T. ) ;
#55555 = CARTESIAN_POINT ( 'NONE',  ( 36.11951409089245146, -277.7570510648502591, -286.3423530635178054 ) ) ;
#55556 = CARTESIAN_POINT ( 'NONE',  ( -13.40362284056542563, -272.3628528587607889, -199.2839127544727091 ) ) ;
#55557 = CARTESIAN_POINT ( 'NONE',  ( 193.2782748703399420, 250.0348692542015385, 16.89756558802352870 ) ) ;
#55558 = CARTESIAN_POINT ( 'NONE',  ( -109.7214204775096533, -286.1943910878828774, -292.0967853559159266 ) ) ;
#55559 = ORIENTED_EDGE ( 'NONE', *, *, #53042, .T. ) ;
#55560 = CARTESIAN_POINT ( 'NONE',  ( 155.8055003384352801, 17.52828139914646499, -8.087387968560612705 ) ) ;
#55561 = CARTESIAN_POINT ( 'NONE',  ( -40.83110399604597518, -287.0958686692045490, -345.2925181388677061 ) ) ;
#55562 = CARTESIAN_POINT ( 'NONE',  ( 202.9738562182569694, 293.9636489450776367, -54.00000000000000000 ) ) ;
#55563 = CARTESIAN_POINT ( 'NONE',  ( 12.61395769135607736, -293.1322295059306384, -324.2040166919188096 ) ) ;
#55564 = CARTESIAN_POINT ( 'NONE',  ( 11.97198968448825873, -284.8853739300199095, -214.8030651670278814 ) ) ;
#55565 = CARTESIAN_POINT ( 'NONE',  ( 156.6530531571843028, 18.17946993580008197, -9.832064661606517930 ) ) ;
#55566 = CARTESIAN_POINT ( 'NONE',  ( -2.229372256407885722, -292.5872080975239555, -336.6342277833913954 ) ) ;
#55567 = CARTESIAN_POINT ( 'NONE',  ( -33.74050798617618341, -284.5765813893596032, -194.1394729668528214 ) ) ;
#55568 = CARTESIAN_POINT ( 'NONE',  ( -34.30053951456762462, -281.6911172414450562, -196.6111209455514768 ) ) ;
#55569 = CARTESIAN_POINT ( 'NONE',  ( 25.21194345192014552, -288.1687898585081484, -226.1225567101169815 ) ) ;
#55570 = CARTESIAN_POINT ( 'NONE',  ( 38.69654786586400519, -279.7869057944955102, -269.9583100898284442 ) ) ;
#55571 = CARTESIAN_POINT ( 'NONE',  ( -48.06098284628401274, -289.1921850050840703, -342.6208443211500025 ) ) ;
#55572 = CARTESIAN_POINT ( 'NONE',  ( -11.55353154165473661, -281.8198655261309682, -201.3844866885457634 ) ) ;
#55573 = CARTESIAN_POINT ( 'NONE',  ( -59.79288494713743063, -280.5567011948643312, -200.6761909063671396 ) ) ;
#55574 = CARTESIAN_POINT ( 'NONE',  ( 11.00262234227823299, -288.6968189920589793, -212.4896453108611922 ) ) ;
#55575 = ORIENTED_EDGE ( 'NONE', *, *, #74260, .T. ) ;
#55576 = CARTESIAN_POINT ( 'NONE',  ( -5.114264152580068057, -274.4647670537403883, -200.4297775803843535 ) ) ;
#55577 = CARTESIAN_POINT ( 'NONE',  ( -105.5404452068812304, -292.1310368509668365, -300.8329939880798634 ) ) ;
#55578 = CARTESIAN_POINT ( 'NONE',  ( 207.5211292351690417, 36.67813790105583394, 13.69055975427937000 ) ) ;
#55579 = CARTESIAN_POINT ( 'NONE',  ( -19.05039376806008633, -297.3376638359844719, -350.3538533559490702 ) ) ;
#55580 = VERTEX_POINT ( 'NONE', #6335 ) ;
#55581 = CARTESIAN_POINT ( 'NONE',  ( 24.64741721620444181, -272.9770163691381413, -227.8250279221243204 ) ) ;
#55582 = DIRECTION ( 'NONE',  ( 0.000000000000000000, 0.000000000000000000, 1.000000000000000000 ) ) ;
#55583 = CARTESIAN_POINT ( 'NONE',  ( -70.47859530821351370, -293.8815144607628440, -338.9931630804020983 ) ) ;
#55584 = CARTESIAN_POINT ( 'NONE',  ( -102.1169269822903090, -272.3625217312203404, -236.3684310538140210 ) ) ;
#55585 = CARTESIAN_POINT ( 'NONE',  ( 32.98102004045814795, -289.3635330527375231, -292.5634128866782930 ) ) ;
#55586 = CARTESIAN_POINT ( 'NONE',  ( 24.99586053098165905, -283.8577910119429362, -310.3552836523294900 ) ) ;
#55587 = CARTESIAN_POINT ( 'NONE',  ( -51.55775109786338817, -290.6558347610954911, -345.4378133426385489 ) ) ;
#55588 = CARTESIAN_POINT ( 'NONE',  ( -100.2654114290711505, -291.2888686213889855, -313.8801348498201378 ) ) ;
#55589 = CARTESIAN_POINT ( 'NONE',  ( -57.96822921182693023, -287.7860059551414338, -198.1991730765212480 ) ) ;
#55590 = CARTESIAN_POINT ( 'NONE',  ( -101.8923791302096191, -279.2712278385557170, -228.2859501127942679 ) ) ;
#55591 = CARTESIAN_POINT ( 'NONE',  ( -103.3569439115035209, -294.1451416631172719, -307.2281958411635969 ) ) ;
#55592 = CARTESIAN_POINT ( 'NONE',  ( -1.636023932056818397, -282.4254500264314061, -338.5821168898514770 ) ) ;
#55593 = CARTESIAN_POINT ( 'NONE',  ( -3.563451093186552843, -276.3632319589444251, -204.2416654072322899 ) ) ;
#55594 = CARTESIAN_POINT ( 'NONE',  ( 7.399455738971494334, -283.1948066931273615, -214.2051214447836571 ) ) ;
#55595 = CARTESIAN_POINT ( 'NONE',  ( 36.65334540946774666, -273.5723328426788044, -253.0212941062590062 ) ) ;
#55596 = CARTESIAN_POINT ( 'NONE',  ( 133.0872704186301405, -299.5541904835127980, -189.2068768330456123 ) ) ;
#55597 = CARTESIAN_POINT ( 'NONE',  ( 35.48981690850820314, -281.1441792772546933, -276.7627667117184274 ) ) ;
#55598 = CARTESIAN_POINT ( 'NONE',  ( -105.9827270148045386, -279.3165397582349101, -304.4865625263158222 ) ) ;
#55599 = CARTESIAN_POINT ( 'NONE',  ( -3.581989427031941897, -285.5455876395546397, -201.4038876781254714 ) ) ;
#55600 = CARTESIAN_POINT ( 'NONE',  ( -75.52128544669649557, -293.2959112135206396, -206.8954906990949780 ) ) ;
#55601 = CARTESIAN_POINT ( 'NONE',  ( -29.93710617173993427, -275.7445226842622219, -194.5217324153228446 ) ) ;
#55602 = CARTESIAN_POINT ( 'NONE',  ( -21.47352411282671980, -275.5667094868534832, -195.5179535560141630 ) ) ;
#55603 = CARTESIAN_POINT ( 'NONE',  ( 33.58602562233892286, -275.6139639127588339, -287.6839082804112877 ) ) ;
#55604 = CARTESIAN_POINT ( 'NONE',  ( -68.02417613890577286, -297.4560484359759585, -338.6292065791885761 ) ) ;
#55605 = CARTESIAN_POINT ( 'NONE',  ( -112.0570084947017477, -282.6168989365954189, -265.3168681408515113 ) ) ;
#55606 = CARTESIAN_POINT ( 'NONE',  ( 11.10877385490507407, -292.3684952848250873, -210.4736760558672017 ) ) ;
#55607 = CARTESIAN_POINT ( 'NONE',  ( 23.63878784852626680, -272.9843932777092732, -227.2898600109737686 ) ) ;
#55608 = CARTESIAN_POINT ( 'NONE',  ( -17.90848375983574314, -290.4057607847047393, -344.0414444956037414 ) ) ;
#55609 = CARTESIAN_POINT ( 'NONE',  ( -17.33508574209895059, -291.2366728098951967, -199.7819822093789242 ) ) ;
#55610 = ORIENTED_EDGE ( 'NONE', *, *, #54326, .T. ) ;
#55611 = CARTESIAN_POINT ( 'NONE',  ( -14.02882395874058830, -290.9233845878376883, -197.5380184614061818 ) ) ;
#55612 = CARTESIAN_POINT ( 'NONE',  ( -105.1342552513342952, -289.8541907227410093, -297.6309001967361496 ) ) ;
#55613 = ORIENTED_EDGE ( 'NONE', *, *, #72108, .T. ) ;
#55614 = CARTESIAN_POINT ( 'NONE',  ( 23.90368209773672703, -289.2489040155889484, -316.5184106539559252 ) ) ;
#55615 = CARTESIAN_POINT ( 'NONE',  ( -103.1482246355916033, -278.4559834648771925, -302.1259906924534562 ) ) ;
#55616 = EDGE_CURVE ( 'NONE', #32542, #69284, #40918, .T. ) ;
#55617 = CARTESIAN_POINT ( 'NONE',  ( -39.11453006185769965, -293.9942459872765426, -347.0315137352340003 ) ) ;
#55618 = CARTESIAN_POINT ( 'NONE',  ( -64.51893673637594873, -286.3579673822758309, -198.4115071107036101 ) ) ;
#55619 = CARTESIAN_POINT ( 'NONE',  ( -110.2033003136022131, -284.5723902959645102, -295.1992239871389643 ) ) ;
#55620 = CARTESIAN_POINT ( 'NONE',  ( 3.405537827692454833, -282.8211910679626726, -331.0172508417033441 ) ) ;
#55621 = CARTESIAN_POINT ( 'NONE',  ( 203.5337727339234846, 295.8836732959281903, -68.67824016207623572 ) ) ;
#55622 = CARTESIAN_POINT ( 'NONE',  ( 192.4874460990043303, 278.9581800658359043, -125.3567854953941350 ) ) ;
#55623 = CARTESIAN_POINT ( 'NONE',  ( 120.3257472410092106, 148.3080601949953348, -260.4889484542558193 ) ) ;
#55624 = CARTESIAN_POINT ( 'NONE',  ( -0.4560453400966971160, -273.7531173004441030, -207.1638205314783931 ) ) ;
#55625 = CARTESIAN_POINT ( 'NONE',  ( 35.41109380573036702, -274.5961976119448309, -279.7796281686540283 ) ) ;
#55626 = CARTESIAN_POINT ( 'NONE',  ( -106.4552899028562933, -296.4942700314139188, -236.5552218770223760 ) ) ;
#55627 = CARTESIAN_POINT ( 'NONE',  ( 122.7515402636430224, 147.2049715914294268, -260.8663683293274289 ) ) ;
#55628 = CARTESIAN_POINT ( 'NONE',  ( 14.53640247338804770, -275.0254564862075313, -326.6645220150668933 ) ) ;
#55629 = CARTESIAN_POINT ( 'NONE',  ( -110.5888894825546629, -274.4550657320833125, -259.3883154377897995 ) ) ;
#55630 = ORIENTED_EDGE ( 'NONE', *, *, #70399, .F. ) ;
#55631 = CARTESIAN_POINT ( 'NONE',  ( -54.55409744218442825, -298.7774356042808677, -195.5510010799730480 ) ) ;
#55632 = CARTESIAN_POINT ( 'NONE',  ( 5.886078104987047865, -288.9407488534707227, -329.3253402771463243 ) ) ;
#55633 = CARTESIAN_POINT ( 'NONE',  ( -36.26643213138716249, -295.8418579235143397, -347.2051944878751897 ) ) ;
#55634 = CARTESIAN_POINT ( 'NONE',  ( -111.1545745462997417, -296.7714692090581252, -292.1144043037991764 ) ) ;
#55635 = CARTESIAN_POINT ( 'NONE',  ( -25.41118314430918801, -292.3750007293102158, -198.2911504901928481 ) ) ;
#55636 = EDGE_LOOP ( 'NONE', ( #6505, #58311, #43291, #68761, #49564 ) ) ;
#55637 = CARTESIAN_POINT ( 'NONE',  ( 11.78722809278406736, -278.2960936690671474, -327.7689798758927964 ) ) ;
#55638 = CARTESIAN_POINT ( 'NONE',  ( 33.11910213914773493, -280.6654289443937955, -239.4612434371679512 ) ) ;
#55639 = CIRCLE ( 'NONE', #7306, 2.395975569037533948 ) ;
#55640 = CARTESIAN_POINT ( 'NONE',  ( -9.889073925254171726, -277.6258911462621199, -338.2699548257710944 ) ) ;
#55641 = CARTESIAN_POINT ( 'NONE',  ( -8.251561255757351887, -278.4365837355462077, -340.5730644662727400 ) ) ;
#55642 = CARTESIAN_POINT ( 'NONE',  ( -45.49721202029022038, -275.1749793123691461, -345.3256222091466157 ) ) ;
#55643 = CARTESIAN_POINT ( 'NONE',  ( -84.14645356983561442, -298.0404107818304738, -214.1415903054838736 ) ) ;
#55644 = CARTESIAN_POINT ( 'NONE',  ( -106.3521216461459602, -295.4666160159509900, -244.6616095124171864 ) ) ;
#55645 = DIRECTION ( 'NONE',  ( -0.000000000000000000, 1.000000000000000000, -0.000000000000000000 ) ) ;
#55646 = CARTESIAN_POINT ( 'NONE',  ( -71.21315557542598640, -280.1092840815544491, -201.2796341432523093 ) ) ;
#55647 = CARTESIAN_POINT ( 'NONE',  ( 15.59934075976178747, -276.4433566139026084, -320.6228946544690643 ) ) ;
#55648 = CARTESIAN_POINT ( 'NONE',  ( -57.60906701975474675, -284.4807686903452009, -196.5326051539492767 ) ) ;
#55649 = CARTESIAN_POINT ( 'NONE',  ( -69.95714607383332861, -299.6237110336759315, -202.6391782771511600 ) ) ;
#55650 = DIRECTION ( 'NONE',  ( 1.000000000000000000, -0.000000000000000000, -0.000000000000000000 ) ) ;
#55651 = CARTESIAN_POINT ( 'NONE',  ( 17.01743078045893398, -286.0495725490682730, -221.3762336936270287 ) ) ;
#55652 = CARTESIAN_POINT ( 'NONE',  ( 11.99778753103542961, -278.9892213532961023, -215.1923861784540861 ) ) ;
#55654 = CARTESIAN_POINT ( 'NONE',  ( -43.06760934430345600, -281.2046985372259655, -344.6316517377554192 ) ) ;
#55653 = CARTESIAN_POINT ( 'NONE',  ( -41.06297474710797246, -278.5791259067076453, -196.8660362883793198 ) ) ;
#55655 = CARTESIAN_POINT ( 'NONE',  ( 23.21259941325403631, -288.9481928874927803, -226.0248794563007380 ) ) ;
#55656 = CARTESIAN_POINT ( 'NONE',  ( -108.5536175172389619, -279.5233021261240083, -288.1890860987542169 ) ) ;
#55657 = CARTESIAN_POINT ( 'NONE',  ( 153.6937476593222982, 20.34834636856922430, 12.69848024943771314 ) ) ;
#55658 = CARTESIAN_POINT ( 'NONE',  ( 3.042594796722233763, -294.5941410503118050, -207.1006052751409356 ) ) ;
#55659 = CARTESIAN_POINT ( 'NONE',  ( -74.85569394479161076, -275.7844272069818885, -336.4419342769684818 ) ) ;
#55660 = TOROIDAL_SURFACE ( 'NONE', #58709, 24.49999999999999645, 0.5000000000000000000 ) ;
#55661 = CARTESIAN_POINT ( 'NONE',  ( -26.99890439060824576, -277.5685812009255073, -342.7276796274720709 ) ) ;
#55662 = CARTESIAN_POINT ( 'NONE',  ( 36.35327034838019955, -283.7419359996447383, -285.1624610414698964 ) ) ;
#55663 = CARTESIAN_POINT ( 'NONE',  ( 83.14890176555634582, -299.5541904835127980, -195.3611179825600175 ) ) ;
#55664 = CARTESIAN_POINT ( 'NONE',  ( -48.62927324826024034, -291.1148120146132783, -345.1261981136486838 ) ) ;
#55665 = CARTESIAN_POINT ( 'NONE',  ( -98.42176093626626709, -293.9599617903735407, -313.9055724975239627 ) ) ;
#55666 = EDGE_CURVE ( 'NONE', #36954, #83022, #57014, .T. ) ;
#55667 = CARTESIAN_POINT ( 'NONE',  ( -64.48057318514403846, -284.9039561673485537, -198.4606790583654004 ) ) ;
#55668 = DIRECTION ( 'NONE',  ( -0.000000000000000000, -0.000000000000000000, -1.000000000000000000 ) ) ;
#55669 = CARTESIAN_POINT ( 'NONE',  ( -76.81508418721976739, -272.1961921824168940, -208.3684133438687525 ) ) ;
#55670 = CARTESIAN_POINT ( 'NONE',  ( -33.41988252052209418, -290.2415950093939045, -196.2168772655398925 ) ) ;
#55671 = DIRECTION ( 'NONE',  ( -1.000000000000000000, -0.000000000000000000, -0.000000000000000000 ) ) ;
#55672 = CARTESIAN_POINT ( 'NONE',  ( 200.4972393895363041, 64.43555889006553627, 7.250946725472672050 ) ) ;
#55673 = CARTESIAN_POINT ( 'NONE',  ( -34.96246114849688524, -290.5613764734843016, -194.0785186837560445 ) ) ;
#55674 = CARTESIAN_POINT ( 'NONE',  ( -18.41250031138758914, -284.5324909898027386, -196.7155727485262560 ) ) ;
#55675 = CARTESIAN_POINT ( 'NONE',  ( -73.86370777302514057, -286.9822846621844405, -206.4597448808022477 ) ) ;
#55676 = ADVANCED_FACE ( 'NONE', ( #58853 ), #42762, .F. ) ;
#55677 = CARTESIAN_POINT ( 'NONE',  ( -19.78698905443609135, -287.0865211982446681, -199.3369400883534865 ) ) ;
#55678 = CARTESIAN_POINT ( 'NONE',  ( -19.79478280444287819, -294.2564015011995480, -197.0236909666916176 ) ) ;
#55679 = CARTESIAN_POINT ( 'NONE',  ( 23.19895576365909307, -274.2449536268571251, -315.5733197082653305 ) ) ;
#55680 = CARTESIAN_POINT ( 'NONE',  ( 36.04375762715931586, -276.1776722089371674, -293.6058782860841347 ) ) ;
#55681 = CARTESIAN_POINT ( 'NONE',  ( 10.23148833066985119, -290.7818777374869228, -211.5902411261003522 ) ) ;
#55682 = CARTESIAN_POINT ( 'NONE',  ( -62.04762978673585394, -279.7397439990473913, -197.3760363536219984 ) ) ;
#55683 = CARTESIAN_POINT ( 'NONE',  ( -48.00359504862603188, -297.1681962995274375, -344.2929853756847365 ) ) ;
#55684 = CARTESIAN_POINT ( 'NONE',  ( -48.18343439339133027, -254.1872365014273782, -480.9328361744520066 ) ) ;
#55685 = DIRECTION ( 'NONE',  ( -0.000000000000000000, -1.000000000000000000, -0.000000000000000000 ) ) ;
#55686 = CARTESIAN_POINT ( 'NONE',  ( -83.94776212069248800, -284.0814448168353010, -213.4696746476450926 ) ) ;
#55687 = CARTESIAN_POINT ( 'NONE',  ( 31.71421918993832989, -279.9358960430425896, -299.7559121142176650 ) ) ;
#55688 = CARTESIAN_POINT ( 'NONE',  ( 196.1963538710216994, 282.2246705312485915, -40.00000000000000711 ) ) ;
#55689 = CARTESIAN_POINT ( 'NONE',  ( 38.93829113487036153, -274.0065691618967776, -268.3435244019307220 ) ) ;
#55690 = CARTESIAN_POINT ( 'NONE',  ( -64.37854747591299542, -276.7630070288747106, -338.3332230366665954 ) ) ;
#55691 = CARTESIAN_POINT ( 'NONE',  ( -18.02025417391305595, -296.3186316492326569, -341.4764431728233376 ) ) ;
#55692 = CARTESIAN_POINT ( 'NONE',  ( -28.24795573831202233, -279.0851709983578530, -194.1578794746408505 ) ) ;
#55693 = CARTESIAN_POINT ( 'NONE',  ( -93.25429658683719936, -296.8231378173207986, -317.6794842056817174 ) ) ;
#55694 = CARTESIAN_POINT ( 'NONE',  ( -109.8728282831767729, -297.5588150344766518, -294.7031335299384978 ) ) ;
#55695 = CARTESIAN_POINT ( 'NONE',  ( -86.09871264348110742, -297.1866082164692671, -216.0310734854319037 ) ) ;
#55696 = CARTESIAN_POINT ( 'NONE',  ( -111.9653373810833017, -292.6486687494431749, -262.8568918128862606 ) ) ;
#55697 = CARTESIAN_POINT ( 'NONE',  ( -76.10855650049418841, -285.7161634103759980, -203.7705439254983162 ) ) ;
#55698 = CARTESIAN_POINT ( 'NONE',  ( 38.47115475176315158, -273.7021723269643303, -271.1822867159073098 ) ) ;
#55699 = CARTESIAN_POINT ( 'NONE',  ( -71.90837130967148028, -289.3298041366661550, -339.1662431401754816 ) ) ;
#55700 = CARTESIAN_POINT ( 'NONE',  ( -99.37424697185159062, -281.0970458832503027, -228.7505034914514965 ) ) ;
#55701 = CARTESIAN_POINT ( 'NONE',  ( 24.43040069887143417, -287.1531027544596100, -309.7008689654628597 ) ) ;
#55702 = AXIS2_PLACEMENT_3D ( 'NONE', #43588, #92845, #22285 ) ;
#55703 = CARTESIAN_POINT ( 'NONE',  ( -50.19781756788521676, -289.8878837452321022, -196.4711938357012286 ) ) ;
#55704 = CARTESIAN_POINT ( 'NONE',  ( -107.5886556134111913, -275.3214365662247474, -283.9876634089608274 ) ) ;
#55705 = CARTESIAN_POINT ( 'NONE',  ( 15.07801039995889347, -286.3246022718897734, -219.4674799734574151 ) ) ;
#55706 = CARTESIAN_POINT ( 'NONE',  ( 198.4642567341846018, 298.3489338295183302, -6.693632019895620289 ) ) ;
#55707 = CARTESIAN_POINT ( 'NONE',  ( 32.18438806766314286, -282.9127591946071334, -303.0278025205892618 ) ) ;
#55708 = CARTESIAN_POINT ( 'NONE',  ( -108.1454784106161782, -289.9893077222147326, -240.7023049033719531 ) ) ;
#55709 = CARTESIAN_POINT ( 'NONE',  ( -39.58434629786869152, -281.6245873055125344, -194.1812092771705238 ) ) ;
#55710 = CARTESIAN_POINT ( 'NONE',  ( -113.7386667343605069, -279.8157304895464677, -274.4601135827386997 ) ) ;
#55711 = CARTESIAN_POINT ( 'NONE',  ( 15.82440590370200795, -282.1063148144999104, -320.4576903719632242 ) ) ;
#55712 = CARTESIAN_POINT ( 'NONE',  ( 36.07400187443877826, -277.3546180322813939, -254.9643979733300796 ) ) ;
#55713 = CARTESIAN_POINT ( 'NONE',  ( 4.227299072872228614, -294.5087312939130015, -335.2391569669870250 ) ) ;
#55714 = CARTESIAN_POINT ( 'NONE',  ( -105.0376438474083614, -288.9874518093317306, -238.9110622825188273 ) ) ;
#55715 = CARTESIAN_POINT ( 'NONE',  ( -69.38026857188837937, -296.5406205986563464, -204.4236005376833134 ) ) ;
#55716 = ORIENTED_EDGE ( 'NONE', *, *, #19155, .F. ) ;
#55717 = ORIENTED_EDGE ( 'NONE', *, *, #69834, .F. ) ;
#55718 = CARTESIAN_POINT ( 'NONE',  ( -111.7572433318797920, -286.4287678944498907, -273.7271644540815601 ) ) ;
#55719 = CARTESIAN_POINT ( 'NONE',  ( -39.21796628501986959, -293.1088215601851061, -193.6802010814483026 ) ) ;
#55720 = CARTESIAN_POINT ( 'NONE',  ( 22.67319087874643557, -282.7844968492826183, -312.0996556395778612 ) ) ;
#55721 = CARTESIAN_POINT ( 'NONE',  ( 37.06014482014440148, -274.3736905368810426, -251.4617613254791024 ) ) ;
#55722 = CARTESIAN_POINT ( 'NONE',  ( -73.39327764319359915, -292.2381881952337608, -202.4227762886041830 ) ) ;
#55723 = CARTESIAN_POINT ( 'NONE',  ( -110.5218504365429482, -282.9436818642863614, -250.5434911029181251 ) ) ;
#55724 = CARTESIAN_POINT ( 'NONE',  ( -37.79916431218168071, -292.3798483090299101, -193.3836211527325872 ) ) ;
#55725 = CARTESIAN_POINT ( 'NONE',  ( 27.67503360213356345, -287.4326100166892957, -237.0094317225492944 ) ) ;
#55726 = CARTESIAN_POINT ( 'NONE',  ( 180.5131398354828320, 249.5000000000000568, -23.92352941176472569 ) ) ;
#55727 = CARTESIAN_POINT ( 'NONE',  ( -74.94434090351494149, -212.1443419142231051, 54.50000000000000711 ) ) ;
#55728 = CARTESIAN_POINT ( 'NONE',  ( 65.08017568742300796, 46.23336141765577878, -315.3328154015194400 ) ) ;
#55729 = CARTESIAN_POINT ( 'NONE',  ( -27.44268967638380730, -284.4488165136957036, -346.0758614227595444 ) ) ;
#55730 = CARTESIAN_POINT ( 'NONE',  ( -85.28047601435909542, -288.9094976428777386, -210.1954327657594206 ) ) ;
#55731 = ORIENTED_EDGE ( 'NONE', *, *, #63462, .F. ) ;
#55732 = CARTESIAN_POINT ( 'NONE',  ( 34.53102223102401780, -280.6630023714232607, -284.8650735297037500 ) ) ;
#55733 = CARTESIAN_POINT ( 'NONE',  ( 22.62185884198586550, -275.8662042734623014, -318.6532404526579398 ) ) ;
#55734 = CARTESIAN_POINT ( 'NONE',  ( -21.83886583921823643, -282.2513104852705510, -197.0980541976623215 ) ) ;
#55735 = CARTESIAN_POINT ( 'NONE',  ( 155.3744588886772533, 204.7076335705557995, -215.6431656911598509 ) ) ;
#55736 = CARTESIAN_POINT ( 'NONE',  ( 38.82581658908117106, -280.0501020718857603, -264.2688533097283994 ) ) ;
#55737 = CARTESIAN_POINT ( 'NONE',  ( -110.0326981478991826, -282.3527207339477627, -287.3836503301616858 ) ) ;
#55738 = CARTESIAN_POINT ( 'NONE',  ( -113.1122788582135001, -298.3931845793690627, -263.9781883939792806 ) ) ;
#55739 = CARTESIAN_POINT ( 'NONE',  ( 34.27556952650019895, -293.8539723999066382, -255.9058376649994102 ) ) ;
#55740 = ORIENTED_EDGE ( 'NONE', *, *, #48576, .T. ) ;
#55741 = CARTESIAN_POINT ( 'NONE',  ( -55.11551891749013521, -290.5035561635493195, -199.0495842573903928 ) ) ;
#55742 = CARTESIAN_POINT ( 'NONE',  ( -28.60436878489555568, -277.5956510857978401, -346.8147002688712064 ) ) ;
#55743 = CARTESIAN_POINT ( 'NONE',  ( -99.28047840515753819, -273.0853839058438552, -231.7270948223558094 ) ) ;
#55744 = ORIENTED_EDGE ( 'NONE', *, *, #83965, .T. ) ;
#55745 = CARTESIAN_POINT ( 'NONE',  ( -3.948224698501486163, -273.4026288294535902, -201.3077763909095950 ) ) ;
#55746 = CARTESIAN_POINT ( 'NONE',  ( 160.5350683151633291, 275.0000000000000568, 20.22542485937379908 ) ) ;
#55747 = CARTESIAN_POINT ( 'NONE',  ( 201.2104617360081704, 60.19600395700749829, 10.00000000000000000 ) ) ;
#55748 = CARTESIAN_POINT ( 'NONE',  ( 155.4148940283180309, 19.61091623264239558, 11.07022379048214766 ) ) ;
#55749 = CARTESIAN_POINT ( 'NONE',  ( -8.359437159206827062, -283.7432030591600096, -337.6979912946849822 ) ) ;
#55750 = CARTESIAN_POINT ( 'NONE',  ( 37.78931172455114051, -283.1638641883933474, -258.6492710758498106 ) ) ;
#55751 = CARTESIAN_POINT ( 'NONE',  ( -110.6259620222402731, -283.6038201957822480, -270.8991039316575211 ) ) ;
#55752 = CARTESIAN_POINT ( 'NONE',  ( 32.82876002637679846, -273.6500458308333350, -247.3372971107000922 ) ) ;
#55753 = CARTESIAN_POINT ( 'NONE',  ( 3.361782054203298120, -282.4656345588975910, -208.2181152117511544 ) ) ;
#55754 = CARTESIAN_POINT ( 'NONE',  ( -7.242007727162001807, -275.1298703312037901, -337.6271292472314940 ) ) ;
#55755 = DIRECTION ( 'NONE',  ( -0.000000000000000000, -0.000000000000000000, -1.000000000000000000 ) ) ;
#55756 = CARTESIAN_POINT ( 'NONE',  ( 3.089007127703217392, -275.6885724997914622, -209.1483183521881131 ) ) ;
#55757 = CARTESIAN_POINT ( 'NONE',  ( 189.9243309297870610, 249.5000000000000568, 20.22542485937349355 ) ) ;
#55758 = CARTESIAN_POINT ( 'NONE',  ( -95.08268006545570472, -278.6674674094970214, -321.0576470220410670 ) ) ;
#55759 = ORIENTED_EDGE ( 'NONE', *, *, #63139, .T. ) ;
#55760 = ORIENTED_EDGE ( 'NONE', *, *, #66040, .T. ) ;
#55761 = CARTESIAN_POINT ( 'NONE',  ( 180.6209651459523968, 250.0000000000000568, -24.41176470588237635 ) ) ;
#55762 = CARTESIAN_POINT ( 'NONE',  ( -111.0124335009993786, -286.1870216109697367, -288.1057534714771009 ) ) ;
#55763 = CARTESIAN_POINT ( 'NONE',  ( -5.480408186216903843, -293.8191100215200890, -336.2343521740498886 ) ) ;
#55764 = CARTESIAN_POINT ( 'NONE',  ( -37.50970520695263843, -288.4027580212027715, -347.2720563524545128 ) ) ;
#55765 = CARTESIAN_POINT ( 'NONE',  ( -86.38102030887576177, -283.6005606901758824, -214.8569168338974293 ) ) ;
#55767 = CARTESIAN_POINT ( 'NONE',  ( -15.57473655852678718, -287.0065720128536668, -341.1548522733850746 ) ) ;
#55766 = CARTESIAN_POINT ( 'NONE',  ( -107.9624628954410781, -282.8548056065602623, -291.0963094781445193 ) ) ;
#55768 = AXIS2_PLACEMENT_3D ( 'NONE', #44513, #1900, #74325 ) ;
#55769 = CARTESIAN_POINT ( 'NONE',  ( -110.0074938962367526, -285.8928315151327411, -260.0260843109732605 ) ) ;
#55770 = CARTESIAN_POINT ( 'NONE',  ( 37.62310905036242303, -273.5983726887791931, -273.9737064408737979 ) ) ;
#55771 = CARTESIAN_POINT ( 'NONE',  ( -7.635997141478554795, -284.8348229458724745, -200.1337411741459107 ) ) ;
#55772 = CARTESIAN_POINT ( 'NONE',  ( -111.1748427600444558, -298.7215197931117245, -257.1828138500309251 ) ) ;
#55773 = CARTESIAN_POINT ( 'NONE',  ( -33.78790323397614515, -284.0966204425338901, -195.2785037753886854 ) ) ;
#55774 = CARTESIAN_POINT ( 'NONE',  ( 19.85228082211398259, -281.8492405191142325, -224.6199221954164216 ) ) ;
#55775 = CARTESIAN_POINT ( 'NONE',  ( -29.15101971653988500, -290.9488840420743259, -345.1324524934789792 ) ) ;
#55776 = LINE ( 'NONE', #39197, #23191 ) ;
#55777 = FACE_OUTER_BOUND ( 'NONE', #84697, .T. ) ;
#55778 = CARTESIAN_POINT ( 'NONE',  ( -58.42561724735296025, -297.2426359752225835, -342.9744673645919875 ) ) ;
#55779 = CARTESIAN_POINT ( 'NONE',  ( -82.47157427380329864, -277.4361608080855603, -210.3935417485051858 ) ) ;
#55780 = CARTESIAN_POINT ( 'NONE',  ( 33.18025448408185696, -292.3597320987174726, -239.8518941690257407 ) ) ;
#55781 = CARTESIAN_POINT ( 'NONE',  ( -94.57576155651388206, -294.2995129234390674, -316.9717853151980762 ) ) ;
#55782 = CARTESIAN_POINT ( 'NONE',  ( -87.85751897368534458, -278.0132771434929850, -216.9110740695190032 ) ) ;
#55783 = CARTESIAN_POINT ( 'NONE',  ( -100.4893558085904743, -271.1655393221718100, -230.9442715989578971 ) ) ;
#55784 = CARTESIAN_POINT ( 'NONE',  ( 33.09694854689596610, -294.5896179906439443, -249.2182908589441297 ) ) ;
#55785 = CARTESIAN_POINT ( 'NONE',  ( -110.4683760289727132, -293.2662352645559167, -253.7030783399848985 ) ) ;
#55786 = CARTESIAN_POINT ( 'NONE',  ( -101.7209603822269912, -295.5738542108901470, -229.3974926409373438 ) ) ;
#55787 = CARTESIAN_POINT ( 'NONE',  ( 35.73587712130937177, -291.5269599033745180, -249.4895906788872253 ) ) ;
#55788 = CARTESIAN_POINT ( 'NONE',  ( -109.7555292035626309, -291.8060000616287084, -283.4612048821228427 ) ) ;
#55789 = ADVANCED_FACE ( 'NONE', ( #36597 ), #80289, .T. ) ;
#55790 = CARTESIAN_POINT ( 'NONE',  ( 222.8344101925596306, 0.000000000000000000, -7.000000000000000888 ) ) ;
#55791 = CARTESIAN_POINT ( 'NONE',  ( -110.4983976614188919, -291.3439824565651861, -271.1973789680909022 ) ) ;
#55792 = LINE ( 'NONE', #33527, #65671 ) ;
#55793 = CARTESIAN_POINT ( 'NONE',  ( -111.1552297526095003, -291.4992625893619334, -290.8445640704211996 ) ) ;
#55795 = CARTESIAN_POINT ( 'NONE',  ( 27.48653718474616525, -293.0957602275715885, -236.8007299199687168 ) ) ;
#55794 = CARTESIAN_POINT ( 'NONE',  ( -1.886548434290350240, -278.5395588520241290, -203.8679677830192531 ) ) ;
#55796 = CARTESIAN_POINT ( 'NONE',  ( -28.22500312982331039, -280.1646684249916461, -193.8491002969554984 ) ) ;
#55797 = CARTESIAN_POINT ( 'NONE',  ( -114.1875369891244247, -284.1519321946227024, -275.7120810180312560 ) ) ;
#55798 = CARTESIAN_POINT ( 'NONE',  ( 27.26633376575570367, -286.0588070545921369, -308.2236728744064180 ) ) ;
#55799 = CARTESIAN_POINT ( 'NONE',  ( -93.50896925536522986, -282.0114961195919250, -318.9201793785103405 ) ) ;
#55800 = CARTESIAN_POINT ( 'NONE',  ( -3.943430770372944760, -278.9645314803108249, -201.7372293118942821 ) ) ;
#55801 = CARTESIAN_POINT ( 'NONE',  ( -46.45507292069262206, -284.8593993161610456, -194.2136364376552820 ) ) ;
#55802 = CARTESIAN_POINT ( 'NONE',  ( 195.8576258688865721, 41.78303943026349998, 14.12515198783110826 ) ) ;
#55803 = CARTESIAN_POINT ( 'NONE',  ( 36.22349847479316765, -295.2290441538630716, -276.2434617587404091 ) ) ;
#55804 = CARTESIAN_POINT ( 'NONE',  ( 17.65280880277210329, -276.2447126287162860, -217.2360527939434292 ) ) ;
#55805 = CARTESIAN_POINT ( 'NONE',  ( -48.61529096533158167, -276.8662340104509667, -342.5581641288240462 ) ) ;
#55806 = CARTESIAN_POINT ( 'NONE',  ( -111.5414034733405231, -290.4610346717873313, -290.9379016961150342 ) ) ;
#55807 = CARTESIAN_POINT ( 'NONE',  ( -3.559017702572665254, -280.6897044565262718, -337.9628060080183900 ) ) ;
#55808 = CARTESIAN_POINT ( 'NONE',  ( 9.006989620723835799, -291.7648262048850825, -213.5925334579890773 ) ) ;
#55809 = CARTESIAN_POINT ( 'NONE',  ( -110.0365941876441696, -294.3143545456031234, -288.8644052524561516 ) ) ;
#55810 = ORIENTED_EDGE ( 'NONE', *, *, #40105, .T. ) ;
#55811 = CARTESIAN_POINT ( 'NONE',  ( 152.5497490326716274, 19.93678331745992693, 10.54177645506989514 ) ) ;
#55812 = CARTESIAN_POINT ( 'NONE',  ( -36.19888313780195688, -291.5744784292485292, -197.2960307922057268 ) ) ;
#55813 = CARTESIAN_POINT ( 'NONE',  ( 202.9738562182569694, 293.9636489450776367, -54.00000000000000000 ) ) ;
#55814 = CARTESIAN_POINT ( 'NONE',  ( 7.399455738971487229, -291.9094976428775681, -326.5171145203363494 ) ) ;
#55815 = CARTESIAN_POINT ( 'NONE',  ( -81.74539468072137538, -294.6989818203433060, -333.0449921331582459 ) ) ;
#55816 = CARTESIAN_POINT ( 'NONE',  ( 16.36453107020616926, -278.9441997284798731, -216.8464740409250453 ) ) ;
#55817 = CARTESIAN_POINT ( 'NONE',  ( -21.10505758099044371, -287.5714525714565184, -195.5970242595604986 ) ) ;
#55818 = CARTESIAN_POINT ( 'NONE',  ( 34.52131555760914239, -287.5547708797462292, -283.1949397468496841 ) ) ;
#55819 = CARTESIAN_POINT ( 'NONE',  ( -54.09289418273807115, -278.7911472558761830, -342.1779847956091771 ) ) ;
#55820 = CARTESIAN_POINT ( 'NONE',  ( -94.35464198576957529, -293.9024660101249538, -318.5615386243209741 ) ) ;
#55821 = CARTESIAN_POINT ( 'NONE',  ( -73.78206468869193202, -297.3032420467771431, -334.7821847612454462 ) ) ;
#55822 = CARTESIAN_POINT ( 'NONE',  ( -64.49423303950477759, -276.2094338642514799, -338.6050565531623420 ) ) ;
#55823 = ORIENTED_EDGE ( 'NONE', *, *, #34144, .F. ) ;
#55824 = CARTESIAN_POINT ( 'NONE',  ( 194.7276689066472954, 39.51856478053394994, 14.01265887717885050 ) ) ;
#55825 = CARTESIAN_POINT ( 'NONE',  ( -112.2861918467459645, -295.9982331894827894, -287.9984599004405368 ) ) ;
#55826 = CARTESIAN_POINT ( 'NONE',  ( -110.7000149349150462, -292.6396919553939142, -257.4222166310048578 ) ) ;
#55827 = CARTESIAN_POINT ( 'NONE',  ( 200.9738101188480641, 294.0933875133407582, -53.99999999999736389 ) ) ;
#55828 = CARTESIAN_POINT ( 'NONE',  ( 19.59809741626572688, -288.8508133312125779, -316.2059881883614025 ) ) ;
#55829 = CARTESIAN_POINT ( 'NONE',  ( -48.18343439339133027, -259.5409938267127359, -446.9856792133372778 ) ) ;
#55830 = EDGE_LOOP ( 'NONE', ( #60692, #18796, #55610, #73688 ) ) ;
#55831 = CARTESIAN_POINT ( 'NONE',  ( -38.15535180422752148, -279.1009419465214592, -193.6007233445317581 ) ) ;
#55832 = CARTESIAN_POINT ( 'NONE',  ( -96.42776434157040910, -296.5404914507276430, -319.5969309025309713 ) ) ;
#55833 = CARTESIAN_POINT ( 'NONE',  ( -107.2186457609142565, -289.0702917503227809, -241.0777106136807788 ) ) ;
#55834 = AXIS2_PLACEMENT_3D ( 'NONE', #33294, #77806, #39912 ) ;
#55835 = CARTESIAN_POINT ( 'NONE',  ( -36.90127381467026169, -298.3908043557193537, -193.3822376128566702 ) ) ;
#55836 = CARTESIAN_POINT ( 'NONE',  ( 34.85953520503804981, -294.0336780712257223, -281.6020136788554282 ) ) ;
#55837 = DIRECTION ( 'NONE',  ( -1.000000000000000000, 0.000000000000000000, 0.000000000000000000 ) ) ;
#55838 = CARTESIAN_POINT ( 'NONE',  ( 159.4851178187871312, 69.18068689461284748, -7.000000000000000888 ) ) ;
#55839 = CYLINDRICAL_SURFACE ( 'NONE', #47652, 4.000000000000003553 ) ;
#55840 = CARTESIAN_POINT ( 'NONE',  ( -17.88229110778965136, -290.3257672423472400, -344.1448502786595327 ) ) ;
#55841 = CARTESIAN_POINT ( 'NONE',  ( -115.3430155898818299, -281.2662352645559167, -252.5904736702033517 ) ) ;
#55842 = ORIENTED_EDGE ( 'NONE', *, *, #56649, .F. ) ;
#55843 = EDGE_CURVE ( 'NONE', #15987, #4883, #87838, .T. ) ;
#55844 = CARTESIAN_POINT ( 'NONE',  ( 25.84183455916705086, -281.4808017252806280, -314.2152407590183429 ) ) ;
#55845 = CARTESIAN_POINT ( 'NONE',  ( -84.83047191448920898, -287.3962458681714907, -212.4591364090152013 ) ) ;
#55846 = ADVANCED_FACE ( 'NONE', ( #65976 ), #51261, .F. ) ;
#55847 = CARTESIAN_POINT ( 'NONE',  ( 38.50338223247301528, -286.2491977846910913, -280.0664877549826883 ) ) ;
#55848 = CARTESIAN_POINT ( 'NONE',  ( -79.87671474844671593, -271.4756853532445007, -208.7287062667988948 ) ) ;
#55849 = CARTESIAN_POINT ( 'NONE',  ( -36.74868521505418073, -275.9798131421405856, -195.9108166195481147 ) ) ;
#55850 = CARTESIAN_POINT ( 'NONE',  ( -99.32295929599442275, -288.0705370889169217, -311.6109972932421783 ) ) ;
#55851 = CARTESIAN_POINT ( 'NONE',  ( -69.75079384670668503, -279.3346533238908478, -338.8585765529960554 ) ) ;
#55852 = ORIENTED_EDGE ( 'NONE', *, *, #15423, .F. ) ;
#55854 = CARTESIAN_POINT ( 'NONE',  ( -30.24424277496249047, -279.4927526733891341, -197.5541204920621681 ) ) ;
#55853 = CARTESIAN_POINT ( 'NONE',  ( -79.05486759071510505, -279.4718180145512747, -210.4527574622263728 ) ) ;
#55855 = CARTESIAN_POINT ( 'NONE',  ( 38.61611732443666511, -276.4989896970977270, -259.7827212467331606 ) ) ;
#55856 = CARTESIAN_POINT ( 'NONE',  ( -53.66084412209648491, -278.6423028466743972, -195.4623654345158741 ) ) ;
#55857 = CARTESIAN_POINT ( 'NONE',  ( -14.16128100611320306, -91.36119643908550358, -357.2170007693700882 ) ) ;
#55858 = CARTESIAN_POINT ( 'NONE',  ( -93.97978581159480882, -274.2004802261873238, -218.5252275717888040 ) ) ;
#55859 = CARTESIAN_POINT ( 'NONE',  ( -57.25379985901823687, -299.2255164674996877, -196.5355697911905963 ) ) ;
#55860 = CARTESIAN_POINT ( 'NONE',  ( 10.59707575819634329, -283.1948066931273047, -210.1954327657594490 ) ) ;
#55861 = EDGE_LOOP ( 'NONE', ( #24285, #50689, #49205, #59227 ) ) ;
#55862 = DIRECTION ( 'NONE',  ( 0.000000000000000000, 0.000000000000000000, -1.000000000000000000 ) ) ;
#55863 = CARTESIAN_POINT ( 'NONE',  ( 19.76288963607669302, -289.2790021743219313, -316.3316727168393641 ) ) ;
#55864 = CARTESIAN_POINT ( 'NONE',  ( 29.23279321469740921, -288.8302933671461687, -233.6212629989304901 ) ) ;
#55865 = CARTESIAN_POINT ( 'NONE',  ( -90.67279597412355940, -289.1816131803250869, -320.4319183225489951 ) ) ;
#55866 = CARTESIAN_POINT ( 'NONE',  ( -105.7323232406256324, -283.6038696310185969, -305.7229403694566940 ) ) ;
#55867 = CARTESIAN_POINT ( 'NONE',  ( -51.96617292990010384, -278.2618729916962366, -197.9723508188855590 ) ) ;
#55868 = CARTESIAN_POINT ( 'NONE',  ( 18.69325183354095898, -288.7299117239803650, -221.6687197992358165 ) ) ;
#55869 = CARTESIAN_POINT ( 'NONE',  ( 36.25740623410334962, -280.0807058659170252, -274.0866103614196732 ) ) ;
#55870 = CARTESIAN_POINT ( 'NONE',  ( -66.27919769689943053, -280.9803944930607713, -202.7910034938128376 ) ) ;
#55871 = CARTESIAN_POINT ( 'NONE',  ( -41.85412637857432117, -277.6028586809467242, -343.2957823925473804 ) ) ;
#55872 = CARTESIAN_POINT ( 'NONE',  ( -97.85542198797053004, -288.7165946713528797, -317.3302374858305939 ) ) ;
#55873 = CARTESIAN_POINT ( 'NONE',  ( -30.21966086357525683, -283.7670395628373967, -346.8688651529612912 ) ) ;
#55874 = CARTESIAN_POINT ( 'NONE',  ( -111.4305179371361731, -284.7843327317326612, -291.1065748104892350 ) ) ;
#55875 = CARTESIAN_POINT ( 'NONE',  ( -26.74067808226551080, -283.0803734113878249, -342.6385788490022151 ) ) ;
#55876 = ORIENTED_EDGE ( 'NONE', *, *, #30492, .F. ) ;
#55877 = DIRECTION ( 'NONE',  ( 1.000000000000000000, 0.000000000000000000, 0.000000000000000000 ) ) ;
#55878 = CARTESIAN_POINT ( 'NONE',  ( -108.3250529612868007, -292.7547362850664285, -243.7224436749581855 ) ) ;
#55879 = CARTESIAN_POINT ( 'NONE',  ( -42.00705088205833704, -290.6793331058134982, -193.9966447276455312 ) ) ;
#55880 = CARTESIAN_POINT ( 'NONE',  ( 20.87584843434727944, -273.9878481103862669, -225.9093399019967023 ) ) ;
#55881 = CARTESIAN_POINT ( 'NONE',  ( 17.48304448391924737, -293.6427124877519077, -324.3586428718817842 ) ) ;
#55882 = CARTESIAN_POINT ( 'NONE',  ( -95.50966863292985920, -288.4003599626506116, -315.6274541830374005 ) ) ;
#55883 = CARTESIAN_POINT ( 'NONE',  ( 31.52024291141157519, -292.1514989223406360, -297.6306795168488293 ) ) ;
#55884 = CARTESIAN_POINT ( 'NONE',  ( -110.0139457998354118, -291.6210493910559762, -280.7407214309300798 ) ) ;
#55885 = DIRECTION ( 'NONE',  ( -0.000000000000000000, 1.000000000000000000, -0.000000000000000000 ) ) ;
#55886 = CARTESIAN_POINT ( 'NONE',  ( -97.41158021147037971, -291.9386487216985984, -315.2890294410007073 ) ) ;
#55887 = CARTESIAN_POINT ( 'NONE',  ( 5.473371315473700705, -290.6302035960407011, -208.5800684491783841 ) ) ;
#55888 = CARTESIAN_POINT ( 'NONE',  ( -14.97970168342837205, -296.7627957996746204, -342.0032791716342899 ) ) ;
#55889 = CARTESIAN_POINT ( 'NONE',  ( 17.05738341949641068, -287.7933754856827591, -221.3102863981775954 ) ) ;
#55890 = CARTESIAN_POINT ( 'NONE',  ( -63.60126968552361149, -297.3938025512567265, -340.7916755050466122 ) ) ;
#55891 = CARTESIAN_POINT ( 'NONE',  ( 36.33185452959686756, -277.3289541461293197, -254.4694129795140327 ) ) ;
#55892 = CARTESIAN_POINT ( 'NONE',  ( -62.78192564562182554, -296.9263962180383487, -197.8562647251423527 ) ) ;
#55893 = CARTESIAN_POINT ( 'NONE',  ( -56.88908866994516700, -275.5474131657332464, -341.7997376742808342 ) ) ;
#55894 = CARTESIAN_POINT ( 'NONE',  ( -36.97720910188893839, -278.1365987337397883, -195.9220062992334590 ) ) ;
#55895 = CARTESIAN_POINT ( 'NONE',  ( -36.74819187013572730, -275.2648506555660788, -196.9539611793013307 ) ) ;
#55896 = CARTESIAN_POINT ( 'NONE',  ( -39.68980033698543508, -296.5074572549635263, -343.9254086251661420 ) ) ;
#55897 = CARTESIAN_POINT ( 'NONE',  ( 200.2296996224750103, 68.12454877784578855, 2.194831983258790586 ) ) ;
#55898 = CARTESIAN_POINT ( 'NONE',  ( -109.2062116672338732, -297.5363869913909411, -256.5796213035073379 ) ) ;
#55899 = CIRCLE ( 'NONE', #78549, 4.000000000000003553 ) ;
#55900 = CARTESIAN_POINT ( 'NONE',  ( 144.2857639756989272, -299.5541904835127980, -195.3611179825600175 ) ) ;
#55902 = CARTESIAN_POINT ( 'NONE',  ( -96.28011415179295795, -272.9896300714245854, -227.2043692953074014 ) ) ;
#55901 = CARTESIAN_POINT ( 'NONE',  ( 37.34841062809199030, -285.4445980340938149, -260.3714153990554792 ) ) ;
#55903 = CARTESIAN_POINT ( 'NONE',  ( 34.85422980127450643, -287.2136738447925381, -243.5889738466200924 ) ) ;
#55904 = AXIS2_PLACEMENT_3D ( 'NONE', #29110, #70354, #22016 ) ;
#55905 = CARTESIAN_POINT ( 'NONE',  ( -43.18492493439285340, -288.7907554321525367, -347.1178832569394217 ) ) ;
#55906 = CARTESIAN_POINT ( 'NONE',  ( -70.03866069211196077, -299.6034460271838498, -202.4691775345005453 ) ) ;
#55907 = CARTESIAN_POINT ( 'NONE',  ( -7.274496013806282413, -292.6567565528593491, -338.9023397666148867 ) ) ;
#55908 = CARTESIAN_POINT ( 'NONE',  ( 34.43302058299196489, -281.0973585484160822, -297.7937315470803128 ) ) ;
#55909 = CARTESIAN_POINT ( 'NONE',  ( -54.49178911615187815, -286.7666405000204577, -345.3538533559490702 ) ) ;
#55910 = CARTESIAN_POINT ( 'NONE',  ( -87.92197074771574705, -277.3452524989666585, -214.9147161604864493 ) ) ;
#55911 = CARTESIAN_POINT ( 'NONE',  ( -90.89292050906632880, -288.6280399794289337, -320.6289542331822986 ) ) ;
#55912 = DIRECTION ( 'NONE',  ( 0.000000000000000000, 0.000000000000000000, 1.000000000000000000 ) ) ;
#55913 = CARTESIAN_POINT ( 'NONE',  ( -105.8856430268801887, -288.1516246467788847, -300.9316883930976587 ) ) ;
#55914 = CARTESIAN_POINT ( 'NONE',  ( -95.16870256805567863, -274.7108019603028310, -224.6802079267853856 ) ) ;
#55915 = CARTESIAN_POINT ( 'NONE',  ( 32.62606933562828715, -282.5827397648077977, -239.6508993634868148 ) ) ;
#55917 = CARTESIAN_POINT ( 'NONE',  ( 21.00990313595386993, -282.1683262619324637, -314.2462292977136826 ) ) ;
#55916 = CARTESIAN_POINT ( 'NONE',  ( -72.49048407444017528, -295.6097756893146880, -203.6479357346821644 ) ) ;
#55918 = CARTESIAN_POINT ( 'NONE',  ( -108.3742201476035518, -296.3392501628699165, -300.2208348617602383 ) ) ;
#55919 = CARTESIAN_POINT ( 'NONE',  ( -92.47153030126679596, -274.6682450133892530, -221.6161003592695522 ) ) ;
#55920 = CARTESIAN_POINT ( 'NONE',  ( 38.14058268163777399, -285.5754942089768065, -265.9277254572482434 ) ) ;
#55921 = CARTESIAN_POINT ( 'NONE',  ( -17.54506600210016032, -282.3077298343403641, -198.0209913362684517 ) ) ;
#55922 = CARTESIAN_POINT ( 'NONE',  ( -108.2354701892585922, -271.7201905374424769, -251.5038136496105494 ) ) ;
#55923 = ORIENTED_EDGE ( 'NONE', *, *, #78922, .T. ) ;
#55924 = DIRECTION ( 'NONE',  ( -0.000000000000000000, 1.000000000000000000, -0.000000000000000000 ) ) ;
#55925 = CARTESIAN_POINT ( 'NONE',  ( -111.2441444686217409, -286.6675229615570970, -259.8599026558893001 ) ) ;
#55926 = FACE_OUTER_BOUND ( 'NONE', #21458, .T. ) ;
#55927 = CARTESIAN_POINT ( 'NONE',  ( 36.57525178469694538, -279.4809262143061233, -305.9938812882205070 ) ) ;
#55928 = CARTESIAN_POINT ( 'NONE',  ( 30.39587602696987290, -275.2204084354752354, -306.7471127574326033 ) ) ;
#55929 = CARTESIAN_POINT ( 'NONE',  ( -85.29845084291568469, -285.2492099288584200, -326.3151867489012261 ) ) ;
#55930 = CARTESIAN_POINT ( 'NONE',  ( -92.98987905329120451, -285.2569901151141494, -322.7433206337930187 ) ) ;
#55931 = CARTESIAN_POINT ( 'NONE',  ( -40.26545599562581401, -281.8846417625223353, -343.6999355166549321 ) ) ;
#55932 = CARTESIAN_POINT ( 'NONE',  ( 12.61967677588809167, -282.7489176715701547, -214.4248912238800813 ) ) ;
#55933 = CARTESIAN_POINT ( 'NONE',  ( -66.22918976118340595, -273.8509994291147791, -198.9710907124845392 ) ) ;
#55934 = CARTESIAN_POINT ( 'NONE',  ( 25.32813594469280005, -274.7926116731607635, -225.6005275951170574 ) ) ;
#55935 = CARTESIAN_POINT ( 'NONE',  ( -106.2865849365744708, -298.1035589174763913, -298.4309782289709005 ) ) ;
#55936 = CARTESIAN_POINT ( 'NONE',  ( 185.1905923765118587, 275.0000000000000568, 21.83530662808691503 ) ) ;
#55937 = CARTESIAN_POINT ( 'NONE',  ( 185.5586831021499563, 214.8268611780448509, 22.89084223187800049 ) ) ;
#55938 = CARTESIAN_POINT ( 'NONE',  ( -100.5066118230988934, -295.2513606600918479, -228.4985345894234570 ) ) ;
#55939 = CARTESIAN_POINT ( 'NONE',  ( 18.35125672540491948, -275.7316529746526612, -317.6504719508592416 ) ) ;
#55940 = CARTESIAN_POINT ( 'NONE',  ( -52.31554381620688332, -287.6179290135529527, -197.8783061155932330 ) ) ;
#55941 = CARTESIAN_POINT ( 'NONE',  ( 35.71161274853539425, -295.3535080424982766, -292.5838881597506997 ) ) ;
#55942 = CARTESIAN_POINT ( 'NONE',  ( 23.72179193499144745, -295.3765905230803241, -316.6132385493590391 ) ) ;
#55943 = EDGE_CURVE ( 'NONE', #42552, #54877, #19800, .T. ) ;
#55944 = CARTESIAN_POINT ( 'NONE',  ( -108.3180105222826342, -292.8595474917478327, -246.6463169331190102 ) ) ;
#55945 = CARTESIAN_POINT ( 'NONE',  ( -72.98095372644304746, -277.5785202583151090, -204.5593548495735661 ) ) ;
#55946 = CARTESIAN_POINT ( 'NONE',  ( -102.0758771461041476, -280.9659075920111491, -233.6078797385226551 ) ) ;
#55947 = CARTESIAN_POINT ( 'NONE',  ( -87.47752126717529109, -293.8381145249664428, -325.3857818550354182 ) ) ;
#55948 = CARTESIAN_POINT ( 'NONE',  ( 10.72751330863799701, -284.2566703096534297, -328.9922918666186433 ) ) ;
#55949 = CARTESIAN_POINT ( 'NONE',  ( -65.19799313359399662, -284.5998147868286878, -202.4966679312256019 ) ) ;
#55950 = CARTESIAN_POINT ( 'NONE',  ( -107.7075741586806004, -267.3548955105460436, -306.6422084984729395 ) ) ;
#55951 = VERTEX_POINT ( 'NONE', #14841 ) ;
#55952 = CARTESIAN_POINT ( 'NONE',  ( -107.7826725225565525, -283.9641996549107716, -289.6477982820007924 ) ) ;
#55953 = ORIENTED_EDGE ( 'NONE', *, *, #4532, .F. ) ;
#55954 = CARTESIAN_POINT ( 'NONE',  ( 37.02812134833334312, -282.3965876746442518, -251.6362103877525840 ) ) ;
#55955 = CARTESIAN_POINT ( 'NONE',  ( -110.2101890171688723, -272.9572434417630120, -264.9161015990332544 ) ) ;
#55956 = CARTESIAN_POINT ( 'NONE',  ( -87.47840982099886276, -284.1659497068868063, -212.3744229478787133 ) ) ;
#55957 = CARTESIAN_POINT ( 'NONE',  ( -90.90261130641086140, -280.2559220546347092, -215.2956475704461070 ) ) ;
#55958 = CARTESIAN_POINT ( 'NONE',  ( -39.91996080952217341, -278.6040766945079667, -346.6371661126491972 ) ) ;
#55959 = CARTESIAN_POINT ( 'NONE',  ( -62.02277691988539488, -280.3910522545137951, -197.4753124099462696 ) ) ;
#55960 = CARTESIAN_POINT ( 'NONE',  ( 7.450504543161054372, -272.1952119285918457, -214.2458315076590907 ) ) ;
#55961 = CARTESIAN_POINT ( 'NONE',  ( -106.8288633700993842, -263.1380580373908060, -317.6964085897507744 ) ) ;
#55962 = EDGE_LOOP ( 'NONE', ( #14434, #31859, #25101, #92750 ) ) ;
#55963 = CARTESIAN_POINT ( 'NONE',  ( 21.27606504587327407, -276.9115181615392771, -223.8219603609496460 ) ) ;
#55964 = CARTESIAN_POINT ( 'NONE',  ( -40.17672028908389592, -139.3485780022602114, -364.5271839380368988 ) ) ;
#55965 = AXIS2_PLACEMENT_3D ( 'NONE', #76227, #26971, #68191 ) ;
#55966 = CARTESIAN_POINT ( 'NONE',  ( -110.4942328733011010, -276.7646804713084521, -255.4459848794400898 ) ) ;
#55967 = CARTESIAN_POINT ( 'NONE',  ( 8.225115480596734585, -294.4256391158502311, -209.4872439545429756 ) ) ;
#55968 = CARTESIAN_POINT ( 'NONE',  ( -88.57920399699580116, -295.1424681792105389, -322.5725643634546600 ) ) ;
#55969 = CARTESIAN_POINT ( 'NONE',  ( -113.3002979947120679, -289.9066060351497072, -282.6011471253438572 ) ) ;
#55970 = DIRECTION ( 'NONE',  ( 0.000000000000000000, 0.000000000000000000, 1.000000000000000000 ) ) ;
#55972 = CARTESIAN_POINT ( 'NONE',  ( -9.169343535973261794, -284.8266026337799417, -202.1363265868821202 ) ) ;
#55971 = CARTESIAN_POINT ( 'NONE',  ( -112.0207258588586399, -295.3314643056204432, -254.1245355009379523 ) ) ;
#55973 = CARTESIAN_POINT ( 'NONE',  ( -100.7792367118623105, -292.9347134587859500, -231.8053864879299510 ) ) ;
#55974 = CARTESIAN_POINT ( 'NONE',  ( -110.7217342482675235, -285.9316996899287915, -265.4488170674724756 ) ) ;
#55975 = VERTEX_POINT ( 'NONE', #6813 ) ;
#55976 = CARTESIAN_POINT ( 'NONE',  ( -69.53545040790464782, -292.5799643079080283, -200.6590684102577882 ) ) ;
#55977 = CARTESIAN_POINT ( 'NONE',  ( -65.33347925078153651, -283.9205091120809357, -337.8613834636599904 ) ) ;
#55978 = CARTESIAN_POINT ( 'NONE',  ( -94.36630442429415666, -294.6493489821700109, -321.5294999101631106 ) ) ;
#55979 = CARTESIAN_POINT ( 'NONE',  ( -113.1990069752303185, -291.2015767068866694, -282.6015353977554128 ) ) ;
#55980 = CARTESIAN_POINT ( 'NONE',  ( -113.2983005987443050, -290.8911414489775780, -282.6135360386335833 ) ) ;
#55981 = CARTESIAN_POINT ( 'NONE',  ( 24.23948716713388762, -288.2608561698000358, -309.5626150944148094 ) ) ;
#55982 = ORIENTED_EDGE ( 'NONE', *, *, #34585, .T. ) ;
#55983 = CARTESIAN_POINT ( 'NONE',  ( -55.80257052418233599, -229.5268262511776527, 25.50000000000000000 ) ) ;
#55984 = CARTESIAN_POINT ( 'NONE',  ( -93.71639224285308956, -297.7143456237691339, -320.9986143411068724 ) ) ;
#55985 = CARTESIAN_POINT ( 'NONE',  ( -43.23495037039796074, -296.6641745611853480, -194.0287110980780767 ) ) ;
#55986 = CARTESIAN_POINT ( 'NONE',  ( -72.23128332299555154, -278.6372576719850827, -205.9707038432285344 ) ) ;
#55987 = CARTESIAN_POINT ( 'NONE',  ( 29.89680538609862026, -274.5734307707119228, -232.8548872660012421 ) ) ;
#55988 = CARTESIAN_POINT ( 'NONE',  ( -110.9350641024688997, -294.9818793123391742, -274.1983734775977268 ) ) ;
#55989 = CARTESIAN_POINT ( 'NONE',  ( 10.47749449157027790, -278.2439866612750734, -327.1430702514073801 ) ) ;
#55990 = CARTESIAN_POINT ( 'NONE',  ( 21.67773767129911633, -273.0688328519118500, -225.3116234614367386 ) ) ;
#55991 = CARTESIAN_POINT ( 'NONE',  ( -68.67297359981033367, -296.6784032147823496, -336.7487265291185281 ) ) ;
#55992 = CARTESIAN_POINT ( 'NONE',  ( -72.25975483507748720, -296.6052505806879367, -334.8343906807415920 ) ) ;
#55993 = LINE ( 'NONE', #90996, #8187 ) ;
#55994 = CARTESIAN_POINT ( 'NONE',  ( -95.88358803708518963, -297.4890531626940060, -319.1593432995440480 ) ) ;
#55995 = CARTESIAN_POINT ( 'NONE',  ( -111.4460249503558344, -270.7505508581946287, -256.4098452757740461 ) ) ;
#55996 = CARTESIAN_POINT ( 'NONE',  ( -49.71412802039538548, -292.5417297973257860, -198.2624042794496404 ) ) ;
#55997 = CARTESIAN_POINT ( 'NONE',  ( -78.76312769857507590, -274.3119664689808133, -205.6430821792482391 ) ) ;
#55998 = CARTESIAN_POINT ( 'NONE',  ( -110.0037841511857977, -288.9734550269866986, -282.0850863145746530 ) ) ;
#55999 = LINE ( 'NONE', #61255, #56375 ) ;
#56000 = CARTESIAN_POINT ( 'NONE',  ( -81.22044027451509862, -273.9659596949470597, -207.0970052568395658 ) ) ;
#56001 = CARTESIAN_POINT ( 'NONE',  ( -107.6220062574573575, -296.6235284075772256, -290.1794442787860362 ) ) ;
#56002 = CARTESIAN_POINT ( 'NONE',  ( -74.22535347838116593, -281.5442461561903542, -204.6496051451285325 ) ) ;
#56003 = CARTESIAN_POINT ( 'NONE',  ( 32.72804225596879490, -279.8427345702752973, -239.6441931085220176 ) ) ;
#56004 = CARTESIAN_POINT ( 'NONE',  ( -7.931305937635153569, -276.0254187580629264, -341.4270648641387993 ) ) ;
#56005 = CARTESIAN_POINT ( 'NONE',  ( 22.26243476972170754, -279.3095750331083877, -222.8662941098490933 ) ) ;
#56006 = CARTESIAN_POINT ( 'NONE',  ( 28.15169309927801677, -280.0435018229886737, -307.3540410067049606 ) ) ;
#56007 = CARTESIAN_POINT ( 'NONE',  ( -27.19108800622527866, -272.7582728492885735, -197.4240066745856268 ) ) ;
#56008 = CARTESIAN_POINT ( 'NONE',  ( -13.27255544842608082, -278.7398390813743276, -341.4481691860847263 ) ) ;
#56009 = CARTESIAN_POINT ( 'NONE',  ( 85.55100297371609486, -373.0521521680024648, -521.1711561948568487 ) ) ;
#56010 = CARTESIAN_POINT ( 'NONE',  ( 175.2296996224750103, 215.0000000000000568, 0.000000000000000000 ) ) ;
#56011 = CARTESIAN_POINT ( 'NONE',  ( -90.90513193883295173, -295.5443093140505084, -216.4636896091547271 ) ) ;
#56012 = CARTESIAN_POINT ( 'NONE',  ( -22.19378902478616311, -292.2408841875071630, -194.8114887592158198 ) ) ;
#56013 = CARTESIAN_POINT ( 'NONE',  ( 0.1551213403316603068, -278.5547186166668894, -335.5662848355707411 ) ) ;
#56014 = CARTESIAN_POINT ( 'NONE',  ( 23.10787926403396852, -272.9466195775318056, -225.9668728316694057 ) ) ;
#56015 = DIRECTION ( 'NONE',  ( 0.000000000000000000, 0.000000000000000000, 1.000000000000000000 ) ) ;
#56016 = CARTESIAN_POINT ( 'NONE',  ( 12.74489682270729141, -284.2804808577405993, -327.0050446814506131 ) ) ;
#56017 = CARTESIAN_POINT ( 'NONE',  ( 200.6103193995254230, 250.0000000000000568, -2.464576988612307229 ) ) ;
#56018 = ADVANCED_FACE ( 'NONE', ( #93427 ), #89317, .T. ) ;
#56019 = CARTESIAN_POINT ( 'NONE',  ( 37.66962986651619616, -285.5834618133250160, -272.8124283608974565 ) ) ;
#56020 =( BOUNDED_CURVE ( )  B_SPLINE_CURVE ( 3, ( #60591, #47268, #91297, #19348 ),
 .UNSPECIFIED., .F., .F. ) 
 B_SPLINE_CURVE_WITH_KNOTS ( ( 4, 4 ),
 ( 6.022196528194273313, 6.283185307179586232 ),
 .UNSPECIFIED. ) 
 CURVE ( )  GEOMETRIC_REPRESENTATION_ITEM ( )  RATIONAL_B_SPLINE_CURVE ( ( 1.000000000000000000, 0.9943317885200936290, 0.9943317885200936290, 1.000000000000000000 ) ) 
 REPRESENTATION_ITEM ( '' )  );
#56021 = CARTESIAN_POINT ( 'NONE',  ( 200.4738562182569694, 293.9636489450776367, -54.00000000000000000 ) ) ;
#56022 = CARTESIAN_POINT ( 'NONE',  ( -45.14814083827369728, -293.9479929199981711, -343.3926203374080046 ) ) ;
#56023 = CARTESIAN_POINT ( 'NONE',  ( -4.019223346084575432, -284.6360237272390350, -204.0250190281032019 ) ) ;
#56024 = DIRECTION ( 'NONE',  ( 0.000000000000000000, 0.000000000000000000, 1.000000000000000000 ) ) ;
#56025 = CARTESIAN_POINT ( 'NONE',  ( -5.950385865498482474, -292.6393662856775109, -338.4756248186760672 ) ) ;
#56026 = CARTESIAN_POINT ( 'NONE',  ( -65.60242375132042980, -284.1691266791250996, -199.4666351295204265 ) ) ;
#56027 = CARTESIAN_POINT ( 'NONE',  ( -68.88349678279791988, -281.2304653985445384, -203.6411398544783253 ) ) ;
#56028 = CARTESIAN_POINT ( 'NONE',  ( -2.417699391155528676, -287.7088322681562431, -202.1678324573639145 ) ) ;
#56029 = CARTESIAN_POINT ( 'NONE',  ( 38.51599593232745633, -279.8585754077139995, -275.6134851717976630 ) ) ;
#56030 = CARTESIAN_POINT ( 'NONE',  ( 35.65517884072506405, -287.5610568891780758, -271.0361445105027656 ) ) ;
#56031 =( BOUNDED_SURFACE ( )  B_SPLINE_SURFACE ( 3, 2, ( 
 ( #62784, #69382, #34345 ),
 ( #4514, #54235, #39530 ),
 ( #47110, #33391, #61822 ),
 ( #76017, #84049, #4989 ),
 ( #19195, #75551, #12087 ),
 ( #90206, #48054, #18257 ) ),
 .UNSPECIFIED., .F., .F., .F. ) 
 B_SPLINE_SURFACE_WITH_KNOTS ( ( 4, 2, 4 ),
 ( 3, 3 ),
 ( 0.006706248180543205976, 0.007337862909626279365, 0.007969477638709351885 ),
 ( 0.000000000000000000, 1.000000000000000000 ),
 .UNSPECIFIED. ) 
 GEOMETRIC_REPRESENTATION_ITEM ( )  RATIONAL_B_SPLINE_SURFACE ( (
 ( 1.000000000000000000, 0.7791885400064301193, 1.000000000000000000),
 ( 1.000000000000000000, 0.7898969217198510417, 1.000000000000000000),
 ( 1.000000000000000000, 0.7999169422268818108, 1.000000000000000000),
 ( 1.000000000000000000, 0.8184003267333962439, 1.000000000000000000),
 ( 1.000000000000000000, 0.8267394355353160362, 1.000000000000000000),
 ( 1.000000000000000000, 0.8333723006562909763, 1.000000000000000000) ) ) 
 REPRESENTATION_ITEM ( '' )  SURFACE ( )  );
#56032 = CARTESIAN_POINT ( 'NONE',  ( -24.79362128576465452, -281.6406575474871374, -197.8495972905729730 ) ) ;
#56033 = CARTESIAN_POINT ( 'NONE',  ( 18.08017707397654306, -281.6760748464290032, -222.5818940085184749 ) ) ;
#56034 = CARTESIAN_POINT ( 'NONE',  ( 0.6697430067040709423, -288.5361353586789050, -205.2804738438148604 ) ) ;
#56035 = AXIS2_PLACEMENT_3D ( 'NONE', #74794, #18894, #47749 ) ;
#56036 = VERTEX_POINT ( 'NONE', #44623 ) ;
#56037 = CARTESIAN_POINT ( 'NONE',  ( -36.89473150819597436, -297.8909244976909463, -193.3611301614376430 ) ) ;
#56039 = CARTESIAN_POINT ( 'NONE',  ( -104.3102276518549019, -292.0951064787559517, -303.3317582684422291 ) ) ;
#56038 = AXIS2_PLACEMENT_3D ( 'NONE', #16775, #52292, #1638 ) ;
#56040 = FACE_BOUND ( 'NONE', #70723, .T. ) ;
#56041 = CARTESIAN_POINT ( 'NONE',  ( -85.33152481854864391, -275.9090924074130839, -210.2361428286349110 ) ) ;
#56042 = ORIENTED_EDGE ( 'NONE', *, *, #32302, .F. ) ;
#56043 = CARTESIAN_POINT ( 'NONE',  ( 30.89960074401644263, -273.1375551215259065, -238.7227445224759208 ) ) ;
#56044 = CARTESIAN_POINT ( 'NONE',  ( -48.18343439339133027, -291.0521521680024080, -502.6442049081569508 ) ) ;
#56045 = CARTESIAN_POINT ( 'NONE',  ( -102.4428027032239470, -294.4295120102975716, -309.9627196893305268 ) ) ;
#56046 = CARTESIAN_POINT ( 'NONE',  ( 8.983965382278052303, -298.1551325937431329, -197.3035830641272526 ) ) ;
#56047 = CARTESIAN_POINT ( 'NONE',  ( -66.58653162377873969, -290.9622919390602078, -338.0576942310134427 ) ) ;
#56048 = CARTESIAN_POINT ( 'NONE',  ( 34.74228035353977617, -283.0938460413431130, -253.5720210866410014 ) ) ;
#56049 = CARTESIAN_POINT ( 'NONE',  ( -15.10623445322716663, -290.1951008165304984, -343.5204162540024413 ) ) ;
#56050 = CARTESIAN_POINT ( 'NONE',  ( -87.05122025990725376, -291.0424129964769122, -328.5879059861280780 ) ) ;
#56051 = CARTESIAN_POINT ( 'NONE',  ( -65.87713355294340545, -287.6791493860777678, -200.9464024555221044 ) ) ;
#56052 = CARTESIAN_POINT ( 'NONE',  ( -38.17203572532561395, -280.2086946658774878, -193.3655950781079866 ) ) ;
#56053 = CARTESIAN_POINT ( 'NONE',  ( 36.65532809355934063, -291.8268569546354456, -285.6501341635693052 ) ) ;
#56054 = CARTESIAN_POINT ( 'NONE',  ( 32.02238942766086183, -280.9552158191860372, -236.8075744291823241 ) ) ;
#56055 = CARTESIAN_POINT ( 'NONE',  ( 33.22876386161097173, -277.1100321137354285, -247.1595325974809612 ) ) ;
#56056 = EDGE_CURVE ( 'NONE', #23662, #17402, #12228, .T. ) ;
#56057 = CARTESIAN_POINT ( 'NONE',  ( 27.33386217378599881, -283.6233781216987495, -239.1787733560258573 ) ) ;
#56058 = CARTESIAN_POINT ( 'NONE',  ( 37.92359159668361457, -273.6596351941662988, -259.9155507374346143 ) ) ;
#56059 = DIRECTION ( 'NONE',  ( -1.000000000000000000, 0.000000000000000000, 0.000000000000000000 ) ) ;
#56060 = CARTESIAN_POINT ( 'NONE',  ( 35.76431847340407444, -281.0724510958451674, -271.3208181675600486 ) ) ;
#56061 = CARTESIAN_POINT ( 'NONE',  ( -38.52336472219708696, -278.2717301988474219, -346.9549322820475936 ) ) ;
#56062 = CARTESIAN_POINT ( 'NONE',  ( -102.4752169656997580, -274.3287924989739963, -236.2086887407280358 ) ) ;
#56063 = CARTESIAN_POINT ( 'NONE',  ( -112.1277792125293615, -283.8281385059705144, -253.0445770638732768 ) ) ;
#56064 = CARTESIAN_POINT ( 'NONE',  ( -63.17513472305719091, -293.4711289431203909, -201.0025736617258474 ) ) ;
#56065 = CARTESIAN_POINT ( 'NONE',  ( -71.06725443763581040, -275.2145963204682744, -202.0308362257548538 ) ) ;
#56066 = CARTESIAN_POINT ( 'NONE',  ( -68.65762688818671222, -274.9642966368102179, -200.5427231659969323 ) ) ;
#56067 = DIRECTION ( 'NONE',  ( -0.7453559924999217934, 0.000000000000000000, -0.6666666666666758445 ) ) ;
#56068 = CARTESIAN_POINT ( 'NONE',  ( 18.30703445672270036, -276.0572674661329984, -317.6074759759202948 ) ) ;
#56069 = CARTESIAN_POINT ( 'NONE',  ( -50.77594290759483187, -297.2243425807369022, -343.9787078956802588 ) ) ;
#56070 = CARTESIAN_POINT ( 'NONE',  ( -57.87353748088431615, -283.7863288919468232, -198.3455879892530334 ) ) ;
#56071 = CARTESIAN_POINT ( 'NONE',  ( 4.133717683148574018, -292.2610753755764108, -205.4478441155281132 ) ) ;
#56072 = CARTESIAN_POINT ( 'NONE',  ( 1.710938404082930742, -274.5476746908430528, -334.0358190628547845 ) ) ;
#56073 = CARTESIAN_POINT ( 'NONE',  ( 14.07904642907681314, -289.9450211195631937, -326.6673892184522288 ) ) ;
#56074 = CARTESIAN_POINT ( 'NONE',  ( -104.3357715634736422, -289.0719655914077180, -300.2526313965403801 ) ) ;
#56075 = ORIENTED_EDGE ( 'NONE', *, *, #19615, .T. ) ;
#56076 = CARTESIAN_POINT ( 'NONE',  ( -30.73002346790145722, -290.7087765773584351, -194.1845752282874855 ) ) ;
#56077 = CARTESIAN_POINT ( 'NONE',  ( -105.7289510306664653, -290.5619881419297599, -244.6193941095278319 ) ) ;
#56078 = ORIENTED_EDGE ( 'NONE', *, *, #13000, .F. ) ;
#56079 = CARTESIAN_POINT ( 'NONE',  ( 39.29615340389884182, -288.6824484063742489, -274.3929202436269179 ) ) ;
#56080 = CARTESIAN_POINT ( 'NONE',  ( -87.54824253368641962, -279.6614668651365037, -217.2686879053882194 ) ) ;
#56081 = ADVANCED_FACE ( 'NONE', ( #43694 ), #29968, .T. ) ;
#56082 = CARTESIAN_POINT ( 'NONE',  ( -33.46427230025540211, -293.9247800029913833, -346.9669916583351892 ) ) ;
#56083 = CARTESIAN_POINT ( 'NONE',  ( -76.06257783564061015, -286.2008183768584786, -203.8618062814195753 ) ) ;
#56084 = CARTESIAN_POINT ( 'NONE',  ( -78.51473750191632917, -285.8471941912260377, -205.3186296776731012 ) ) ;
#56085 = CARTESIAN_POINT ( 'NONE',  ( 28.17191445445139664, -282.3236899235331521, -302.7257461959653710 ) ) ;
#56086 = CARTESIAN_POINT ( 'NONE',  ( 180.2115114871389210, 254.1752151913870250, -166.7759868809612840 ) ) ;
#56087 = CARTESIAN_POINT ( 'NONE',  ( 188.1608565823388801, 271.2200784998753420, -139.0206290322748544 ) ) ;
#56088 = CARTESIAN_POINT ( 'NONE',  ( -94.43123972790466780, -238.4150439815195739, -338.5472242393929605 ) ) ;
#56089 = CARTESIAN_POINT ( 'NONE',  ( 34.86484249539895330, -274.9084239664247775, -282.4490291555209751 ) ) ;
#56090 = CARTESIAN_POINT ( 'NONE',  ( 19.24619231726884649, -273.8147980199998415, -223.7560055679572883 ) ) ;
#56091 = CARTESIAN_POINT ( 'NONE',  ( -110.7429703914275052, -295.7693060960082221, -293.4655916616991362 ) ) ;
#56092 = CARTESIAN_POINT ( 'NONE',  ( -110.4136360351100308, -271.8502356476486170, -283.7365558647884427 ) ) ;
#56093 = CARTESIAN_POINT ( 'NONE',  ( 26.52814733732099128, -273.6795811212947456, -228.2429407039788316 ) ) ;
#56094 = CARTESIAN_POINT ( 'NONE',  ( -101.6086385096167959, -274.8096281454858740, -233.5464982536482239 ) ) ;
#56095 = CARTESIAN_POINT ( 'NONE',  ( -38.91795226453715628, -293.1115901840395281, -197.0689526187062484 ) ) ;
#56096 = ORIENTED_EDGE ( 'NONE', *, *, #49490, .T. ) ;
#56097 = CARTESIAN_POINT ( 'NONE',  ( -111.3619466279452297, -297.2377964174202134, -290.7037658316841657 ) ) ;
#56098 = CARTESIAN_POINT ( 'NONE',  ( 21.22657140224840688, -288.6570643363683644, -314.0598147405129339 ) ) ;
#56099 = CARTESIAN_POINT ( 'NONE',  ( -88.49030546875899006, -296.5503979021305554, -327.7733609191539585 ) ) ;
#56100 = CARTESIAN_POINT ( 'NONE',  ( -65.57507530830704923, -295.9039270333842637, -341.9462958329617095 ) ) ;
#56101 = CARTESIAN_POINT ( 'NONE',  ( 34.06801983643734388, -293.9195337676179065, -285.5753549825724349 ) ) ;
#56102 = ORIENTED_EDGE ( 'NONE', *, *, #19615, .F. ) ;
#56103 = CARTESIAN_POINT ( 'NONE',  ( 21.61905308987663332, -276.8270026609069419, -223.0865746737032964 ) ) ;
#56104 = EDGE_LOOP ( 'NONE', ( #36284, #79027, #60629, #43491 ) ) ;
#56105 = CARTESIAN_POINT ( 'NONE',  ( -56.53523653229239443, -279.3189735065992636, -195.8002231839548983 ) ) ;
#56106 = PRODUCT_DEFINITION_CONTEXT ( 'detailed design', #84968, 'design' ) ;
#56107 = CARTESIAN_POINT ( 'NONE',  ( -1.344153737431386553, -277.5038249682741025, -334.1961303392545801 ) ) ;
#56108 = CARTESIAN_POINT ( 'NONE',  ( 37.91741627755514799, -277.1793497440049237, -259.8711508077181520 ) ) ;
#56109 = AXIS2_PLACEMENT_3D ( 'NONE', #35204, #64133, #92967 ) ;
#56110 = CARTESIAN_POINT ( 'NONE',  ( -70.86233746374362852, -275.5122971263422187, -337.8501813903125139 ) ) ;
#56111 = CARTESIAN_POINT ( 'NONE',  ( -49.97968222912750491, -298.5380334163676253, -198.3599091295398011 ) ) ;
#56112 = CARTESIAN_POINT ( 'NONE',  ( -96.08557286186945134, -294.5090240609454781, -314.7049276706690080 ) ) ;
#56113 = LINE ( 'NONE', #48042, #3352 ) ;
#56114 = CARTESIAN_POINT ( 'NONE',  ( -97.00269320569096010, -278.3918511870139127, -318.9625334014482405 ) ) ;
#56115 = CARTESIAN_POINT ( 'NONE',  ( -66.80071543032686066, -277.6159260062093495, -337.1530817353018392 ) ) ;
#56116 = AXIS2_PLACEMENT_3D ( 'NONE', #63195, #5880, #92025 ) ;
#56117 = CARTESIAN_POINT ( 'NONE',  ( -10.15344535591867547, -285.0844489322089430, -198.7917601921903952 ) ) ;
#56118 = CARTESIAN_POINT ( 'NONE',  ( -51.48132906306179990, -299.8720352385096248, -196.4832810645096686 ) ) ;
#56119 = DIRECTION ( 'NONE',  ( -0.000000000000000000, -0.000000000000000000, -1.000000000000000000 ) ) ;
#56120 = CARTESIAN_POINT ( 'NONE',  ( 28.36831870069437400, -287.1840995813325890, -302.5293500126085178 ) ) ;
#56121 = CARTESIAN_POINT ( 'NONE',  ( -34.24885224764852154, -278.3313906953229093, -196.3997135302541892 ) ) ;
#56123 = CARTESIAN_POINT ( 'NONE',  ( -108.3669899675573589, -282.3423169509645163, -292.6483879220964468 ) ) ;
#56122 = CARTESIAN_POINT ( 'NONE',  ( -83.79575546704707278, -277.9749421671019718, -213.2215784465003594 ) ) ;
#56124 = CARTESIAN_POINT ( 'NONE',  ( -30.52643038339077819, -288.1383674637465901, -195.6200632462643512 ) ) ;
#56125 = CARTESIAN_POINT ( 'NONE',  ( 19.49879119586512388, -277.4113360036536733, -316.8167879374884137 ) ) ;
#56126 = FACE_OUTER_BOUND ( 'NONE', #23482, .T. ) ;
#56127 = CARTESIAN_POINT ( 'NONE',  ( -2.995052495117620506, -294.5060914721845506, -203.6735798760489615 ) ) ;
#56128 = CARTESIAN_POINT ( 'NONE',  ( -42.75662538109197186, -275.3594626212182561, -346.1546045006214740 ) ) ;
#56129 = CARTESIAN_POINT ( 'NONE',  ( -66.83619260384088534, -278.1005808026465616, -337.2488416847240273 ) ) ;
#56130 = CARTESIAN_POINT ( 'NONE',  ( 12.48502450904744876, -284.3604744035619660, -326.7094229152319258 ) ) ;
#56131 = DIRECTION ( 'NONE',  ( 0.000000000000000000, 0.000000000000000000, 1.000000000000000000 ) ) ;
#56132 = CARTESIAN_POINT ( 'NONE',  ( 34.58464376219601633, -289.7689638375961181, -293.5109614464082028 ) ) ;
#56133 = CARTESIAN_POINT ( 'NONE',  ( -58.69855347909871313, -293.3280512289803710, -342.3093950506277565 ) ) ;
#56134 = LINE ( 'NONE', #20142, #17911 ) ;
#56135 = CARTESIAN_POINT ( 'NONE',  ( -34.00162091959891342, -272.7798640336235394, -196.9439037219777333 ) ) ;
#56136 = CARTESIAN_POINT ( 'NONE',  ( -14.44326268775513533, -290.4917740870004650, -199.7457723312913060 ) ) ;
#56137 = DIRECTION ( 'NONE',  ( 0.000000000000000000, 0.000000000000000000, 1.000000000000000000 ) ) ;
#56138 = DIRECTION ( 'NONE',  ( 0.000000000000000000, 0.000000000000000000, -1.000000000000000000 ) ) ;
#56139 = CARTESIAN_POINT ( 'NONE',  ( -112.4858525041450719, -289.1994887688476865, -257.0922025289438579 ) ) ;
#56140 = CARTESIAN_POINT ( 'NONE',  ( -94.02356840303724539, -285.4888981486163289, -317.6221614120665890 ) ) ;
#56141 = CARTESIAN_POINT ( 'NONE',  ( 38.08186445193869929, -285.9143828498046673, -280.0169502407761684 ) ) ;
#56142 = EDGE_CURVE ( 'NONE', #77260, #54214, #28579, .T. ) ;
#56143 = CARTESIAN_POINT ( 'NONE',  ( -49.53690538590971215, -287.3190342997609719, -197.7375001204646878 ) ) ;
#56144 = CARTESIAN_POINT ( 'NONE',  ( -46.75575602308124701, -286.7325507428079732, -197.7569578035559630 ) ) ;
#56145 = CARTESIAN_POINT ( 'NONE',  ( -112.3717159241940493, -292.6283266365251734, -262.8270252350141618 ) ) ;
#56146 = CARTESIAN_POINT ( 'NONE',  ( 2.716951582430970902, -274.5995686634144590, -334.4899941275415927 ) ) ;
#56147 = CARTESIAN_POINT ( 'NONE',  ( 35.18248142849234483, -276.2129943351353631, -296.3249920667107631 ) ) ;
#56148 = CARTESIAN_POINT ( 'NONE',  ( -107.0294434081068431, -289.0105632392450730, -241.1561075897265027 ) ) ;
#56149 = CARTESIAN_POINT ( 'NONE',  ( -37.12696551596004468, -277.0494984396683549, -347.3738772233279519 ) ) ;
#56150 = CARTESIAN_POINT ( 'NONE',  ( -109.8918220812226281, -298.3048153400479237, -287.9741771711922524 ) ) ;
#56151 = CARTESIAN_POINT ( 'NONE',  ( -48.18343439339133027, -253.2160367274611872, -476.5905725146912459 ) ) ;
#56152 = CARTESIAN_POINT ( 'NONE',  ( 186.6539576904058890, 293.9636489450775230, 0.000000000000000000 ) ) ;
#56153 = CARTESIAN_POINT ( 'NONE',  ( -110.7194928009815129, -283.3017751159325712, -265.4154428059761130 ) ) ;
#56154 = CARTESIAN_POINT ( 'NONE',  ( -14.80384949957305984, -278.3438646973627897, -198.7731334203974711 ) ) ;
#56155 = DIRECTION ( 'NONE',  ( -1.000000000000000000, 0.000000000000000000, 0.000000000000000000 ) ) ;
#56156 = CARTESIAN_POINT ( 'NONE',  ( 38.24011964427000265, -273.8996157313088702, -259.8684408988631844 ) ) ;
#56157 = CARTESIAN_POINT ( 'NONE',  ( -27.01530201320642988, -276.2659646161451974, -342.7300213178120885 ) ) ;
#56158 = CARTESIAN_POINT ( 'NONE',  ( -6.456866650744444769, -296.1590791022027247, -337.2702714331201719 ) ) ;
#56159 = CARTESIAN_POINT ( 'NONE',  ( -35.33030082650350323, -278.9971463005194323, -193.6835260780933083 ) ) ;
#56160 = CARTESIAN_POINT ( 'NONE',  ( -53.18864949045561019, -296.2014857338569982, -341.9134967324556555 ) ) ;
#56161 = CARTESIAN_POINT ( 'NONE',  ( -24.97094080966079588, -296.2128485230616661, -345.9149225143329431 ) ) ;
#56162 = CARTESIAN_POINT ( 'NONE',  ( -91.84347862019282616, -297.0799420491071601, -221.7961496853052950 ) ) ;
#56163 = CARTESIAN_POINT ( 'NONE',  ( -41.73477394707572330, -293.9970988171320414, -195.4386734662660388 ) ) ;
#56164 = CARTESIAN_POINT ( 'NONE',  ( -80.93995271441103512, -285.6450764003434415, -206.8287161890721109 ) ) ;
#56165 = CARTESIAN_POINT ( 'NONE',  ( 25.13956825401882966, -273.1167383573363168, -227.4849147633873940 ) ) ;
#56166 = CARTESIAN_POINT ( 'NONE',  ( -4.334988585874142153, -288.4623828018427503, -339.9425218279787373 ) ) ;
#56167 = CARTESIAN_POINT ( 'NONE',  ( -77.73260448470320227, -281.4872097975710972, -207.5267108538691616 ) ) ;
#56168 = ADVANCED_FACE ( 'NONE', ( #29517 ), #58397, .F. ) ;
#56169 = CARTESIAN_POINT ( 'NONE',  ( -93.42759532358584806, -284.2775400376325479, -223.2677977673970133 ) ) ;
#56170 = CARTESIAN_POINT ( 'NONE',  ( -103.4065977414673654, -288.0807596467917620, -305.8636523889234127 ) ) ;
#56171 = CARTESIAN_POINT ( 'NONE',  ( 30.52007695399996479, -26.23604800832216100, -343.5755449821854768 ) ) ;
#56172 = CARTESIAN_POINT ( 'NONE',  ( -54.76494257819371825, -285.3298827151859314, -199.3551368336666201 ) ) ;
#56173 = CARTESIAN_POINT ( 'NONE',  ( 198.3053063117764907, 298.1794517842361643, -6.802035004563411924 ) ) ;
#56174 = CARTESIAN_POINT ( 'NONE',  ( 6.799537257745960517, -283.4093464495015269, -333.2303568041374433 ) ) ;
#56175 = CARTESIAN_POINT ( 'NONE',  ( -96.39017246408651829, -290.2727280257241773, -221.2888144382199300 ) ) ;
#56176 = CARTESIAN_POINT ( 'NONE',  ( -98.79489647237402039, -280.7571348047457604, -225.2841770571867812 ) ) ;
#56177 = CARTESIAN_POINT ( 'NONE',  ( -77.24966325893828412, -280.8444757689106837, -205.0261045969996587 ) ) ;
#56178 = CARTESIAN_POINT ( 'NONE',  ( 31.35387658402771649, -281.7161544125552837, -295.2070776969027861 ) ) ;
#56179 = CARTESIAN_POINT ( 'NONE',  ( 36.99967650147244314, -277.4249723052648164, -260.4434383497034560 ) ) ;
#56180 = CARTESIAN_POINT ( 'NONE',  ( -90.71207447207180508, -295.7834944769748518, -325.9377074866476960 ) ) ;
#56181 = CARTESIAN_POINT ( 'NONE',  ( -104.3324312289769296, -288.1359593528396772, -303.2866209571684522 ) ) ;
#56182 = CARTESIAN_POINT ( 'NONE',  ( -104.2242475918841222, -295.0683892303916309, -300.5011037832608167 ) ) ;
#56183 = ORIENTED_EDGE ( 'NONE', *, *, #27622, .T. ) ;
#56184 = ORIENTED_EDGE ( 'NONE', *, *, #27047, .T. ) ;
#56185 = CARTESIAN_POINT ( 'NONE',  ( 29.45379109670336604, -283.9103074744073751, -303.3366064260893609 ) ) ;
#56186 = CARTESIAN_POINT ( 'NONE',  ( -110.2331408390485450, -296.2762403300752112, -266.0107895148270245 ) ) ;
#56187 = CARTESIAN_POINT ( 'NONE',  ( 27.78256927198205162, -294.0987262493824801, -229.7599130250441988 ) ) ;
#56188 = CARTESIAN_POINT ( 'NONE',  ( -93.49505205585893464, -284.5403364527106191, -317.1659653360856055 ) ) ;
#56189 = ADVANCED_FACE ( 'NONE', ( #21464 ), #157, .T. ) ;
#56190 = CARTESIAN_POINT ( 'NONE',  ( 17.92853962991826933, -273.8785699404692764, -217.0117216562484259 ) ) ;
#56191 = CARTESIAN_POINT ( 'NONE',  ( -42.05601121605359793, -292.6456027885760705, -193.6076942305612079 ) ) ;
#56192 = CARTESIAN_POINT ( 'NONE',  ( -66.68839300440839679, -283.8113595802154805, -200.5107271523263819 ) ) ;
#56193 = CARTESIAN_POINT ( 'NONE',  ( -111.5204605413089070, -290.6276088922380723, -290.9342994363199750 ) ) ;
#56194 = CARTESIAN_POINT ( 'NONE',  ( 32.29247638116856933, -287.5936364837710357, -248.3381605330316972 ) ) ;
#56195 = DIRECTION ( 'NONE',  ( 0.000000000000000000, 0.000000000000000000, -1.000000000000000000 ) ) ;
#56196 = CYLINDRICAL_SURFACE ( 'NONE', #78031, 2.000000000000000000 ) ;
#56197 = CARTESIAN_POINT ( 'NONE',  ( 160.6708272468242740, 217.8012694009499626, -202.3251110406953899 ) ) ;
#56198 = CARTESIAN_POINT ( 'NONE',  ( -13.61894215047240664, -284.2697782174893177, -342.8865514901725078 ) ) ;
#56199 = CARTESIAN_POINT ( 'NONE',  ( -54.42813229853333468, -283.3380690714491266, -195.3538533559490702 ) ) ;
#56200 = ORIENTED_EDGE ( 'NONE', *, *, #8700, .F. ) ;
#56201 = CARTESIAN_POINT ( 'NONE',  ( 3.551296040237138740, -281.4084660206444255, -331.2664868571021657 ) ) ;
#56202 = CARTESIAN_POINT ( 'NONE',  ( -7.896651663262564291, -276.3434994152810873, -341.5001718711064314 ) ) ;
#56203 = CARTESIAN_POINT ( 'NONE',  ( -84.13375484440895491, -279.6968515543772469, -328.8275528808673016 ) ) ;
#56204 = CARTESIAN_POINT ( 'NONE',  ( -92.65688847005533546, -240.4251198286245028, -339.9941278092445600 ) ) ;
#56205 = CARTESIAN_POINT ( 'NONE',  ( 38.21490009151112588, -279.9789647599371278, -258.6241527485910865 ) ) ;
#56206 = CARTESIAN_POINT ( 'NONE',  ( -88.81079852685080311, -283.3451212658792429, -216.2983885761691454 ) ) ;
#56207 = CARTESIAN_POINT ( 'NONE',  ( -82.38812378547730475, -299.2071559892513051, -209.1010080315972459 ) ) ;
#56208 = CARTESIAN_POINT ( 'NONE',  ( 34.38598553318960427, -294.2276716163444235, -284.2581518925622390 ) ) ;
#56209 = ORIENTED_EDGE ( 'NONE', *, *, #49759, .F. ) ;
#56210 = CARTESIAN_POINT ( 'NONE',  ( -110.4618674326619328, -289.3338684781452912, -262.9662136043678515 ) ) ;
#56211 = CARTESIAN_POINT ( 'NONE',  ( 39.52874431672737643, -276.1777548212208444, -268.3001577368727908 ) ) ;
#56212 = CARTESIAN_POINT ( 'NONE',  ( -71.90772880776439990, -273.5820958407003900, -206.0071293961021297 ) ) ;
#56213 = ORIENTED_EDGE ( 'NONE', *, *, #60067, .T. ) ;
#56214 = CARTESIAN_POINT ( 'NONE',  ( -46.82907625988709555, -272.8546930203463035, -194.2593295450973017 ) ) ;
#56215 = CARTESIAN_POINT ( 'NONE',  ( 222.8344101925596306, 0.000000000000000000, -21.50000000000000000 ) ) ;
#56216 = CARTESIAN_POINT ( 'NONE',  ( 155.0601170292805193, 20.95974790765944107, -14.78042489204667120 ) ) ;
#56217 = EDGE_CURVE ( 'NONE', #39182, #49216, #47008, .T. ) ;
#56218 = DIRECTION ( 'NONE',  ( 0.000000000000000000, 1.000000000000000000, 0.000000000000000000 ) ) ;
#56219 = CARTESIAN_POINT ( 'NONE',  ( -36.17487965774702730, -284.1168558368651702, -343.6609447530025250 ) ) ;
#56220 = CARTESIAN_POINT ( 'NONE',  ( -94.21838698159886860, -281.0040325333411033, -219.9724634315274159 ) ) ;
#56221 = CARTESIAN_POINT ( 'NONE',  ( -105.4371278660812123, -283.2498839915487565, -297.4514208470191079 ) ) ;
#56222 = CARTESIAN_POINT ( 'NONE',  ( -38.39478520791233507, -281.8992335247962728, -196.1207729376543512 ) ) ;
#56223 = CARTESIAN_POINT ( 'NONE',  ( 21.37776051075837458, -274.6519185729246146, -314.8890047105255690 ) ) ;
#56224 = CARTESIAN_POINT ( 'NONE',  ( 208.2166030336615563, 27.61833517603036725, 14.22786471510347184 ) ) ;
#56225 = LINE ( 'NONE', #49574, #45584 ) ;
#56226 = CARTESIAN_POINT ( 'NONE',  ( -71.48988190798968390, -278.2945715345014719, -339.1946890244837505 ) ) ;
#56227 = EDGE_LOOP ( 'NONE', ( #32429, #43280, #13207, #77734 ) ) ;
#56228 = ORIENTED_EDGE ( 'NONE', *, *, #82755, .T. ) ;
#56229 = DIRECTION ( 'NONE',  ( -0.000000000000000000, -0.000000000000000000, -1.000000000000000000 ) ) ;
#56230 = CARTESIAN_POINT ( 'NONE',  ( -112.5646487503656630, -286.4647331273862960, -275.6284759522291097 ) ) ;
#56231 = CARTESIAN_POINT ( 'NONE',  ( -4.751984350100819654, -291.6898812667785137, -204.8451606152623583 ) ) ;
#56232 = CARTESIAN_POINT ( 'NONE',  ( -8.279354188717762852, -288.0300666213736349, -341.5701174569828140 ) ) ;
#56233 = CARTESIAN_POINT ( 'NONE',  ( -101.8638743311186516, -283.2826316567292793, -233.9951015377691306 ) ) ;
#56235 = CARTESIAN_POINT ( 'NONE',  ( -96.59283317398147517, -288.1777366249448278, -314.7362757162314892 ) ) ;
#56234 = CARTESIAN_POINT ( 'NONE',  ( -110.9801791004865237, -283.1198777690026418, -270.8956101083488193 ) ) ;
#56236 = CARTESIAN_POINT ( 'NONE',  ( 1.323459663542760900, -283.7285887856345994, -332.8074569326296910 ) ) ;
#56237 = CARTESIAN_POINT ( 'NONE',  ( 4.727820773182989988, -274.4838739887581482, -332.4510210081800778 ) ) ;
#56238 = VECTOR ( 'NONE', #66130, 1000.000000000000000 ) ;
#56239 = CARTESIAN_POINT ( 'NONE',  ( 31.99266720023009114, -285.5422704550279036, -238.6241207358383463 ) ) ;
#56240 = CARTESIAN_POINT ( 'NONE',  ( -26.59438322183623526, -300.1868440504003388, -195.3574452081263928 ) ) ;
#56241 = CARTESIAN_POINT ( 'NONE',  ( -99.46653649144340648, -283.1247177515152771, -227.9545250757125814 ) ) ;
#56242 = CIRCLE ( 'NONE', #45654, 1.000000000000000888 ) ;
#56243 = CARTESIAN_POINT ( 'NONE',  ( -41.07512915030789458, -280.9452678741344585, -197.2210471851076932 ) ) ;
#56244 = CARTESIAN_POINT ( 'NONE',  ( 29.77313388996562438, -289.1061269904064943, -236.5139987813681444 ) ) ;
#56245 = CARTESIAN_POINT ( 'NONE',  ( 196.9534188175200029, 25.84350552936208700, 12.42857142857141817 ) ) ;
#56246 = CARTESIAN_POINT ( 'NONE',  ( 207.3481610410795213, 36.16742558173439193, 14.95883904121434682 ) ) ;
#56247 = CARTESIAN_POINT ( 'NONE',  ( -33.48344422893534045, -296.9241208876456994, -345.8354260878668356 ) ) ;
#56248 = AXIS2_PLACEMENT_3D ( 'NONE', #59043, #88373, #80342 ) ;
#56249 = CARTESIAN_POINT ( 'NONE',  ( -105.1679627103966084, -276.9744033437324902, -238.2297838379603263 ) ) ;
#56250 = CARTESIAN_POINT ( 'NONE',  ( -108.2142479086888045, -290.1277048480106373, -240.6754178707049618 ) ) ;
#56251 = CARTESIAN_POINT ( 'NONE',  ( -38.37369884090015404, -293.4651714320732481, -344.1539048664077995 ) ) ;
#56252 = CARTESIAN_POINT ( 'NONE',  ( -66.24834732509143009, -278.3504715100134490, -202.7778004026537246 ) ) ;
#56253 = CARTESIAN_POINT ( 'NONE',  ( -109.9338283156847922, -270.8452343914886455, -253.8778802156916754 ) ) ;
#56254 = CARTESIAN_POINT ( 'NONE',  ( 12.70285890476359469, -295.6520734641661647, -324.2526782947396100 ) ) ;
#56255 = CARTESIAN_POINT ( 'NONE',  ( -85.33152481854862970, -299.9090924074130839, -210.2361428286348826 ) ) ;
#56256 = CARTESIAN_POINT ( 'NONE',  ( -112.9681805602069744, -294.8988480238744501, -280.9146161741039691 ) ) ;
#56257 = CARTESIAN_POINT ( 'NONE',  ( -23.61662371915925718, -290.4740980344088825, -342.9258863462990803 ) ) ;
#56258 = CARTESIAN_POINT ( 'NONE',  ( -1.264941970054690001, -290.7639020069694311, -203.4848027728918680 ) ) ;
#56259 = ADVANCED_FACE ( 'NONE', ( #59314 ), #51716, .F. ) ;
#56260 = CARTESIAN_POINT ( 'NONE',  ( -79.88603296318224523, -292.8897146260090381, -210.2540428243744657 ) ) ;
#56261 = DIRECTION ( 'NONE',  ( -1.000000000000000000, 0.000000000000000000, 0.000000000000000000 ) ) ;
#56262 = CARTESIAN_POINT ( 'NONE',  ( -44.32577674786252686, -292.7645359449425086, -197.4828270622239756 ) ) ;
#56263 = DIRECTION ( 'NONE',  ( 0.9693563597868444237, 0.2456588035076248677, 0.000000000000000000 ) ) ;
#56264 = CARTESIAN_POINT ( 'NONE',  ( -111.9341454638480116, -291.9764053611519898, -252.9262156499200671 ) ) ;
#56266 = CARTESIAN_POINT ( 'NONE',  ( 2.240500172301783000, -292.5982639183745846, -208.9640595639771448 ) ) ;
#56265 = CARTESIAN_POINT ( 'NONE',  ( 31.67678337766244923, -279.1781233808102343, -240.1145357874084709 ) ) ;
#56267 = CARTESIAN_POINT ( 'NONE',  ( -42.43005377325469851, -279.9896423994456995, -193.5294275340110346 ) ) ;
#56268 = CARTESIAN_POINT ( 'NONE',  ( -30.22107432238242808, -282.6311090432532751, -347.0099338875499484 ) ) ;
#56269 = CARTESIAN_POINT ( 'NONE',  ( -97.25096915064618486, -287.9377561655864497, -315.2256598190316481 ) ) ;
#56270 = CARTESIAN_POINT ( 'NONE',  ( 27.54986949932021290, -279.2070033484595228, -234.3063031964529159 ) ) ;
#56271 = CARTESIAN_POINT ( 'NONE',  ( -79.78485323236849069, -283.4785847621789117, -208.4633460878366975 ) ) ;
#56272 = CARTESIAN_POINT ( 'NONE',  ( 82.64890176555634582, -299.5541904835127980, -192.9639945212225882 ) ) ;
#56273 = CARTESIAN_POINT ( 'NONE',  ( 12.55356583895141220, -279.2129172431603479, -212.6275039862651965 ) ) ;
#56274 = CARTESIAN_POINT ( 'NONE',  ( 20.06454712660518780, -285.7801732321295844, -219.4298294336416859 ) ) ;
#56275 = CARTESIAN_POINT ( 'NONE',  ( 196.4497209205300692, 41.67145302791455208, 13.67271671015795675 ) ) ;
#56276 = CARTESIAN_POINT ( 'NONE',  ( -3.284999187389276543, -294.1099210363839802, -204.8891274986903568 ) ) ;
#56277 = CARTESIAN_POINT ( 'NONE',  ( 2.098208443403834167, -275.9946387408119222, -204.9157216251434477 ) ) ;
#56278 = CARTESIAN_POINT ( 'NONE',  ( -107.8417834087898086, -277.9676861758980522, -289.3828356823390777 ) ) ;
#56279 = CARTESIAN_POINT ( 'NONE',  ( -112.9253662689182818, -290.9035425593309014, -255.5917613736295948 ) ) ;
#56280 = CARTESIAN_POINT ( 'NONE',  ( -68.61324321467263587, -281.5397302433052573, -339.1604726839812542 ) ) ;
#56281 = CARTESIAN_POINT ( 'NONE',  ( -108.9380767348257422, -289.8134852999838813, -254.9543887493984755 ) ) ;
#56282 = CARTESIAN_POINT ( 'NONE',  ( -89.34418774903762994, -293.7836561763161285, -324.4765332201062051 ) ) ;
#56283 = ORIENTED_EDGE ( 'NONE', *, *, #53042, .F. ) ;
#56284 = CARTESIAN_POINT ( 'NONE',  ( 150.4957602436334696, 20.00000000000000355, 3.637614988394419324 ) ) ;
#56285 = CARTESIAN_POINT ( 'NONE',  ( -33.49893427736539309, -291.6094427673351106, -197.3882041903070785 ) ) ;
#56286 = CYLINDRICAL_SURFACE ( 'NONE', #578, 11.40608546931776779 ) ;
#56287 = CARTESIAN_POINT ( 'NONE',  ( -67.74223827176244583, -300.1233781216987495, -207.3071070584150277 ) ) ;
#56288 = CARTESIAN_POINT ( 'NONE',  ( -105.7534716745016965, -295.1597832577228928, -305.3013691916552261 ) ) ;
#56289 = CARTESIAN_POINT ( 'NONE',  ( 32.41920201379472388, -280.0756181050880400, -300.0537876351163504 ) ) ;
#56290 = CARTESIAN_POINT ( 'NONE',  ( -112.6485215791210379, -285.6937724263038945, -284.1490872394634835 ) ) ;
#56291 = CARTESIAN_POINT ( 'NONE',  ( 35.45172209074848979, -287.4662348023951495, -276.4834481234726127 ) ) ;
#56292 = CARTESIAN_POINT ( 'NONE',  ( 24.57736227788190675, -277.6213489690156280, -310.4144435115568399 ) ) ;
#56293 = CARTESIAN_POINT ( 'NONE',  ( -110.3834894310941621, -294.7715376765541464, -254.9132797313550327 ) ) ;
#56294 = CARTESIAN_POINT ( 'NONE',  ( -58.67924790920642408, -297.0920617900294474, -341.2320081014541415 ) ) ;
#56295 = CARTESIAN_POINT ( 'NONE',  ( -76.58099912719606550, -276.3845421949446859, -332.4483759141702990 ) ) ;
#56296 = ORIENTED_EDGE ( 'NONE', *, *, #67159, .F. ) ;
#56297 = DIRECTION ( 'NONE',  ( 0.000000000000000000, 0.000000000000000000, 1.000000000000000000 ) ) ;
#56298 = CARTESIAN_POINT ( 'NONE',  ( -94.63867754377160679, -295.5210027576895300, -321.7889354388340735 ) ) ;
#56299 = CARTESIAN_POINT ( 'NONE',  ( 37.09534282965131524, -289.4809019409074153, -271.0250687287473852 ) ) ;
#56300 = CARTESIAN_POINT ( 'NONE',  ( 82.17440492340898572, -297.5479941798179766, -195.4018648718562758 ) ) ;
#56301 = CARTESIAN_POINT ( 'NONE',  ( 34.62349548100537078, -288.3727319458883471, -283.2025855520745381 ) ) ;
#56302 = ORIENTED_EDGE ( 'NONE', *, *, #12686, .F. ) ;
#56303 = CARTESIAN_POINT ( 'NONE',  ( -33.91374910648440988, -279.1530423493786088, -193.6729874459910548 ) ) ;
#56304 = CARTESIAN_POINT ( 'NONE',  ( -94.57016159653069565, -296.5055381387020930, -321.7443005989644575 ) ) ;
#56305 = CARTESIAN_POINT ( 'NONE',  ( -85.70604012864082222, -289.5309752984884994, -211.9732409193950389 ) ) ;
#56306 = CARTESIAN_POINT ( 'NONE',  ( -114.1000937285443513, -296.9665543338628595, -263.8764648965195647 ) ) ;
#56308 = CARTESIAN_POINT ( 'NONE',  ( 30.84662000572555129, -293.5366409679363073, -244.2375561265371857 ) ) ;
#56307 = AXIS2_PLACEMENT_3D ( 'NONE', #18245, #60874, #89253 ) ;
#56309 = CARTESIAN_POINT ( 'NONE',  ( 198.0020767287909962, 65.94727227685316961, -9.918438920559909278 ) ) ;
#56310 = AXIS2_PLACEMENT_3D ( 'NONE', #53921, #9895, #68135 ) ;
#56311 =( NAMED_UNIT ( * ) PLANE_ANGLE_UNIT ( ) SI_UNIT ( $, .RADIAN. ) );
#56312 = CARTESIAN_POINT ( 'NONE',  ( 197.8941236165608473, 42.00370313906616104, 9.707778735729039710 ) ) ;
#56313 = CARTESIAN_POINT ( 'NONE',  ( 11.98253380504862520, -289.9008660174117722, -328.5833448195132860 ) ) ;
#56314 = CARTESIAN_POINT ( 'NONE',  ( -19.11405058567862625, -282.7662352645559167, -190.3538533559490702 ) ) ;
#56315 = CONICAL_SURFACE ( 'NONE', #77525, 7.500000000000012434, 0.7853981633974513876 ) ;
#56316 = CARTESIAN_POINT ( 'NONE',  ( 29.66899579363884598, -281.3920319619346628, -308.1906945360046848 ) ) ;
#56317 = CARTESIAN_POINT ( 'NONE',  ( -23.70708394855249068, -284.8776729340844440, -343.9418604719035670 ) ) ;
#56318 = CARTESIAN_POINT ( 'NONE',  ( 38.75896854923772850, -286.2135528554616144, -277.2382190204973540 ) ) ;
#56320 = CARTESIAN_POINT ( 'NONE',  ( -102.9231427508413788, -288.1597575417061421, -305.6896235641398789 ) ) ;
#56319 = AXIS2_PLACEMENT_3D ( 'NONE', #84764, #56391, #62074 ) ;
#56321 = CARTESIAN_POINT ( 'NONE',  ( 37.00207179470736207, -277.2269286007979190, -255.7560141021987761 ) ) ;
#56323 = ORIENTED_EDGE ( 'NONE', *, *, #54849, .T. ) ;
#56322 = ADVANCED_FACE ( 'NONE', ( #72144 ), #36137, .F. ) ;
#56325 = CARTESIAN_POINT ( 'NONE',  ( -1.909417204406070878, -279.8833477539669161, -206.4201608802100623 ) ) ;
#56324 = CARTESIAN_POINT ( 'NONE',  ( -70.45280026804331897, -277.5014054036172411, -335.4199763150070339 ) ) ;
#56326 = CARTESIAN_POINT ( 'NONE',  ( -11.95548255968575191, -277.8091189405590171, -342.7841683369392740 ) ) ;
#56327 = CARTESIAN_POINT ( 'NONE',  ( -113.3212225893833818, -277.4747514743254442, -260.2052129746995206 ) ) ;
#56328 = CARTESIAN_POINT ( 'NONE',  ( -112.1726278936763492, -268.3392834764117652, -295.5492975640193549 ) ) ;
#56329 = CARTESIAN_POINT ( 'NONE',  ( -101.0200949150615912, -274.0609840243497501, -227.3959344430673752 ) ) ;
#56330 = EDGE_CURVE ( 'NONE', #43712, #34296, #73971, .T. ) ;
#56331 = CARTESIAN_POINT ( 'NONE',  ( -65.34311428139507427, -299.1186235670851943, -199.2093613379682040 ) ) ;
#56332 = CARTESIAN_POINT ( 'NONE',  ( -4.771743288812468897, -291.1233781216987495, -337.9199732462171255 ) ) ;
#56333 = LINE ( 'NONE', #12788, #19659 ) ;
#56334 = CARTESIAN_POINT ( 'NONE',  ( 35.06669393023508974, -288.7833723934188583, -281.8976726960947872 ) ) ;
#56335 = CARTESIAN_POINT ( 'NONE',  ( -80.38292546119866699, -287.2382810150907630, -207.6762968376524157 ) ) ;
#56336 = CARTESIAN_POINT ( 'NONE',  ( 34.66926882740423110, -286.7312232153552145, -257.4931494000165912 ) ) ;
#56337 = CARTESIAN_POINT ( 'NONE',  ( -70.44932511048989454, -282.9845510535215567, -339.8263573073675161 ) ) ;
#56338 = CARTESIAN_POINT ( 'NONE',  ( -16.67841166895991378, -278.7234554548429060, -199.5129075359699868 ) ) ;
#56339 = CARTESIAN_POINT ( 'NONE',  ( -77.74080598953176491, -287.3642007066288784, -208.0202818289762376 ) ) ;
#56340 = CARTESIAN_POINT ( 'NONE',  ( -2.807201313430653933, -278.9971878765248903, -205.2462958701118794 ) ) ;
#56341 = CARTESIAN_POINT ( 'NONE',  ( -87.41940843683433116, -279.0837538562848295, -324.1520708242007913 ) ) ;
#56342 = CARTESIAN_POINT ( 'NONE',  ( 11.79372153771742227, -276.8402246400063405, -324.5010119735229068 ) ) ;
#56343 = CARTESIAN_POINT ( 'NONE',  ( 22.08732485151113423, -286.9991296965905008, -318.7160061877781345 ) ) ;
#56344 = CARTESIAN_POINT ( 'NONE',  ( -81.46046194946160313, -284.4380496721336158, -333.3360457249852971 ) ) ;
#56345 = CARTESIAN_POINT ( 'NONE',  ( -114.1464828408261241, -284.9774276322870605, -275.7197462586422603 ) ) ;
#56346 = CARTESIAN_POINT ( 'NONE',  ( 31.06955988498283006, -281.3773405714608771, -244.7426012350530868 ) ) ;
#56347 = EDGE_LOOP ( 'NONE', ( #89239, #25276 ) ) ;
#56348 = EDGE_LOOP ( 'NONE', ( #56806, #76708 ) ) ;
#56349 = DIRECTION ( 'NONE',  ( 0.000000000000000000, 0.000000000000000000, 1.000000000000000000 ) ) ;
#56350 = CARTESIAN_POINT ( 'NONE',  ( -89.94566032384366849, -293.1796539632111376, -215.7618773006412880 ) ) ;
#56351 = CARTESIAN_POINT ( 'NONE',  ( -58.78432046757862395, -290.4652603212256849, -196.9205821417289997 ) ) ;
#56352 = CARTESIAN_POINT ( 'NONE',  ( -103.4122115735392100, -272.0367976005389323, -238.7684611663970315 ) ) ;
#56353 = CARTESIAN_POINT ( 'NONE',  ( 39.39981045361309953, -292.9718554279172054, -276.0398927534272389 ) ) ;
#56354 = CARTESIAN_POINT ( 'NONE',  ( -110.3847005139535042, -289.1646141710455709, -260.2146500376612153 ) ) ;
#56355 = CARTESIAN_POINT ( 'NONE',  ( 26.65781588813821301, -292.2950747541514716, -307.5368622444860875 ) ) ;
#56356 = CARTESIAN_POINT ( 'NONE',  ( -92.70116429069648234, -291.0731096436051644, -318.6289601620851499 ) ) ;
#56357 = DIRECTION ( 'NONE',  ( 0.000000000000000000, 0.000000000000000000, 1.000000000000000000 ) ) ;
#56358 = CARTESIAN_POINT ( 'NONE',  ( -95.71691776013170738, -291.9039756178406719, -317.4699461381828201 ) ) ;
#56359 = CARTESIAN_POINT ( 'NONE',  ( -109.4656954231785306, -288.8240063700159226, -249.1913817905198130 ) ) ;
#56360 = EDGE_CURVE ( 'NONE', #12543, #64179, #77247, .T. ) ;
#56361 = CARTESIAN_POINT ( 'NONE',  ( -111.0088617772822630, -292.7339166449121421, -256.2172616351275565 ) ) ;
#56362 = CARTESIAN_POINT ( 'NONE',  ( 2.565225255155341610, -287.5430868522681180, -208.9539054237454536 ) ) ;
#56363 = CARTESIAN_POINT ( 'NONE',  ( 36.26138935328503976, -295.3561070711276102, -255.0464579060937069 ) ) ;
#56364 = DIRECTION ( 'NONE',  ( 0.000000000000000000, 1.000000000000000000, 0.000000000000000000 ) ) ;
#56365 = DIRECTION ( 'NONE',  ( -0.000000000000000000, -1.000000000000000000, -0.000000000000000000 ) ) ;
#56366 = CARTESIAN_POINT ( 'NONE',  ( -27.24246546777073519, -276.1596564890069772, -195.6334513602025993 ) ) ;
#56367 = CARTESIAN_POINT ( 'NONE',  ( -105.8184513689372466, -295.2981803934353593, -305.3365452077952682 ) ) ;
#56368 = CARTESIAN_POINT ( 'NONE',  ( -2.415952884151053581, -272.7607832837292108, -205.1064921343491108 ) ) ;
#56369 = CARTESIAN_POINT ( 'NONE',  ( -109.2169069403395554, -276.3810697804223651, -289.7329750374756259 ) ) ;
#56370 = CARTESIAN_POINT ( 'NONE',  ( -93.22603672602734548, -274.4305195931991079, -222.7594525282359541 ) ) ;
#56371 = CARTESIAN_POINT ( 'NONE',  ( -110.6848704805083372, -297.8909408968103776, -276.9704801140501900 ) ) ;
#56372 = DIRECTION ( 'NONE',  ( -0.000000000000000000, -0.000000000000000000, 1.000000000000000000 ) ) ;
#56373 = CARTESIAN_POINT ( 'NONE',  ( -95.42348713590395448, -297.9796698452749979, -225.8535378633549442 ) ) ;
#56374 = FACE_OUTER_BOUND ( 'NONE', #61772, .T. ) ;
#56375 = VECTOR ( 'NONE', #62171, 1000.000000000000000 ) ;
#56377 = CARTESIAN_POINT ( 'NONE',  ( -97.84200078662045996, -272.9543443512566796, -229.4210500452513486 ) ) ;
#56376 = CARTESIAN_POINT ( 'NONE',  ( 17.17926379417045624, -284.8447838605778202, -218.2678467999553789 ) ) ;
#56378 = AXIS2_PLACEMENT_3D ( 'NONE', #5091, #60523, #26860 ) ;
#56379 = CARTESIAN_POINT ( 'NONE',  ( 24.70327030290053116, -286.9464343003230624, -224.7604420641200704 ) ) ;
#56380 = CARTESIAN_POINT ( 'NONE',  ( -100.6656204782153168, -289.6406795300139265, -314.1312608087405920 ) ) ;
#56381 = CARTESIAN_POINT ( 'NONE',  ( -108.3104668044043564, -298.8588096818442637, -245.0265377043011767 ) ) ;
#56382 = CARTESIAN_POINT ( 'NONE',  ( 34.50333385887570614, -291.8226894927343551, -291.3432020639249913 ) ) ;
#56383 = ADVANCED_FACE ( 'NONE', ( #38900 ), #45511, .F. ) ;
#56384 = AXIS2_PLACEMENT_3D ( 'NONE', #37482, #44119, #10001 ) ;
#56385 = CARTESIAN_POINT ( 'NONE',  ( 36.02457618131488459, -280.4618263272919876, -247.5236855309644000 ) ) ;
#56386 = EDGE_CURVE ( 'NONE', #20929, #39726, #36433, .T. ) ;
#56387 = CARTESIAN_POINT ( 'NONE',  ( 10.59707575819633618, -291.9094976428776249, -330.5268031993606428 ) ) ;
#56388 = AXIS2_PLACEMENT_3D ( 'NONE', #57622, #86945, #22097 ) ;
#56389 = CARTESIAN_POINT ( 'NONE',  ( 221.8344101925596306, -0.9999999999999997780, -22.50000000000000000 ) ) ;
#56390 = CARTESIAN_POINT ( 'NONE',  ( 16.29067623551082633, -287.0645619213318582, -320.5423392063346455 ) ) ;
#56391 = DIRECTION ( 'NONE',  ( -0.000000000000000000, -0.000000000000000000, -1.000000000000000000 ) ) ;
#56392 = CARTESIAN_POINT ( 'NONE',  ( -51.14385109387259121, -287.2282702336642046, -344.1332859679654916 ) ) ;
#56393 = CARTESIAN_POINT ( 'NONE',  ( -92.55030523426522393, -274.7630793605416670, -221.5480287987056442 ) ) ;
#56394 = CARTESIAN_POINT ( 'NONE',  ( 28.76763901231315756, -282.4752722187291170, -232.0445214468282416 ) ) ;
#56396 = CARTESIAN_POINT ( 'NONE',  ( 7.793960597335130913, -282.4162055343190900, -327.7996435053851769 ) ) ;
#56395 = CARTESIAN_POINT ( 'NONE',  ( -106.2583369648586284, -294.9711037820858905, -239.7542778171975897 ) ) ;
#56397 = CARTESIAN_POINT ( 'NONE',  ( -104.6018702781830569, -296.2316398208089367, -307.9543686941682950 ) ) ;
#56398 = CARTESIAN_POINT ( 'NONE',  ( -75.58686874495387542, -299.0523962641618709, -207.3097658321668462 ) ) ;
#56399 = CARTESIAN_POINT ( 'NONE',  ( 37.24936808194060944, -285.7897704759747626, -282.7403791609850146 ) ) ;
#56400 = CARTESIAN_POINT ( 'NONE',  ( 36.89534189518388274, -283.6893232533773812, -281.0317431091017966 ) ) ;
#56401 = CARTESIAN_POINT ( 'NONE',  ( -109.2745235932589765, -295.7925843850696879, -256.5438441849921105 ) ) ;
#56402 = ORIENTED_EDGE ( 'NONE', *, *, #54344, .F. ) ;
#56403 = DIRECTION ( 'NONE',  ( -1.000000000000000000, -0.000000000000000000, -0.000000000000000000 ) ) ;
#56404 = CARTESIAN_POINT ( 'NONE',  ( -67.19474045159624609, -285.4253656885182977, -338.7902156312812849 ) ) ;
#56405 = CARTESIAN_POINT ( 'NONE',  ( 208.4306832106271088, 0.000000000000000000, 0.000000000000000000 ) ) ;
#56406 = CARTESIAN_POINT ( 'NONE',  ( -95.99890600148557951, -293.4094976428775681, -317.0979686699210447 ) ) ;
#56407 = CARTESIAN_POINT ( 'NONE',  ( 37.74569222420570469, -274.9545116771682274, -286.7333592771032045 ) ) ;
#56408 = CARTESIAN_POINT ( 'NONE',  ( 29.85657639541818398, -293.0010133415241853, -241.7117630421124090 ) ) ;
#56409 = CARTESIAN_POINT ( 'NONE',  ( 34.32895408557164529, -283.2970485482736080, -287.5620208184632247 ) ) ;
#56410 = CARTESIAN_POINT ( 'NONE',  ( 5.881650902148037652, -278.0556472069850429, -330.2421458938829346 ) ) ;
#56411 = AXIS2_PLACEMENT_3D ( 'NONE', #33199, #69192, #70144 ) ;
#56412 = CARTESIAN_POINT ( 'NONE',  ( -105.2520809208994450, -285.5211805215334380, -305.5020222564936603 ) ) ;
#56413 = CARTESIAN_POINT ( 'NONE',  ( -107.3692767163192485, -283.0572798969670316, -292.3444985727988978 ) ) ;
#56414 = CARTESIAN_POINT ( 'NONE',  ( -104.9224074670407560, -280.1225945586293733, -303.0057886147212116 ) ) ;
#56415 = CARTESIAN_POINT ( 'NONE',  ( 36.58525964960605137, -275.4466457618862023, -248.6386858202942562 ) ) ;
#56416 = CARTESIAN_POINT ( 'NONE',  ( 39.31752326143391230, -275.2881896637475165, -262.5824542022432411 ) ) ;
#56417 = CARTESIAN_POINT ( 'NONE',  ( -15.14049336077824215, -296.6827114616025938, -341.4675825952333525 ) ) ;
#56418 = FACE_OUTER_BOUND ( 'NONE', #84895, .T. ) ;
#56419 = CARTESIAN_POINT ( 'NONE',  ( 164.6329196456214277, 250.5000000000000568, 23.09031830825856346 ) ) ;
#56420 = CARTESIAN_POINT ( 'NONE',  ( -111.9190304113460854, -294.8615671220086369, -256.9997075063920988 ) ) ;
#56421 = CARTESIAN_POINT ( 'NONE',  ( -13.77147239918030586, -276.2456213985070121, -339.5694344242997431 ) ) ;
#56422 = CARTESIAN_POINT ( 'NONE',  ( 32.78708948229623843, -295.4603535007067308, -300.5722172756474606 ) ) ;
#56423 = CARTESIAN_POINT ( 'NONE',  ( 38.21718242986301561, -294.9166731736594329, -283.0448169870533661 ) ) ;
#56424 = CARTESIAN_POINT ( 'NONE',  ( -111.0877877734702821, -292.7196854543867630, -257.3547263124657434 ) ) ;
#56425 = CARTESIAN_POINT ( 'NONE',  ( -110.9304309794785013, -276.7268931438641744, -256.7696824266112117 ) ) ;
#56426 = CARTESIAN_POINT ( 'NONE',  ( -86.45218274701142036, -281.2839572177943523, -214.4194099985491846 ) ) ;
#56427 = CARTESIAN_POINT ( 'NONE',  ( -89.52847982924940595, -293.8739317488976326, -323.5170472912803916 ) ) ;
#56428 = CARTESIAN_POINT ( 'NONE',  ( 38.38597053036861695, -283.4427150067806451, -272.7329051855021476 ) ) ;
#56429 = CARTESIAN_POINT ( 'NONE',  ( -72.51027266384272707, -284.4953637003557674, -206.0242369529304085 ) ) ;
#56430 = CARTESIAN_POINT ( 'NONE',  ( -111.2916113504647768, -274.2541639013562076, -270.3827886689474553 ) ) ;
#56431 = CARTESIAN_POINT ( 'NONE',  ( -65.09732603224448155, -285.3460844923644686, -202.7668437869050990 ) ) ;
#56432 = ORIENTED_EDGE ( 'NONE', *, *, #93286, .T. ) ;
#56433 = CARTESIAN_POINT ( 'NONE',  ( 32.11828435561940864, -283.0511563316167098, -302.9947871730552151 ) ) ;
#56434 = CIRCLE ( 'NONE', #73049, 0.5000000000000004441 ) ;
#56435 = CARTESIAN_POINT ( 'NONE',  ( -113.5106799047506456, -283.2447218810432901, -278.5033067414787524 ) ) ;
#56436 = CARTESIAN_POINT ( 'NONE',  ( -113.8106557013271072, -279.5851393093995512, -263.0482996926588726 ) ) ;
#56437 = CARTESIAN_POINT ( 'NONE',  ( -90.82911165092819772, -279.3140722481486478, -324.8575574266139938 ) ) ;
#56438 = CARTESIAN_POINT ( 'NONE',  ( -25.41958609695204885, -280.8517118272686730, -194.3928615634703476 ) ) ;
#56439 = ADVANCED_FACE ( 'NONE', ( #74919 ), #81076, .T. ) ;
#56440 = CARTESIAN_POINT ( 'NONE',  ( -102.0455923789670294, -299.4805209788416391, -239.2376011013261916 ) ) ;
#56441 = CARTESIAN_POINT ( 'NONE',  ( 195.2426427160663991, 278.4661148582146097, -125.8609867272279246 ) ) ;
#56442 = EDGE_LOOP ( 'NONE', ( #13836, #39372, #18623, #2026 ) ) ;
#56443 = AXIS2_PLACEMENT_3D ( 'NONE', #22241, #92919, #72895 ) ;
#56444 = CARTESIAN_POINT ( 'NONE',  ( -69.08280927211342259, -275.6339466775700657, -202.5788634308241001 ) ) ;
#56445 = CARTESIAN_POINT ( 'NONE',  ( 153.0615653321293905, 207.2999644492867048, -217.0734274107136628 ) ) ;
#56446 = AXIS2_PLACEMENT_3D ( 'NONE', #23132, #52015, #80901 ) ;
#56447 = CARTESIAN_POINT ( 'NONE',  ( -4.819586325188885745, -278.5027187778517259, -203.1736271744400710 ) ) ;
#56448 = CARTESIAN_POINT ( 'NONE',  ( -8.911432685590609637, -294.1791215237471988, -199.8934381040679398 ) ) ;
#56449 = CARTESIAN_POINT ( 'NONE',  ( 34.58495855550241060, -292.7278342509392814, -257.2358790163861499 ) ) ;
#56450 = CARTESIAN_POINT ( 'NONE',  ( -95.41597551512251130, -289.3771266694707833, -320.8279926791381627 ) ) ;
#56451 = FACE_OUTER_BOUND ( 'NONE', #78324, .T. ) ;
#56453 = CARTESIAN_POINT ( 'NONE',  ( -38.61853276064386620, -284.4357829947898040, -196.5595426480916217 ) ) ;
#56452 = CARTESIAN_POINT ( 'NONE',  ( 0.2348002737982404775, -293.1366900232138732, -336.9089753550182991 ) ) ;
#56454 = CARTESIAN_POINT ( 'NONE',  ( -102.2144349037427702, -292.8990378016016507, -234.1667847760658674 ) ) ;
#56455 = CARTESIAN_POINT ( 'NONE',  ( -109.4602149205049528, -285.6819473107316298, -284.5090260726261704 ) ) ;
#56456 = VERTEX_POINT ( 'NONE', #37965 ) ;
#56457 = CARTESIAN_POINT ( 'NONE',  ( -53.35198213959034774, -292.7930332494909180, -195.2302170355795283 ) ) ;
#56458 = AXIS2_PLACEMENT_3D ( 'NONE', #73622, #59893, #46117 ) ;
#56459 = CARTESIAN_POINT ( 'NONE',  ( -36.18627523469005780, -283.5296266779871530, -343.4135199634243349 ) ) ;
#56460 = CARTESIAN_POINT ( 'NONE',  ( 21.05494722386966799, -293.0188515772367168, -319.9377283723553660 ) ) ;
#56461 = CARTESIAN_POINT ( 'NONE',  ( 23.16664006803374676, -288.9895226902963259, -317.7415681150929458 ) ) ;
#56462 = EDGE_CURVE ( 'NONE', #73850, #44442, #31896, .T. ) ;
#56463 = CARTESIAN_POINT ( 'NONE',  ( -97.23821350659802931, -290.3964065975628159, -318.6720014105655423 ) ) ;
#56464 = CARTESIAN_POINT ( 'NONE',  ( 21.17475724337224818, -288.3314498388709239, -314.0263356679111553 ) ) ;
#56465 = VERTEX_POINT ( 'NONE', #53601 ) ;
#56466 = LINE ( 'NONE', #11004, #6492 ) ;
#56467 = CARTESIAN_POINT ( 'NONE',  ( -110.4368107183282319, -298.6685435892064788, -250.2318759761165268 ) ) ;
#56468 = AXIS2_PLACEMENT_3D ( 'NONE', #54788, #10768, #74723 ) ;
#56469 = CARTESIAN_POINT ( 'NONE',  ( -34.76316277018695899, -296.7686317458075109, -193.8548274820176971 ) ) ;
#56470 = CARTESIAN_POINT ( 'NONE',  ( -7.893869019877665316, -279.5064529411663443, -203.2934392616369905 ) ) ;
#56471 = CARTESIAN_POINT ( 'NONE',  ( -68.81315215092013204, -273.1570677097084854, -200.1393663240377236 ) ) ;
#56472 = CARTESIAN_POINT ( 'NONE',  ( -23.40652372552063909, -293.3507748869216130, -342.7770037375145762 ) ) ;
#56473 = CARTESIAN_POINT ( 'NONE',  ( 12.20852345766576086, -276.5126371984072193, -215.3125929431929251 ) ) ;
#56474 = CARTESIAN_POINT ( 'NONE',  ( -33.72794539926945134, -296.3378518967315927, -196.3488791081413183 ) ) ;
#56475 = CARTESIAN_POINT ( 'NONE',  ( -15.45989597189430675, -295.9677482840294260, -340.4739651587536855 ) ) ;
#56476 = CARTESIAN_POINT ( 'NONE',  ( -78.11027596536193585, -296.6938778292721963, -331.3498351730605691 ) ) ;
#56477 = DIRECTION ( 'NONE',  ( 0.000000000000000000, 0.000000000000000000, -1.000000000000000000 ) ) ;
#56478 = CARTESIAN_POINT ( 'NONE',  ( -50.31110161546963866, -296.8150499799922954, -345.5026824115543036 ) ) ;
#56479 = AXIS2_PLACEMENT_3D ( 'NONE', #37259, #81272, #73720 ) ;
#56480 = CARTESIAN_POINT ( 'NONE',  ( -95.90164498658693049, -295.1990049693231413, -223.2361639816649301 ) ) ;
#56481 = CARTESIAN_POINT ( 'NONE',  ( -9.696609853111157307, -293.0743696447640332, -202.6342113768496915 ) ) ;
#56482 = CARTESIAN_POINT ( 'NONE',  ( -87.93774596085788176, -274.1687926498977390, -212.4613197160124116 ) ) ;
#56483 = CARTESIAN_POINT ( 'NONE',  ( -88.32584239325321107, -289.8959332430033555, -217.2247908743093490 ) ) ;
#56484 = CARTESIAN_POINT ( 'NONE',  ( -38.12820669670584550, -276.0424522993371284, -195.3652376922328244 ) ) ;
#56485 = CARTESIAN_POINT ( 'NONE',  ( -105.5572855983578933, -273.5051798885942844, -234.6627992068795834 ) ) ;
#56486 = CARTESIAN_POINT ( 'NONE',  ( -93.63258947546353284, -297.5447957752236903, -223.8290509811140510 ) ) ;
#56487 = EDGE_CURVE ( 'NONE', #14431, #90108, #31362, .T. ) ;
#56488 = CARTESIAN_POINT ( 'NONE',  ( -28.44476837229287725, -282.1442415856832326, -195.4804942847801783 ) ) ;
#56489 = CARTESIAN_POINT ( 'NONE',  ( 19.77177666151919055, -279.5422357415955616, -219.4361193334763414 ) ) ;
#56490 = CIRCLE ( 'NONE', #5029, 9.550761578869391144 ) ;
#56491 = CARTESIAN_POINT ( 'NONE',  ( -89.14956780075755205, -277.1071420590648700, -327.1876754494122110 ) ) ;
#56492 = CARTESIAN_POINT ( 'NONE',  ( 37.20630972042400231, -279.7518070603735509, -254.5177861087676376 ) ) ;
#56493 = CARTESIAN_POINT ( 'NONE',  ( 5.850221493657672411, -280.4684074958502151, -331.9429301148162494 ) ) ;
#56494 = CARTESIAN_POINT ( 'NONE',  ( -66.02621890771744972, -272.2439711651368839, -202.5925906230976352 ) ) ;
#56495 = CARTESIAN_POINT ( 'NONE',  ( -54.22143493831853789, -279.2689642414715649, -343.4896148003367671 ) ) ;
#56496 = CARTESIAN_POINT ( 'NONE',  ( 196.0143093133015384, 20.19615242270662847, 11.99999999999998934 ) ) ;
#56497 = CARTESIAN_POINT ( 'NONE',  ( 208.4306832106271088, 20.44233620800389772, 0.000000000000000000 ) ) ;
#56498 = CARTESIAN_POINT ( 'NONE',  ( -96.54257871092923438, -295.4389853515199320, -222.7246824237597593 ) ) ;
#56499 = CARTESIAN_POINT ( 'NONE',  ( -5.280555885609304667, -290.4920756620618363, -202.1666179325429482 ) ) ;
#56500 = CARTESIAN_POINT ( 'NONE',  ( -86.51303194554405707, -291.3910918651312727, -211.0366747779846150 ) ) ;
#56501 = CARTESIAN_POINT ( 'NONE',  ( 36.92842868515545263, -277.7047962698657670, -282.2633088143482496 ) ) ;
#56502 = CARTESIAN_POINT ( 'NONE',  ( -43.62496007597515302, -271.9727322638058808, -195.5726732523458509 ) ) ;
#56503 = EDGE_CURVE ( 'NONE', #48026, #87609, #81981, .T. ) ;
#56504 = FACE_OUTER_BOUND ( 'NONE', #39397, .T. ) ;
#56505 = CARTESIAN_POINT ( 'NONE',  ( -35.90165130381072345, -284.9544062847471650, -345.9202695840223782 ) ) ;
#56506 = DIRECTION ( 'NONE',  ( 0.000000000000000000, 0.000000000000000000, -1.000000000000000000 ) ) ;
#56507 = CARTESIAN_POINT ( 'NONE',  ( -24.98171654488527338, -284.2094912620926834, -196.3347462400582515 ) ) ;
#56508 = CARTESIAN_POINT ( 'NONE',  ( -12.89035065966967508, -293.5222210471893050, -339.6191550207059322 ) ) ;
#56509 = CARTESIAN_POINT ( 'NONE',  ( 35.20812380990154367, -285.4877021766924940, -254.6325284008937899 ) ) ;
#56510 = DIRECTION ( 'NONE',  ( 1.000000000000000000, 0.000000000000000000, -0.000000000000000000 ) ) ;
#56511 = CARTESIAN_POINT ( 'NONE',  ( -25.92748607628257318, -292.9066093403312721, -344.4874720277475717 ) ) ;
#56512 = CARTESIAN_POINT ( 'NONE',  ( -97.50978271558163613, -282.3993071669198116, -317.2920203087631990 ) ) ;
#56513 = CARTESIAN_POINT ( 'NONE',  ( -66.40329534439872816, -281.2653028192255533, -202.5102867880562485 ) ) ;
#56514 = CARTESIAN_POINT ( 'NONE',  ( -102.1905362386951737, -286.2939159587666609, -229.5856698161211682 ) ) ;
#56515 = CARTESIAN_POINT ( 'NONE',  ( 36.35402916168109755, -279.5572344014840951, -251.8431942062244104 ) ) ;
#56516 = CARTESIAN_POINT ( 'NONE',  ( 17.77618855459306957, -286.8697964585653040, -222.4965345500855278 ) ) ;
#56517 = CIRCLE ( 'NONE', #20195, 2.397123461337413719 ) ;
#56518 = CARTESIAN_POINT ( 'NONE',  ( -110.5542632014368820, -280.0811463999183388, -262.4354489847819991 ) ) ;
#56519 = CARTESIAN_POINT ( 'NONE',  ( -95.39492501369525712, -278.7299412020260547, -314.8855473203295787 ) ) ;
#56520 = CARTESIAN_POINT ( 'NONE',  ( -72.86051582443228369, -287.5642994051705728, -203.8441525607969425 ) ) ;
#56521 = EDGE_CURVE ( 'NONE', #83682, #24951, #70031, .T. ) ;
#56522 = EDGE_LOOP ( 'NONE', ( #22634, #47781 ) ) ;
#56523 = VECTOR ( 'NONE', #13610, 1000.000000000000000 ) ;
#56524 = CARTESIAN_POINT ( 'NONE',  ( -62.84304624642552994, -297.5624462130562051, -197.7065837080185418 ) ) ;
#56525 = CARTESIAN_POINT ( 'NONE',  ( 4.558267796475975686, -290.4639752367180563, -332.1991768912891985 ) ) ;
#56526 = CARTESIAN_POINT ( 'NONE',  ( 175.2296996224750103, 154.6894116713782807, 20.15985230015483154 ) ) ;
#56527 = CARTESIAN_POINT ( 'NONE',  ( 35.59421657381088266, -301.4082689599840705, -190.3320873922940848 ) ) ;
#56528 = ORIENTED_EDGE ( 'NONE', *, *, #30594, .T. ) ;
#56529 = CARTESIAN_POINT ( 'NONE',  ( -27.21761594896082670, -272.1802448863628570, -195.8272071098441245 ) ) ;
#56530 = CARTESIAN_POINT ( 'NONE',  ( 36.31459455635539513, -291.7044576063424870, -250.7866194261436021 ) ) ;
#56531 = CARTESIAN_POINT ( 'NONE',  ( -110.4436330666481183, -271.9008437819409210, -270.3528433432777547 ) ) ;
#56532 = CIRCLE ( 'NONE', #35358, 0.9999999999999955591 ) ;
#56533 = CARTESIAN_POINT ( 'NONE',  ( -80.80092267947240714, -291.1737327556389232, -329.9393408022421568 ) ) ;
#56534 = CARTESIAN_POINT ( 'NONE',  ( -27.44476216906243593, -281.9396152701979190, -196.9605669658214140 ) ) ;
#56535 = CARTESIAN_POINT ( 'NONE',  ( -37.48214759217880498, -290.4791072874975839, -346.7847344300932946 ) ) ;
#56536 = CARTESIAN_POINT ( 'NONE',  ( -103.3643333324506983, -291.3597523499364570, -309.1221744869474719 ) ) ;
#56537 = CARTESIAN_POINT ( 'NONE',  ( -16.64372211822849579, -288.3195797906191160, -198.2194200888332034 ) ) ;
#56538 = CARTESIAN_POINT ( 'NONE',  ( 12.99056856368130042, -280.8994477234854230, -212.0888026619383595 ) ) ;
#56539 = CARTESIAN_POINT ( 'NONE',  ( -41.88390723272224392, -293.1886797296315308, -345.8358864541437470 ) ) ;
#56540 = CARTESIAN_POINT ( 'NONE',  ( 1.375809934639267373, -280.3874398222892523, -203.7425091662561556 ) ) ;
#56541 = AXIS2_PLACEMENT_3D ( 'NONE', #41300, #20017, #27127 ) ;
#56542 = CARTESIAN_POINT ( 'NONE',  ( 27.86284381676375688, -277.8901445823409517, -305.9543124942162535 ) ) ;
#56543 = VECTOR ( 'NONE', #92618, 1000.000000000000114 ) ;
#56544 = CARTESIAN_POINT ( 'NONE',  ( -54.42813229853333468, -297.7662352645559167, -345.3683826091709648 ) ) ;
#56545 = CARTESIAN_POINT ( 'NONE',  ( 35.51540069524032361, -274.0669267218495975, -291.9897697811916260 ) ) ;
#56546 = CARTESIAN_POINT ( 'NONE',  ( 33.01701867748859343, -281.3198119650901958, -290.0496712513210014 ) ) ;
#56547 = CIRCLE ( 'NONE', #35373, 2.000000000000001776 ) ;
#56548 = CARTESIAN_POINT ( 'NONE',  ( -62.26223509124600497, -278.5741516955810653, -342.8531424128390768 ) ) ;
#56549 = CARTESIAN_POINT ( 'NONE',  ( -69.72323517981750740, -274.9317332416228510, -204.3862768131380108 ) ) ;
#56550 = CARTESIAN_POINT ( 'NONE',  ( -99.14764263528250865, -284.2186387920868924, -224.7451580521282324 ) ) ;
#56551 = CARTESIAN_POINT ( 'NONE',  ( -111.3180478612490987, -292.2652082137114462, -273.9805566028367707 ) ) ;
#56552 = CARTESIAN_POINT ( 'NONE',  ( -109.3525769114165058, -274.4697063331597064, -245.4437738324730276 ) ) ;
#56553 = ADVANCED_FACE ( 'NONE', ( #74430 ), #25180, .F. ) ;
#56554 = CARTESIAN_POINT ( 'NONE',  ( -87.72428621854042774, -274.6810516230699477, -212.7155593108392679 ) ) ;
#56555 = CARTESIAN_POINT ( 'NONE',  ( 199.7700033442230279, 63.22432295887225706, 10.15684170342042236 ) ) ;
#56556 = CARTESIAN_POINT ( 'NONE',  ( -107.5341244964257754, -298.8914970360070242, -244.2682663688783578 ) ) ;
#56557 = CARTESIAN_POINT ( 'NONE',  ( -96.58302693451905441, -281.9238446275705314, -316.1039603026502505 ) ) ;
#56558 = CARTESIAN_POINT ( 'NONE',  ( -103.1955543923324967, -290.7404473726354581, -230.3959139943439993 ) ) ;
#56559 = CARTESIAN_POINT ( 'NONE',  ( 37.23162044898293743, -273.5168815500396704, -266.0689725091951345 ) ) ;
#56560 = CARTESIAN_POINT ( 'NONE',  ( 11.91438134250634029, -289.9808595601708703, -328.5012835449879844 ) ) ;
#56561 = VECTOR ( 'NONE', #91666, 1000.000000000000000 ) ;
#56562 = CARTESIAN_POINT ( 'NONE',  ( -104.9829945871630770, -289.8516009614157838, -241.9645871083978648 ) ) ;
#56563 = VERTEX_POINT ( 'NONE', #53114 ) ;
#56564 = CARTESIAN_POINT ( 'NONE',  ( -113.7789321490720056, -289.1522021094442039, -268.3519541098652326 ) ) ;
#56565 = CARTESIAN_POINT ( 'NONE',  ( -98.13062750240479204, -289.6571539803717883, -310.8411915928285794 ) ) ;
#56566 = EDGE_LOOP ( 'NONE', ( #83401, #83913 ) ) ;
#56567 = CARTESIAN_POINT ( 'NONE',  ( 2.568367604407467919, -287.6537790870643789, -204.8731114234594202 ) ) ;
#56568 = CARTESIAN_POINT ( 'NONE',  ( -79.07042575173363730, -279.8050455313261295, -210.4378258122584100 ) ) ;
#56569 = CARTESIAN_POINT ( 'NONE',  ( -32.04762914715821864, -293.9072002357380029, -346.8822621854082513 ) ) ;
#56570 = CARTESIAN_POINT ( 'NONE',  ( -44.40158332319210643, -283.7905138198533450, -346.9877081854161247 ) ) ;
#56571 = CARTESIAN_POINT ( 'NONE',  ( -71.06079909490395607, -285.9525316224593894, -201.1602028402355984 ) ) ;
#56572 = CARTESIAN_POINT ( 'NONE',  ( -48.32767700335139693, -283.5291232961614583, -342.5511158964246761 ) ) ;
#56573 = CARTESIAN_POINT ( 'NONE',  ( 139.0626142690745723, 180.5554732948571655, -241.5151996274486237 ) ) ;
#56574 = CARTESIAN_POINT ( 'NONE',  ( -110.7569340398763842, -265.4859700393970456, -306.5498943703896657 ) ) ;
#56575 = CARTESIAN_POINT ( 'NONE',  ( 201.3568388210140370, 292.7455855533186195, -68.23575430854765500 ) ) ;
#56576 = CARTESIAN_POINT ( 'NONE',  ( -2.828471751044380866, -273.7179372179217580, -205.8519031810168087 ) ) ;
#56577 = CARTESIAN_POINT ( 'NONE',  ( 5.367948354894304330, -273.5654586165605906, -210.7155518452954936 ) ) ;
#56578 = CARTESIAN_POINT ( 'NONE',  ( -92.65712151590203405, -295.3266424335277520, -323.8375713043415658 ) ) ;
#56579 = CARTESIAN_POINT ( 'NONE',  ( -69.08132297861465076, -196.6430596737640712, -357.2208136483789076 ) ) ;
#56580 = CARTESIAN_POINT ( 'NONE',  ( 19.67958836871779127, -273.5400615760668757, -219.2747051178490381 ) ) ;
#56581 = CARTESIAN_POINT ( 'NONE',  ( -99.49450015584253038, -298.9668567094116725, -229.6737800469756792 ) ) ;
#56582 = CARTESIAN_POINT ( 'NONE',  ( -62.92141544937182829, -292.7907688724012587, -201.6595587741367979 ) ) ;
#56583 = ORIENTED_EDGE ( 'NONE', *, *, #20778, .T. ) ;
#56584 = CARTESIAN_POINT ( 'NONE',  ( -98.91092185458170150, -298.1052951054733740, -224.4910436230923949 ) ) ;
#56585 = CARTESIAN_POINT ( 'NONE',  ( -10.69581716216383072, -289.1874996820229740, -338.4446794674656758 ) ) ;
#56586 = CARTESIAN_POINT ( 'NONE',  ( 39.27927957544802240, -294.2825703586752866, -264.5832040531956295 ) ) ;
#56587 = CARTESIAN_POINT ( 'NONE',  ( -96.46010517989168420, -296.3814511626835611, -319.6212304622717397 ) ) ;
#56588 = CARTESIAN_POINT ( 'NONE',  ( 35.29510435112290168, -293.6164485697258897, -262.5998051288544843 ) ) ;
#56589 = ORIENTED_EDGE ( 'NONE', *, *, #17514, .F. ) ;
#56590 = CARTESIAN_POINT ( 'NONE',  ( 37.94776876029222734, -277.5537237777252813, -276.7493940130202645 ) ) ;
#56591 = EDGE_LOOP ( 'NONE', ( #90569, #38837, #44570, #68411 ) ) ;
#56592 = CARTESIAN_POINT ( 'NONE',  ( -111.3830037309397341, -277.7974794228832707, -291.2755212521244061 ) ) ;
#56593 = VECTOR ( 'NONE', #91610, 1000.000000000000000 ) ;
#56594 = CARTESIAN_POINT ( 'NONE',  ( -8.890452257546689552, -275.3748145659170063, -202.8241881520525283 ) ) ;
#56595 = CARTESIAN_POINT ( 'NONE',  ( -29.95992034420097383, -275.9045097189990656, -194.7338521300180787 ) ) ;
#56596 = CARTESIAN_POINT ( 'NONE',  ( -111.6110347286899156, -276.7351536699262056, -257.6146383805146911 ) ) ;
#56597 = CARTESIAN_POINT ( 'NONE',  ( -101.3077607516715943, -297.6865292886304815, -234.9741746814539169 ) ) ;
#56598 = CARTESIAN_POINT ( 'NONE',  ( -82.73744520628724786, -294.2610853438101230, -328.3450185199600355 ) ) ;
#56599 = CARTESIAN_POINT ( 'NONE',  ( 11.63197158325052172, -331.8906705383788562, 47.50000000000000711 ) ) ;
#56600 = CARTESIAN_POINT ( 'NONE',  ( -111.6732019855097917, -279.2939137386276798, -250.4518718852628467 ) ) ;
#56601 = CARTESIAN_POINT ( 'NONE',  ( -40.50364157120243647, -277.2596628575806790, -343.3050716355485861 ) ) ;
#56602 = VECTOR ( 'NONE', #74283, 1000.000000000000000 ) ;
#56603 = CARTESIAN_POINT ( 'NONE',  ( 30.98891363689950751, -285.7913260709609062, -235.9485404281858223 ) ) ;
#56604 = CARTESIAN_POINT ( 'NONE',  ( -36.93558507469707308, -300.0573805613046829, -195.1943045490916404 ) ) ;
#56605 = DIRECTION ( 'NONE',  ( 0.000000000000000000, 1.000000000000000000, 0.000000000000000000 ) ) ;
#56606 = CARTESIAN_POINT ( 'NONE',  ( 31.12933071685829134, -286.4044262406529811, -244.4436543141399625 ) ) ;
#56607 = AXIS2_PLACEMENT_3D ( 'NONE', #65430, #7630, #1925 ) ;
#56608 = EDGE_CURVE ( 'NONE', #85445, #92893, #59148, .T. ) ;
#56609 = CARTESIAN_POINT ( 'NONE',  ( 21.33280694625357654, -279.1655884264935139, -225.2264748078117123 ) ) ;
#56611 = CARTESIAN_POINT ( 'NONE',  ( -104.3187816133379897, -282.1993325540425417, -302.9662659308841626 ) ) ;
#56610 = CARTESIAN_POINT ( 'NONE',  ( -109.4611051303957936, -277.3192106689721186, -255.6634924303688479 ) ) ;
#56612 = CARTESIAN_POINT ( 'NONE',  ( -84.69704586883723607, -287.4002016735916527, -212.1358925805832030 ) ) ;
#56613 = CARTESIAN_POINT ( 'NONE',  ( 22.79997389512574557, -277.3418080879433205, -312.5210676675291666 ) ) ;
#56614 = DIRECTION ( 'NONE',  ( 0.000000000000000000, 1.000000000000000000, 0.000000000000000000 ) ) ;
#56616 = CARTESIAN_POINT ( 'NONE',  ( -105.4472355744958065, -276.3517999464380637, -304.1783846911034743 ) ) ;
#56615 = TOROIDAL_SURFACE ( 'NONE', #64203, 12.68950434577434372, 1.000000000000000000 ) ;
#56617 = CARTESIAN_POINT ( 'NONE',  ( 13.56169881221938489, -275.4397658221436131, -217.8945891822620808 ) ) ;
#56618 = CARTESIAN_POINT ( 'NONE',  ( 29.08933421837456734, -283.0857735416603305, -235.0799766736670051 ) ) ;
#56619 = DIRECTION ( 'NONE',  ( -0.000000000000000000, 1.000000000000000000, -0.000000000000000000 ) ) ;
#56620 = CARTESIAN_POINT ( 'NONE',  ( 4.775329806740725935, -290.4082781498609620, -333.0944423448184466 ) ) ;
#56621 = CARTESIAN_POINT ( 'NONE',  ( -104.9225891928995651, -294.9816826268902332, -237.7187071093943871 ) ) ;
#56622 = AXIS2_PLACEMENT_3D ( 'NONE', #69668, #20428, #33210 ) ;
#56623 = DIRECTION ( 'NONE',  ( 0.7484200282493165268, 0.000000000000000000, 0.6632250457539224930 ) ) ;
#56624 = CARTESIAN_POINT ( 'NONE',  ( -38.07055923495801153, -272.7276544548315655, -196.8715796523499080 ) ) ;
#56625 = CARTESIAN_POINT ( 'NONE',  ( 21.99514713599179672, -291.0757618644705644, -225.7516566589829381 ) ) ;
#56626 = CARTESIAN_POINT ( 'NONE',  ( 172.7732574597264659, 233.5132621949535121, -195.2123807395911399 ) ) ;
#56627 = CARTESIAN_POINT ( 'NONE',  ( 197.0790555737925445, 71.90044526202932218, -12.15580537966067354 ) ) ;
#56628 = CARTESIAN_POINT ( 'NONE',  ( -112.1917270975734624, -288.8439368079679070, -285.2659359728676236 ) ) ;
#56629 = CARTESIAN_POINT ( 'NONE',  ( 36.73684395173320638, -285.5769064336103611, -253.3816119969115732 ) ) ;
#56630 = EDGE_CURVE ( 'NONE', #66913, #783, #81994, .T. ) ;
#56631 = CARTESIAN_POINT ( 'NONE',  ( -110.5827305937359881, -286.0775974361200724, -262.7066584158793603 ) ) ;
#56632 = CARTESIAN_POINT ( 'NONE',  ( -90.85260795954805246, -284.6390734000214593, -320.2528454543183898 ) ) ;
#56633 = CARTESIAN_POINT ( 'NONE',  ( -107.9418819357910451, -292.8741932966008221, -243.8680003984145799 ) ) ;
#56634 = CARTESIAN_POINT ( 'NONE',  ( 26.42028899075831561, -274.1746367024695132, -311.0011806984875875 ) ) ;
#56635 = CARTESIAN_POINT ( 'NONE',  ( 16.94332650267006457, -276.6379205362107427, -325.0146732586167104 ) ) ;
#56636 = CARTESIAN_POINT ( 'NONE',  ( -104.7089585797346984, -289.0822963016607900, -236.0264345020260350 ) ) ;
#56637 = CARTESIAN_POINT ( 'NONE',  ( -95.21079124202668709, -277.8647645372290071, -321.1564749913054015 ) ) ;
#56638 = CARTESIAN_POINT ( 'NONE',  ( -66.67683049721047439, -297.4182497981705069, -339.0000058740760664 ) ) ;
#56639 = CARTESIAN_POINT ( 'NONE',  ( -48.18343439340156209, -251.9247748416627530, -488.0338856575309592 ) ) ;
#56640 = CYLINDRICAL_SURFACE ( 'NONE', #82844, 25.00000000000000355 ) ;
#56641 = CARTESIAN_POINT ( 'NONE',  ( -108.9093421591220192, -283.0173313112684923, -287.1289103747615741 ) ) ;
#56642 = CARTESIAN_POINT ( 'NONE',  ( -98.60032658439844511, -277.1398641000526482, -227.0900960997149411 ) ) ;
#56643 = DIRECTION ( 'NONE',  ( -0.6056179655966478226, 0.7957555401921982963, -0.000000000000000000 ) ) ;
#56644 = CARTESIAN_POINT ( 'NONE',  ( 27.91971080898837698, -273.5100438833234762, -230.7169739896940257 ) ) ;
#56645 = CARTESIAN_POINT ( 'NONE',  ( -96.17997698430839648, -277.2933346036577404, -313.7635487079500081 ) ) ;
#56646 = CARTESIAN_POINT ( 'NONE',  ( 26.40199734520895802, -295.5748096586437441, -307.3401496571643179 ) ) ;
#56647 = CARTESIAN_POINT ( 'NONE',  ( 3.668340451276424830, -279.5100976521551388, -205.4935287854272588 ) ) ;
#56648 = CARTESIAN_POINT ( 'NONE',  ( -61.07813073046070684, -296.3091108082808773, -339.6968242111963150 ) ) ;
#56649 = EDGE_CURVE ( 'NONE', #86001, #91341, #30406, .T. ) ;
#56650 = CARTESIAN_POINT ( 'NONE',  ( -92.33084088443780502, -297.1338721407038292, -323.5540937528919585 ) ) ;
#56651 = CARTESIAN_POINT ( 'NONE',  ( -109.1497171808796338, -272.3972409699225636, -256.8356854507570119 ) ) ;
#56652 = CARTESIAN_POINT ( 'NONE',  ( -67.38807564903632397, -293.6582444505723970, -201.6427363848794130 ) ) ;
#56653 = CARTESIAN_POINT ( 'NONE',  ( -97.58172773319931537, -285.3609251400712310, -222.4013527759471174 ) ) ;
#56654 = CARTESIAN_POINT ( 'NONE',  ( -36.92238861510700332, -272.1969721148030317, -194.5846314150446972 ) ) ;
#56655 = CARTESIAN_POINT ( 'NONE',  ( 37.82448045515723578, -287.5951405168726183, -287.1259539487356847 ) ) ;
#56656 = CARTESIAN_POINT ( 'NONE',  ( -97.75134497261254296, -281.1321173282420887, -226.5145489663710521 ) ) ;
#56657 = CARTESIAN_POINT ( 'NONE',  ( -89.82313244521755280, -284.3478701727402154, -219.2089320493205378 ) ) ;
#56658 = CARTESIAN_POINT ( 'NONE',  ( -96.59559146607324465, -287.9216386140500390, -316.3391237484386806 ) ) ;
#56659 = CARTESIAN_POINT ( 'NONE',  ( -43.41528170534920861, -158.9639970630164498, -364.8434004397808508 ) ) ;
#56660 = CARTESIAN_POINT ( 'NONE',  ( 18.71300612636314042, -286.3950498778984297, -223.4816383385648635 ) ) ;
#56661 = CARTESIAN_POINT ( 'NONE',  ( -31.64176327053335669, -283.9231350776951217, -346.9271437445970037 ) ) ;
#56662 = CARTESIAN_POINT ( 'NONE',  ( -112.0854227277996813, -289.8304251048978131, -252.8626567332632362 ) ) ;
#56663 = CARTESIAN_POINT ( 'NONE',  ( -79.48547497314076793, -281.0937453553920022, -206.8128319637202992 ) ) ;
#56664 = CARTESIAN_POINT ( 'NONE',  ( -113.2746445971862101, -279.7443217125004367, -280.1332313332333115 ) ) ;
#56665 = CARTESIAN_POINT ( 'NONE',  ( 35.42883406461619700, -281.4697939825421713, -276.7532527611465412 ) ) ;
#56666 = CARTESIAN_POINT ( 'NONE',  ( 34.00849916627620217, -277.8507559612054933, -293.4727970487795687 ) ) ;
#56667 = CARTESIAN_POINT ( 'NONE',  ( -50.46752206666486273, -295.2151791643698857, -346.2880673641592466 ) ) ;
#56668 = CARTESIAN_POINT ( 'NONE',  ( -97.90762704143034512, -287.9755737448996342, -313.9915580636235859 ) ) ;
#56669 = CARTESIAN_POINT ( 'NONE',  ( -110.3568607010007980, -295.5658071095648438, -263.2560802976551599 ) ) ;
#56670 = ORIENTED_EDGE ( 'NONE', *, *, #19214, .F. ) ;
#56671 = ORIENTED_EDGE ( 'NONE', *, *, #28405, .F. ) ;
#56672 = CARTESIAN_POINT ( 'NONE',  ( 4.213975851907634684, -284.4078084029300726, -332.1846355355074820 ) ) ;
#56673 = CARTESIAN_POINT ( 'NONE',  ( -86.50734310374677705, -295.4247318932015105, -324.3502561261821029 ) ) ;
#56674 = CARTESIAN_POINT ( 'NONE',  ( 26.22893654932757457, -294.0632163582802718, -227.3693946471298659 ) ) ;
#56675 = AXIS2_PLACEMENT_3D ( 'NONE', #65377, #36934, #66741 ) ;
#56676 = CARTESIAN_POINT ( 'NONE',  ( -8.446326822210314944, -283.3150140821632021, -337.5098340531724830 ) ) ;
#56677 = CARTESIAN_POINT ( 'NONE',  ( -52.48743207520171694, -272.9216056904402876, -195.0511010066886968 ) ) ;
#56678 = CARTESIAN_POINT ( 'NONE',  ( -91.52081670784414769, -290.4502124374193954, -325.0064848991340227 ) ) ;
#56679 = CARTESIAN_POINT ( 'NONE',  ( -44.32927892556214999, -281.2790897366164700, -345.8555132341144258 ) ) ;
#56680 = CARTESIAN_POINT ( 'NONE',  ( -114.3477987538904870, -290.9104725861690781, -268.3594982842531067 ) ) ;
#56681 = CARTESIAN_POINT ( 'NONE',  ( -18.46394633714706757, -289.1355902506487041, -340.9524886010027558 ) ) ;
#56682 = CARTESIAN_POINT ( 'NONE',  ( 199.4392256788250677, 65.82574266882504332, 7.741079165001067963 ) ) ;
#56683 = FACE_OUTER_BOUND ( 'NONE', #55277, .T. ) ;
#56684 = CARTESIAN_POINT ( 'NONE',  ( 189.0190693845576391, 268.0883035360336635, -137.5188113462812680 ) ) ;
#56685 = CARTESIAN_POINT ( 'NONE',  ( -95.95921662488163406, -288.6952119285919025, -223.5744983911110353 ) ) ;
#56686 = ORIENTED_EDGE ( 'NONE', *, *, #80835, .F. ) ;
#56687 = CARTESIAN_POINT ( 'NONE',  ( -96.64771065340420364, -278.0730481389181250, -227.2679260633267404 ) ) ;
#56688 = CARTESIAN_POINT ( 'NONE',  ( 4.855119491839677615, -274.2717736081243061, -205.9148560242031465 ) ) ;
#56689 = CARTESIAN_POINT ( 'NONE',  ( -111.9953344657296270, -280.4765637467240822, -276.2478437392741739 ) ) ;
#56690 = CARTESIAN_POINT ( 'NONE',  ( -106.9267777310214598, -266.4941316993138685, -306.1134506589970101 ) ) ;
#56691 = CARTESIAN_POINT ( 'NONE',  ( 25.80400527064101723, -279.5540061349556140, -227.2428875975125209 ) ) ;
#56692 = CARTESIAN_POINT ( 'NONE',  ( -37.57032110175317285, -281.0751734034562901, -345.0182820352854378 ) ) ;
#56693 = CARTESIAN_POINT ( 'NONE',  ( -105.6128327790994206, -298.7463959362008836, -236.9990668191579744 ) ) ;
#56694 = AXIS2_PLACEMENT_3D ( 'NONE', #45424, #73866, #75266 ) ;
#56695 = CARTESIAN_POINT ( 'NONE',  ( 35.68263806977347485, -294.0137760869725980, -268.0299225310544671 ) ) ;
#56696 = EDGE_LOOP ( 'NONE', ( #13112, #88651, #32304, #3219 ) ) ;
#56697 = CARTESIAN_POINT ( 'NONE',  ( -108.5824064054046119, -289.4742857532162930, -252.2543676344083394 ) ) ;
#56698 = CARTESIAN_POINT ( 'NONE',  ( 4.800355109748853266, -275.2563093750758867, -205.9756310118413580 ) ) ;
#56699 = CARTESIAN_POINT ( 'NONE',  ( -68.28257698571616174, -273.6341103214037958, -204.2288740640422304 ) ) ;
#56700 = VERTEX_POINT ( 'NONE', #75375 ) ;
#56701 = LINE ( 'NONE', #33968, #82463 ) ;
#56702 = DIRECTION ( 'NONE',  ( 0.000000000000000000, 0.000000000000000000, -1.000000000000000000 ) ) ;
#56703 = DIRECTION ( 'NONE',  ( 0.000000000000000000, 0.000000000000000000, 1.000000000000000000 ) ) ;
#56704 = CARTESIAN_POINT ( 'NONE',  ( -41.08064305408498740, -281.0836649227019848, -197.1474144842652834 ) ) ;
#56705 = CARTESIAN_POINT ( 'NONE',  ( -97.78413017831341847, -280.9345627693524534, -224.2890008721304014 ) ) ;
#56706 = CARTESIAN_POINT ( 'NONE',  ( -106.3996038924070149, -283.2856876924329299, -294.8928170414952774 ) ) ;
#56707 = CARTESIAN_POINT ( 'NONE',  ( 35.77974035929660346, -283.2463849577728183, -257.5501686496451157 ) ) ;
#56708 = CARTESIAN_POINT ( 'NONE',  ( 33.53213756393575551, -273.7654484043518437, -249.9893292490428678 ) ) ;
#56709 = CARTESIAN_POINT ( 'NONE',  ( 17.06571399127465583, -89.54582641780471874, 21.50000000000000000 ) ) ;
#56710 = CARTESIAN_POINT ( 'NONE',  ( 201.2929949297285077, 65.04117685566218654, -7.250946725472672938 ) ) ;
#56711 = CARTESIAN_POINT ( 'NONE',  ( -101.9556507943157584, -278.8071245518754608, -312.0417934033824281 ) ) ;
#56712 = ORIENTED_EDGE ( 'NONE', *, *, #26148, .F. ) ;
#56713 = ORIENTED_EDGE ( 'NONE', *, *, #26684, .F. ) ;
#56714 = CARTESIAN_POINT ( 'NONE',  ( 222.4306832106270804, -147.4436952405746979, -22.50000000000000000 ) ) ;
#56715 = CARTESIAN_POINT ( 'NONE',  ( -49.79628808495661474, -285.1900151265476211, -344.7326805636440099 ) ) ;
#56716 = CARTESIAN_POINT ( 'NONE',  ( 21.12900100429709127, -292.1331741950734795, -226.3863657205809830 ) ) ;
#56717 = CARTESIAN_POINT ( 'NONE',  ( -12.26481900721097951, -288.0830187269731937, -343.1112238485928856 ) ) ;
#56718 = EDGE_CURVE ( 'NONE', #64817, #30244, #10488, .T. ) ;
#56719 = CARTESIAN_POINT ( 'NONE',  ( -97.38393068692143117, -283.3891947413420098, -227.0624381932072140 ) ) ;
#56721 = CARTESIAN_POINT ( 'NONE',  ( -81.02338749182996480, -287.8939974727422850, -330.1734152387459176 ) ) ;
#56720 = CARTESIAN_POINT ( 'NONE',  ( -97.04230389957892555, -283.7240095705122940, -227.3139050342514622 ) ) ;
#56722 = CARTESIAN_POINT ( 'NONE',  ( -26.66995869052062673, -284.1186018979579444, -343.0298064703055161 ) ) ;
#56723 = CARTESIAN_POINT ( 'NONE',  ( -16.31305462463360101, -272.3236647156698496, -198.3155668041703166 ) ) ;
#56724 = CARTESIAN_POINT ( 'NONE',  ( -113.0226960804680800, -283.0642294492725455, -261.4826459136350536 ) ) ;
#56725 = CARTESIAN_POINT ( 'NONE',  ( -107.5559382861217159, -298.2082499079031663, -296.8696270065109957 ) ) ;
#56726 = CARTESIAN_POINT ( 'NONE',  ( -107.3123243349159566, -282.9102301238597761, -242.7580784090494603 ) ) ;
#56727 = CARTESIAN_POINT ( 'NONE',  ( -107.4558385693462981, -279.7725523539320420, -249.2089067747869251 ) ) ;
#56728 = CARTESIAN_POINT ( 'NONE',  ( 18.89770494555045488, -288.8595077096412638, -220.4129036198637550 ) ) ;
#56729 = CARTESIAN_POINT ( 'NONE',  ( 219.7099725226080977, -147.7221692137691775, -1.978481845683818907 ) ) ;
#56730 = DIRECTION ( 'NONE',  ( -0.000000000000000000, -0.000000000000000000, -1.000000000000000000 ) ) ;
#56731 = CARTESIAN_POINT ( 'NONE',  ( 14.50864081789039162, -296.2495432193971965, -325.3234354361447913 ) ) ;
#56732 = CARTESIAN_POINT ( 'NONE',  ( -42.00572826972197049, -275.1107534575936029, -345.2289022584454301 ) ) ;
#56733 = CARTESIAN_POINT ( 'NONE',  ( -114.2286627002245893, -289.7385977494367921, -271.2167335908632140 ) ) ;
#56734 = CARTESIAN_POINT ( 'NONE',  ( 20.30603714499941859, -292.5960922907211739, -316.4592202991721024 ) ) ;
#56735 = CARTESIAN_POINT ( 'NONE',  ( -27.47570216592813352, -278.8647953589371582, -197.4816625090732884 ) ) ;
#56736 = CARTESIAN_POINT ( 'NONE',  ( -75.83114612811395716, -295.6724034417384814, -206.8237537036981166 ) ) ;
#56737 = CARTESIAN_POINT ( 'NONE',  ( -55.14793967977271905, -293.1334808871755513, -199.0576726967778711 ) ) ;
#56738 = CARTESIAN_POINT ( 'NONE',  ( 31.98288692825981272, -284.4805209788416391, -303.7098442033570223 ) ) ;
#56739 = CARTESIAN_POINT ( 'NONE',  ( -112.9123887431978233, -295.1666498957275167, -259.6942202617385647 ) ) ;
#56740 = CARTESIAN_POINT ( 'NONE',  ( 21.82696275339847602, -289.7646664163939931, -314.4902125429033504 ) ) ;
#56741 = CARTESIAN_POINT ( 'NONE',  ( -50.37028049401970975, -290.1278643719413708, -195.4997120031707993 ) ) ;
#56742 = VECTOR ( 'NONE', #43614, 1000.000000000000000 ) ;
#56743 = EDGE_CURVE ( 'NONE', #3669, #77618, #13798, .T. ) ;
#56744 = CARTESIAN_POINT ( 'NONE',  ( -109.0054099783330486, -292.1969947538240149, -253.5822444988266113 ) ) ;
#56745 = EDGE_CURVE ( 'NONE', #9610, #40624, #25863, .T. ) ;
#56746 = CARTESIAN_POINT ( 'NONE',  ( 151.2975037349265790, 130.0000000000000568, -12.50000000000000000 ) ) ;
#56747 = CARTESIAN_POINT ( 'NONE',  ( -91.80017830655891942, -292.0528026991282218, -221.4867128888363368 ) ) ;
#56748 = CARTESIAN_POINT ( 'NONE',  ( 128.9960186029002500, -299.5541904835127980, -195.3611179825600175 ) ) ;
#56749 = CARTESIAN_POINT ( 'NONE',  ( -112.5381414619063207, -291.9417703719585688, -255.6809424883213069 ) ) ;
#56751 = CARTESIAN_POINT ( 'NONE',  ( 31.80103605861241078, -293.2391603830303666, -246.7883386583480387 ) ) ;
#56750 = CARTESIAN_POINT ( 'NONE',  ( 30.55075662629251099, -279.1422954241611478, -237.5450997411538765 ) ) ;
#56752 = CARTESIAN_POINT ( 'NONE',  ( 39.71044205758624912, -281.5467637937352947, -269.9302679464767039 ) ) ;
#56753 = CARTESIAN_POINT ( 'NONE',  ( 34.56624224448843563, -281.5668343145136419, -297.8382378316797485 ) ) ;
#56754 =( GEOMETRIC_REPRESENTATION_CONTEXT ( 3 ) GLOBAL_UNCERTAINTY_ASSIGNED_CONTEXT ( ( #57980 ) ) GLOBAL_UNIT_ASSIGNED_CONTEXT ( ( #65421, #51626, #74343 ) ) REPRESENTATION_CONTEXT ( 'NONE', 'WORKASPACE' ) );
#56755 = CARTESIAN_POINT ( 'NONE',  ( 26.67062851513158250, -285.0279146717099934, -231.2788658862751561 ) ) ;
#56756 = CARTESIAN_POINT ( 'NONE',  ( 34.51323068508828129, -279.9344127122364512, -289.0593257110613763 ) ) ;
#56757 = CARTESIAN_POINT ( 'NONE',  ( -107.1571581817064782, -282.9102301224093026, -242.8192301167730420 ) ) ;
#56758 = LINE ( 'NONE', #20285, #74461 ) ;
#56759 = CARTESIAN_POINT ( 'NONE',  ( -25.48406923646075484, -278.6805263413885427, -194.9813836975748416 ) ) ;
#56760 = AXIS2_PLACEMENT_3D ( 'NONE', #14168, #5653, #85177 ) ;
#56761 = CARTESIAN_POINT ( 'NONE',  ( 14.04997972262696670, -285.6736460602409124, -213.3654549563043474 ) ) ;
#56762 = CARTESIAN_POINT ( 'NONE',  ( -19.24153929570557509, -275.0937682714692301, -199.4214417295161184 ) ) ;
#56763 = CARTESIAN_POINT ( 'NONE',  ( 195.6044778036177547, 41.09067717743725723, 14.48841315576171951 ) ) ;
#56764 = CARTESIAN_POINT ( 'NONE',  ( 36.42027776062617761, -295.1213789819406657, -267.9923564776565854 ) ) ;
#56765 = CARTESIAN_POINT ( 'NONE',  ( -10.57118739194255674, -275.8197702734472045, -198.7370626128347055 ) ) ;
#56766 = CARTESIAN_POINT ( 'NONE',  ( -39.16254299575933828, -276.7423474558363523, -343.3595564460371179 ) ) ;
#56767 = CARTESIAN_POINT ( 'NONE',  ( -107.2613205284957729, -291.1328495609135985, -237.9812195377652699 ) ) ;
#56768 = CARTESIAN_POINT ( 'NONE',  ( 36.72900442108796426, -279.8222554896709653, -285.2891094308296260 ) ) ;
#56769 = CARTESIAN_POINT ( 'NONE',  ( 29.47669420865653933, -292.8883005951869904, -232.0949164105482794 ) ) ;
#56770 = CARTESIAN_POINT ( 'NONE',  ( -52.40650087544421609, -290.9133393305313575, -198.6399494117271445 ) ) ;
#56771 = CARTESIAN_POINT ( 'NONE',  ( 31.56862506508735677, -291.9406376160899299, -300.0956789718887876 ) ) ;
#56772 = VERTEX_POINT ( 'NONE', #5174 ) ;
#56773 = DIRECTION ( 'NONE',  ( -1.000000000000000000, 0.000000000000000000, 0.000000000000000000 ) ) ;
#56774 = CARTESIAN_POINT ( 'NONE',  ( 29.91484724564734066, -292.6753985979214008, -241.6914185068661709 ) ) ;
#56775 = CARTESIAN_POINT ( 'NONE',  ( 158.6539576904058606, 276.0000000000000568, 11.60392986742922616 ) ) ;
#56776 = CARTESIAN_POINT ( 'NONE',  ( -92.05005921254146983, -276.6952119285918457, -226.6919474004047572 ) ) ;
#56777 = CARTESIAN_POINT ( 'NONE',  ( -109.6252612907722579, -295.9381362787688090, -244.5172212517033756 ) ) ;
#56778 = CARTESIAN_POINT ( 'NONE',  ( -103.6216568320890445, -286.3684757066138218, -232.0423045623604992 ) ) ;
#56779 = CARTESIAN_POINT ( 'NONE',  ( 17.77758282519474520, -286.7031433577826078, -222.4981401057240760 ) ) ;
#56780 = CARTESIAN_POINT ( 'NONE',  ( -24.18700188309069787, -278.4014013403927947, -342.9227942856481945 ) ) ;
#56781 = CARTESIAN_POINT ( 'NONE',  ( -111.4403711765601344, -294.4506259081986173, -279.7891289446308178 ) ) ;
#56782 = CARTESIAN_POINT ( 'NONE',  ( -110.8075262018316351, -298.1900563010285623, -279.7564097233081952 ) ) ;
#56783 = CARTESIAN_POINT ( 'NONE',  ( 35.09652309596444297, -274.5062457632989776, -282.4929824959415896 ) ) ;
#56784 = ORIENTED_EDGE ( 'NONE', *, *, #69037, .F. ) ;
#56785 = CARTESIAN_POINT ( 'NONE',  ( 194.4860589715128185, 40.74925082751673955, 14.32478396798074805 ) ) ;
#56786 = CARTESIAN_POINT ( 'NONE',  ( -77.07495303850760138, -295.2356076050358524, -336.3550143346614618 ) ) ;
#56787 = CARTESIAN_POINT ( 'NONE',  ( 30.75200374132935721, -289.8707168858433079, -300.5650338641434587 ) ) ;
#56788 = CARTESIAN_POINT ( 'NONE',  ( 202.9738562182569694, 295.9636489450776367, -54.00000000004089173 ) ) ;
#56789 = CARTESIAN_POINT ( 'NONE',  ( -63.85013099144709514, -290.0584419598487784, -338.5416980120431845 ) ) ;
#56790 = ORIENTED_EDGE ( 'NONE', *, *, #40534, .F. ) ;
#56791 = CARTESIAN_POINT ( 'NONE',  ( -8.936999191915294460, -279.4735078222589095, -199.0449684947067226 ) ) ;
#56792 = CARTESIAN_POINT ( 'NONE',  ( -103.7659439306353306, -297.7095486230705887, -231.5117085965722765 ) ) ;
#56793 = CARTESIAN_POINT ( 'NONE',  ( -111.7079305856647551, -288.8767743187848964, -255.8033243646799519 ) ) ;
#56794 = CARTESIAN_POINT ( 'NONE',  ( -98.25512482786351143, -296.2569967246311080, -317.4280807376011921 ) ) ;
#56795 = CARTESIAN_POINT ( 'NONE',  ( 12.37237532559006148, -294.6703387249092430, -323.9149846298220154 ) ) ;
#56796 = DIRECTION ( 'NONE',  ( 1.000000000000000000, 0.000000000000000000, 0.000000000000000000 ) ) ;
#56797 = CARTESIAN_POINT ( 'NONE',  ( 222.4306832106270804, -141.7221692137691775, 22.50000000000000000 ) ) ;
#56798 = CARTESIAN_POINT ( 'NONE',  ( 36.47863337052626775, -289.3163021980049052, -289.6812141656515109 ) ) ;
#56799 = CARTESIAN_POINT ( 'NONE',  ( -37.30987171927208834, -295.5523547857347353, -190.3611179825600175 ) ) ;
#56800 = ORIENTED_EDGE ( 'NONE', *, *, #27120, .T. ) ;
#56801 = CARTESIAN_POINT ( 'NONE',  ( 36.08085304393108572, -280.6132212610799002, -247.5041393481000398 ) ) ;
#56802 = CARTESIAN_POINT ( 'NONE',  ( -100.5666733072493173, -286.0114868529720411, -310.4909528210415033 ) ) ;
#56803 = CARTESIAN_POINT ( 'NONE',  ( -15.56388324074766594, -284.9031953737429035, -197.0645381205981437 ) ) ;
#56804 = CARTESIAN_POINT ( 'NONE',  ( -75.47415218002545600, -287.6447520726788980, -334.3075471078943224 ) ) ;
#56805 = CARTESIAN_POINT ( 'NONE',  ( 32.56456143457394603, -277.0334261622098211, -241.0123647036332102 ) ) ;
#56806 = ORIENTED_EDGE ( 'NONE', *, *, #51522, .F. ) ;
#56808 = CARTESIAN_POINT ( 'NONE',  ( 34.58425318030838014, -281.0736959019765777, -283.4906920588849175 ) ) ;
#56807 = CARTESIAN_POINT ( 'NONE',  ( -109.2860834537281107, -278.3880026119782656, -282.8045513793434225 ) ) ;
#56809 = CARTESIAN_POINT ( 'NONE',  ( 34.42762214996863435, -276.2884572016843094, -243.3304522691763054 ) ) ;
#56810 = CARTESIAN_POINT ( 'NONE',  ( -111.6967694131591742, -277.5793378866123362, -251.8863690268112805 ) ) ;
#56811 = CARTESIAN_POINT ( 'NONE',  ( 201.0615148111058375, 294.6280088066692997, -54.00000000000862599 ) ) ;
#56812 = CARTESIAN_POINT ( 'NONE',  ( -113.9471166701324023, -273.5649751209182909, -264.6557064416240337 ) ) ;
#56813 = EDGE_CURVE ( 'NONE', #9133, #2187, #48225, .T. ) ;
#56814 = CARTESIAN_POINT ( 'NONE',  ( 7.540083511923226567, -300.0289523866539412, -193.9397036489160087 ) ) ;
#56815 = CARTESIAN_POINT ( 'NONE',  ( -54.42813229853333468, -285.7662352645560873, -345.3683826091709648 ) ) ;
#56816 = ORIENTED_EDGE ( 'NONE', *, *, #45734, .F. ) ;
#56817 = CARTESIAN_POINT ( 'NONE',  ( 82.62398566199905758, -301.5110966808080093, -193.7954372207628069 ) ) ;
#56818 = CARTESIAN_POINT ( 'NONE',  ( 27.30953247925155836, -289.1022317698025290, -305.0299284288985291 ) ) ;
#56819 = CARTESIAN_POINT ( 'NONE',  ( -29.58890784089300752, -287.9091986229846611, -194.7709848651294919 ) ) ;
#56820 = CARTESIAN_POINT ( 'NONE',  ( 34.09738485971947597, -286.6965092121349699, -254.8578988116283597 ) ) ;
#56821 = CARTESIAN_POINT ( 'NONE',  ( -12.79777069895160935, -294.3712007776510973, -199.4370578810420795 ) ) ;
#56822 = CARTESIAN_POINT ( 'NONE',  ( -93.39100730602349643, -283.3396800105341526, -323.0871895847829478 ) ) ;
#56823 = CARTESIAN_POINT ( 'NONE',  ( -7.659186173002896503, -278.8476830580592036, -202.7796329416476055 ) ) ;
#56824 = CARTESIAN_POINT ( 'NONE',  ( -19.54225204922731152, -288.1439343479934792, -198.2913939261817404 ) ) ;
#56825 = CARTESIAN_POINT ( 'NONE',  ( 28.40866685983767326, -279.5830819510757692, -236.9673319692633129 ) ) ;
#56826 = CARTESIAN_POINT ( 'NONE',  ( -41.87035152653127312, -278.4255526404249963, -343.7272915648097182 ) ) ;
#56827 = CARTESIAN_POINT ( 'NONE',  ( -8.952702767496232283, -274.9259822828680626, -202.9866371157663707 ) ) ;
#56828 = CARTESIAN_POINT ( 'NONE',  ( -26.21745756478734179, -287.7084680293881433, -346.1520141715661225 ) ) ;
#56829 = AXIS2_PLACEMENT_3D ( 'NONE', #51876, #80303, #9246 ) ;
#56830 = CARTESIAN_POINT ( 'NONE',  ( -83.77746811494833423, -284.4739443136207910, -331.6478663621231817 ) ) ;
#56831 = CARTESIAN_POINT ( 'NONE',  ( -71.70562383742948498, -283.9864296807396045, -339.1989538783423654 ) ) ;
#56832 = CARTESIAN_POINT ( 'NONE',  ( 34.23110049439648606, -281.9091522222768731, -284.7883723717259841 ) ) ;
#56833 = ORIENTED_EDGE ( 'NONE', *, *, #68323, .T. ) ;
#56834 = ORIENTED_EDGE ( 'NONE', *, *, #1219, .F. ) ;
#56835 = FACE_OUTER_BOUND ( 'NONE', #25685, .T. ) ;
#56836 = CARTESIAN_POINT ( 'NONE',  ( 2.550249945180924627, -290.3842292782780419, -334.8349224950468397 ) ) ;
#56837 = CARTESIAN_POINT ( 'NONE',  ( -1.023102048212159998, -291.2087973157287593, -203.0242209119136305 ) ) ;
#56838 = CARTESIAN_POINT ( 'NONE',  ( -74.38207326934181651, -272.6056845373276474, -207.1246984394913682 ) ) ;
#56839 = CARTESIAN_POINT ( 'NONE',  ( 21.28455134861987474, -293.5724245778756654, -320.1233066875379336 ) ) ;
#56840 = CARTESIAN_POINT ( 'NONE',  ( -109.8646543130901279, -288.8610817458686029, -283.4427413478246081 ) ) ;
#56841 = CARTESIAN_POINT ( 'NONE',  ( 21.31273283856296885, -292.4188606709935812, -315.5219929201330729 ) ) ;
#56842 = CARTESIAN_POINT ( 'NONE',  ( 36.07712869506050879, -288.7300087896967966, -268.2860053273743688 ) ) ;
#56843 = CARTESIAN_POINT ( 'NONE',  ( 10.64812456238590066, -290.9090924074130839, -330.4860931364851808 ) ) ;
#56844 = CARTESIAN_POINT ( 'NONE',  ( -68.50249632939708988, -291.4617104047676435, -338.5954357219931694 ) ) ;
#56845 = CARTESIAN_POINT ( 'NONE',  ( -101.6342081159107948, -289.0738365943886947, -231.3185312610129927 ) ) ;
#56846 = CARTESIAN_POINT ( 'NONE',  ( -53.73033226344534086, -293.8421367365797323, -197.1210015038540178 ) ) ;
#56847 = CARTESIAN_POINT ( 'NONE',  ( -72.49746091384216129, -286.5159606300380233, -206.1013805704130846 ) ) ;
#56848 = CARTESIAN_POINT ( 'NONE',  ( 36.51891599923905574, -295.3735751992887799, -256.4098522915998046 ) ) ;
#56849 = CARTESIAN_POINT ( 'NONE',  ( -113.6885439307725818, -271.0584006130368380, -270.3420989471088660 ) ) ;
#56850 = DIRECTION ( 'NONE',  ( 0.000000000000000000, 1.000000000000000000, 0.000000000000000000 ) ) ;
#56851 = CARTESIAN_POINT ( 'NONE',  ( -70.69790813302894605, -275.5942986426687185, -202.7906348204811877 ) ) ;
#56852 = CARTESIAN_POINT ( 'NONE',  ( -15.57575551524399238, -280.7703005209700677, -342.1332873906470127 ) ) ;
#56853 = CARTESIAN_POINT ( 'NONE',  ( -111.8146800288023286, -295.5114887909660979, -289.3334102642808716 ) ) ;
#56854 = CARTESIAN_POINT ( 'NONE',  ( -49.01343685127250893, -272.1414185873658198, -197.2219963520723525 ) ) ;
#56855 = CARTESIAN_POINT ( 'NONE',  ( -106.8502854795440413, -276.9826370022785227, -243.5734670331097504 ) ) ;
#56856 = CARTESIAN_POINT ( 'NONE',  ( -51.65383020848835827, -275.0702021452863164, -198.3208966084563656 ) ) ;
#56857 = CARTESIAN_POINT ( 'NONE',  ( 25.66903081692104038, -273.5518117621004421, -227.1146142734469038 ) ) ;
#56858 = CARTESIAN_POINT ( 'NONE',  ( -96.06363718400488949, -297.3591076226111909, -314.7339728661498839 ) ) ;
#56859 = FACE_OUTER_BOUND ( 'NONE', #42056, .T. ) ;
#56860 = CARTESIAN_POINT ( 'NONE',  ( -108.7472414845238973, -297.1452719126152715, -286.2938010946481882 ) ) ;
#56861 = CARTESIAN_POINT ( 'NONE',  ( -112.3417001280820386, -272.5521521680024648, -270.3611179825637691 ) ) ;
#56863 = CARTESIAN_POINT ( 'NONE',  ( -109.5824463581982542, -272.5285553788712036, -259.5145635099089532 ) ) ;
#56862 = CARTESIAN_POINT ( 'NONE',  ( 22.56941999757815864, -284.9493879587978995, -224.6336679413746538 ) ) ;
#56864 = CARTESIAN_POINT ( 'NONE',  ( -20.98396659394967045, -286.2564902239945468, -195.1186794679401828 ) ) ;
#56865 = CARTESIAN_POINT ( 'NONE',  ( 20.55419534580220287, -287.9056177152211831, -321.1137015996543482 ) ) ;
#56866 = CARTESIAN_POINT ( 'NONE',  ( -90.49361667431075773, -299.2837399151713385, -216.9450102151081410 ) ) ;
#56867 = CARTESIAN_POINT ( 'NONE',  ( 19.34493790852515360, -292.2309370920916081, -319.2340354594890073 ) ) ;
#56868 = CARTESIAN_POINT ( 'NONE',  ( -68.59745950965171346, -278.8489373814357464, -200.1524878548045763 ) ) ;
#56869 = CARTESIAN_POINT ( 'NONE',  ( -54.42813229853332757, -289.3380690714490129, -195.3538533559490702 ) ) ;
#56870 = FACE_OUTER_BOUND ( 'NONE', #89596, .T. ) ;
#56871 = CARTESIAN_POINT ( 'NONE',  ( 8.214463808611272455, -287.2076671594689969, -327.9090669553941666 ) ) ;
#56872 = ADVANCED_FACE ( 'NONE', ( #20773 ), #9233, .T. ) ;
#56873 = CARTESIAN_POINT ( 'NONE',  ( 197.9854405158082784, 69.89761265382871613, -11.10143562203536582 ) ) ;
#56874 = CARTESIAN_POINT ( 'NONE',  ( -15.28719573718626457, -286.7665914097424888, -342.0994090541371406 ) ) ;
#56875 = CARTESIAN_POINT ( 'NONE',  ( -94.32674145552130085, -274.7281231926065743, -223.6143778571423013 ) ) ;
#56876 = CARTESIAN_POINT ( 'NONE',  ( 8.180831956586883891, -282.0860793272931915, -208.9251251742019235 ) ) ;
#56878 = CARTESIAN_POINT ( 'NONE',  ( 22.58477221173992078, -282.1331888100040146, -312.0482612392601709 ) ) ;
#56877 = CARTESIAN_POINT ( 'NONE',  ( -78.59798690511595964, -293.6248854651838656, -333.4192308821029087 ) ) ;
#56879 = CARTESIAN_POINT ( 'NONE',  ( -99.92278962374336970, -297.3133179158986081, -225.4990266129764507 ) ) ;
#56880 = CARTESIAN_POINT ( 'NONE',  ( -99.79002154730132190, -274.5104264878792719, -231.4306406096073658 ) ) ;
#56881 = EDGE_CURVE ( 'NONE', #3669, #50859, #19829, .T. ) ;
#56882 = CARTESIAN_POINT ( 'NONE',  ( 36.81324051993287583, -283.4038447052250262, -258.7980346704216572 ) ) ;
#56883 = CARTESIAN_POINT ( 'NONE',  ( -109.0069000545257438, -295.8100095338479605, -255.2175149702159445 ) ) ;
#56884 = ORIENTED_EDGE ( 'NONE', *, *, #13868, .F. ) ;
#56885 = DIRECTION ( 'NONE',  ( -0.8660254037844410391, 0.000000000000000000, -0.4999999999999960032 ) ) ;
#56886 = CARTESIAN_POINT ( 'NONE',  ( 21.49261924077924135, -284.1652513568672589, -316.2998779917808747 ) ) ;
#56887 = DIRECTION ( 'NONE',  ( 0.9951408606192334583, 1.205805641958521361E-17, 0.09846150276129006507 ) ) ;
#56888 = CARTESIAN_POINT ( 'NONE',  ( 31.95455697924147032, -285.4809262143061801, -303.7686719486574702 ) ) ;
#56889 = CARTESIAN_POINT ( 'NONE',  ( -1.552024450238887354, -275.7870919687083529, -338.3556614091436359 ) ) ;
#56890 = CARTESIAN_POINT ( 'NONE',  ( 6.677930937926969790, -292.5033594675655308, -212.1264883770056713 ) ) ;
#56891 = CARTESIAN_POINT ( 'NONE',  ( 21.05357421902077419, -282.4453198092525668, -225.3884229207988312 ) ) ;
#56892 = AXIS2_PLACEMENT_3D ( 'NONE', #24492, #90726, #25886 ) ;
#56893 = CARTESIAN_POINT ( 'NONE',  ( 35.50010056705049521, -277.3109969259734839, -282.5242107043105761 ) ) ;
#56894 = CARTESIAN_POINT ( 'NONE',  ( -111.9458314826517409, -285.7692499673535735, -286.8786807654246331 ) ) ;
#56895 = CARTESIAN_POINT ( 'NONE',  ( 34.87338347557749074, -280.5201228497765555, -283.5506168502577111 ) ) ;
#56896 = CARTESIAN_POINT ( 'NONE',  ( -96.84463670779649647, -279.9270754050482992, -316.0163607360962601 ) ) ;
#56897 = CARTESIAN_POINT ( 'NONE',  ( -37.25358771661635160, -298.0532286319332798, -193.3603543084721821 ) ) ;
#56898 = CARTESIAN_POINT ( 'NONE',  ( 38.18195486687699258, -275.5731426814587621, -285.3670348398762258 ) ) ;
#56899 = CARTESIAN_POINT ( 'NONE',  ( 29.70191190629370581, -295.9030012171571116, -302.8292357805218558 ) ) ;
#56900 = DIRECTION ( 'NONE',  ( -0.000000000000000000, -1.000000000000000000, -0.000000000000000000 ) ) ;
#56901 = CARTESIAN_POINT ( 'NONE',  ( 157.7238125175282732, 19.47471017779398750, 10.32097897594415059 ) ) ;
#56902 = CARTESIAN_POINT ( 'NONE',  ( -107.2447219181401294, -294.3124804704074791, -299.7181098438056210 ) ) ;
#56903 = CARTESIAN_POINT ( 'NONE',  ( 30.23412476943069649, -274.6862616529999741, -242.4524217175309957 ) ) ;
#56904 = CARTESIAN_POINT ( 'NONE',  ( 37.11174518959666813, -295.2839562669528277, -287.1351906181812410 ) ) ;
#56905 = CARTESIAN_POINT ( 'NONE',  ( 35.11586680115529902, -295.0739691744238371, -295.3815541510010121 ) ) ;
#56906 = CARTESIAN_POINT ( 'NONE',  ( 34.07063134419961870, -289.8434941292947542, -292.9013247801119064 ) ) ;
#56907 = CARTESIAN_POINT ( 'NONE',  ( -51.65590036480032410, -275.2355271501059519, -343.8126809006914755 ) ) ;
#56908 = CARTESIAN_POINT ( 'NONE',  ( 1.646058413034991785, -278.4470922088816565, -333.8351728074196103 ) ) ;
#56909 = CARTESIAN_POINT ( 'NONE',  ( -37.01327804955438694, -293.1278232743370040, -344.8130663223228680 ) ) ;
#56910 = CARTESIAN_POINT ( 'NONE',  ( 32.43771646870996506, -283.7958510998655015, -300.0102549838469486 ) ) ;
#56911 = CARTESIAN_POINT ( 'NONE',  ( -102.5069106769047096, -283.9270790817337229, -236.7795544871026721 ) ) ;
#56912 = CARTESIAN_POINT ( 'NONE',  ( 123.5159050921753732, 147.8964653910322227, -262.5416932347842476 ) ) ;
#56913 = CARTESIAN_POINT ( 'NONE',  ( -69.98807517729166250, -285.2765890292004087, -205.0302375404852171 ) ) ;
#56914 = ORIENTED_EDGE ( 'NONE', *, *, #82272, .T. ) ;
#56915 = CARTESIAN_POINT ( 'NONE',  ( 27.58231245809937704, -282.0940213766514262, -229.4404881202036393 ) ) ;
#56916 = CARTESIAN_POINT ( 'NONE',  ( -112.1407119049886489, -283.1393277365581298, -286.8873564434757100 ) ) ;
#56917 = CARTESIAN_POINT ( 'NONE',  ( -92.91172984244634847, -280.2203447056240293, -217.3248688841182457 ) ) ;
#56918 =( NAMED_UNIT ( * ) PLANE_ANGLE_UNIT ( ) SI_UNIT ( $, .RADIAN. ) );
#56919 = CARTESIAN_POINT ( 'NONE',  ( -104.3573546980911573, -279.5957396292412227, -306.8523469782555821 ) ) ;
#56920 = CARTESIAN_POINT ( 'NONE',  ( -92.08974858914540107, -275.4094976428775681, -313.9805196606274080 ) ) ;
#56921 = CARTESIAN_POINT ( 'NONE',  ( -111.8162934558724686, -271.8246563314528430, -296.4050190923600212 ) ) ;
#56922 = VERTEX_POINT ( 'NONE', #35912 ) ;
#56923 = CARTESIAN_POINT ( 'NONE',  ( 54.71294253227434012, -301.2046906602610647, -195.3297278719368251 ) ) ;
#56924 = CARTESIAN_POINT ( 'NONE',  ( 197.0526034356285834, 285.3763918474514867, -111.7597976793902745 ) ) ;
#56925 = CARTESIAN_POINT ( 'NONE',  ( -21.82849779101435672, -278.2718982304160704, -197.2931086138896433 ) ) ;
#56926 = CARTESIAN_POINT ( 'NONE',  ( -100.8495406482632006, -292.8691193047577030, -228.5446216049518000 ) ) ;
#56927 = CARTESIAN_POINT ( 'NONE',  ( 23.43059176747042116, -292.3373188057852872, -229.7332801619119493 ) ) ;
#56928 = CARTESIAN_POINT ( 'NONE',  ( -43.18388136776747643, -288.6317150851102156, -347.0774514559837485 ) ) ;
#56929 = CARTESIAN_POINT ( 'NONE',  ( 165.0427047786672290, 249.5000000000000568, 23.37680765314704701 ) ) ;
#56930 = EDGE_CURVE ( 'NONE', #24992, #49098, #48696, .T. ) ;
#56932 = CARTESIAN_POINT ( 'NONE',  ( -37.25974681457593363, -284.4530287867748370, -196.5485861912586927 ) ) ;
#56931 = CARTESIAN_POINT ( 'NONE',  ( 20.90661756809265626, -292.7986906188394300, -319.8155392203443625 ) ) ;
#56933 = CARTESIAN_POINT ( 'NONE',  ( -86.76881564727500518, -293.2169640281572924, -214.9039522005589333 ) ) ;
#56934 = CARTESIAN_POINT ( 'NONE',  ( 32.70642831699704800, -283.1621450715470019, -292.7644115030059879 ) ) ;
#56935 = ORIENTED_EDGE ( 'NONE', *, *, #49001, .T. ) ;
#56936 = CARTESIAN_POINT ( 'NONE',  ( -112.0909025917204787, -291.7126243299221073, -252.8860802084473391 ) ) ;
#56937 = CARTESIAN_POINT ( 'NONE',  ( -1.941747386683363219, -281.0269234322302623, -206.4484291980828345 ) ) ;
#56938 = CARTESIAN_POINT ( 'NONE',  ( 34.07573131882021755, -292.6999002978242288, -298.0659768212267977 ) ) ;
#56939 = CARTESIAN_POINT ( 'NONE',  ( 37.34987216221739459, -288.5816919551905926, -288.4535802332993626 ) ) ;
#56940 = CARTESIAN_POINT ( 'NONE',  ( -70.60678316172038649, -289.9713676323442542, -339.7511000828700958 ) ) ;
#56941 = CARTESIAN_POINT ( 'NONE',  ( 31.40011387464588211, -288.0459424448731056, -294.9286374363081791 ) ) ;
#56942 = EDGE_LOOP ( 'NONE', ( #31645, #993, #40768, #57917 ) ) ;
#56943 = CARTESIAN_POINT ( 'NONE',  ( 199.0061125298537377, 215.0000000000000568, -7.725424859374024678 ) ) ;
#56944 = CARTESIAN_POINT ( 'NONE',  ( -11.45658210774083230, -296.5790722088510165, -341.6225882980729693 ) ) ;
#56945 = CARTESIAN_POINT ( 'NONE',  ( -91.27593461744098136, -295.9892048044292778, -216.0988233189382868 ) ) ;
#56946 = CARTESIAN_POINT ( 'NONE',  ( -87.26465425291733879, -276.8276912394720171, -323.9438306713270208 ) ) ;
#56947 = CARTESIAN_POINT ( 'NONE',  ( -99.51361648575650065, -272.6628428023130937, -224.9497257201346940 ) ) ;
#56948 = CARTESIAN_POINT ( 'NONE',  ( -93.62433890005128490, -294.3621618978256151, -317.9513820634163039 ) ) ;
#56949 = CARTESIAN_POINT ( 'NONE',  ( 20.83266759778180699, -277.9490847756807739, -316.1386876423610488 ) ) ;
#56950 = CARTESIAN_POINT ( 'NONE',  ( -50.10696186630607940, -296.1268671890846917, -197.4569198592163275 ) ) ;
#56951 = CARTESIAN_POINT ( 'NONE',  ( 35.82146021440599526, -294.8340551310141677, -276.2162416171337895 ) ) ;
#56952 = CARTESIAN_POINT ( 'NONE',  ( -94.17349107486099058, -296.9788784132343267, -316.6882248832757227 ) ) ;
#56953 = DIRECTION ( 'NONE',  ( -1.110223024625156383E-14, 0.000000000000000000, 1.000000000000000000 ) ) ;
#56954 = CARTESIAN_POINT ( 'NONE',  ( -112.5044686842429371, -294.5618006923252210, -269.5951895088238643 ) ) ;
#56955 = CARTESIAN_POINT ( 'NONE',  ( -36.55026780097767869, -298.7132266003461609, -193.4629651673951400 ) ) ;
#56956 = CARTESIAN_POINT ( 'NONE',  ( -64.05155414336680053, -287.9820915129198511, -338.9865755659113233 ) ) ;
#56957 = CARTESIAN_POINT ( 'NONE',  ( -77.66027734927040171, -275.5109923772375851, -207.1202057633774416 ) ) ;
#56958 = CARTESIAN_POINT ( 'NONE',  ( -68.82462314344466847, -274.1416028730830590, -200.1445082283984505 ) ) ;
#56959 = CARTESIAN_POINT ( 'NONE',  ( -95.30844261486753055, -297.5101944152214628, -225.9341639076047272 ) ) ;
#56960 = CARTESIAN_POINT ( 'NONE',  ( -70.53332434206403434, -281.5965882558043063, -202.7096369237689828 ) ) ;
#56961 = CARTESIAN_POINT ( 'NONE',  ( 31.93866299124532304, -280.6566962819538276, -302.9439941192916308 ) ) ;
#56962 = EDGE_LOOP ( 'NONE', ( #70327, #35935, #42418, #4009 ) ) ;
#56963 = CARTESIAN_POINT ( 'NONE',  ( 6.859627982674678215, -281.8169376483469364, -333.3512253923741468 ) ) ;
#56964 = CARTESIAN_POINT ( 'NONE',  ( 33.62268972732272942, -274.5220013279320028, -240.6031520531212777 ) ) ;
#56965 = CARTESIAN_POINT ( 'NONE',  ( -1.493590280205330689, -278.9192612726224070, -203.1201078980975581 ) ) ;
#56966 = CARTESIAN_POINT ( 'NONE',  ( -96.24399245295794003, -277.1921505458130923, -223.6647756166170495 ) ) ;
#56967 = CARTESIAN_POINT ( 'NONE',  ( -5.033110370024855840, -273.0607859142414782, -204.2296337750664748 ) ) ;
#56968 = CARTESIAN_POINT ( 'NONE',  ( -37.67496901067786297, -276.0481711635446800, -195.3492686136225700 ) ) ;
#56969 = CARTESIAN_POINT ( 'NONE',  ( 189.9243309297870610, 250.5000000000000568, 20.22542485937349355 ) ) ;
#56970 = CARTESIAN_POINT ( 'NONE',  ( 153.7618860799040590, 19.60619416575235263, 12.81536571218043719 ) ) ;
#56971 = CARTESIAN_POINT ( 'NONE',  ( 34.72157659004641772, -291.2896214802218537, -248.3317977032069450 ) ) ;
#56972 = CARTESIAN_POINT ( 'NONE',  ( -30.69726913359199116, -292.1338189861018009, -193.5955736811883128 ) ) ;
#56973 = CARTESIAN_POINT ( 'NONE',  ( -17.80916112088869951, -278.8009893514287114, -342.9456090505674410 ) ) ;
#56974 = CARTESIAN_POINT ( 'NONE',  ( -0.7245070546902723230, -272.5383256351898922, -204.8927484250020541 ) ) ;
#56975 = CARTESIAN_POINT ( 'NONE',  ( 169.2744399300530347, -11.64849832608277325, 13.00000000000000178 ) ) ;
#56976 = CYLINDRICAL_SURFACE ( 'NONE', #42631, 8.000000000000000000 ) ;
#56977 = CARTESIAN_POINT ( 'NONE',  ( -70.69899523382866846, -283.6121493955225219, -203.1734501447768650 ) ) ;
#56978 = CARTESIAN_POINT ( 'NONE',  ( 199.0743954165634761, 275.0000000000000568, -2.725891136377211144 ) ) ;
#56979 = CARTESIAN_POINT ( 'NONE',  ( 10.53901234483598337, -293.1681233877403088, -325.9899583156043832 ) ) ;
#56980 = CARTESIAN_POINT ( 'NONE',  ( 36.86361269976527666, -285.7368702992679346, -273.8409634762059568 ) ) ;
#56981 = DIRECTION ( 'NONE',  ( -0.000000000000000000, -1.000000000000000000, -0.000000000000000000 ) ) ;
#56982 = CARTESIAN_POINT ( 'NONE',  ( 157.4851178187871312, 15.28877977928703658, -6.999999999998999023 ) ) ;
#56983 = CARTESIAN_POINT ( 'NONE',  ( -3.455197931748154261, -292.6047140793157268, -337.2836856663037111 ) ) ;
#56984 = CARTESIAN_POINT ( 'NONE',  ( -85.67825976110560759, -282.1872209888519478, -329.4058870458297292 ) ) ;
#56985 = CARTESIAN_POINT ( 'NONE',  ( -101.5174171983701967, -280.6459334508145389, -233.9205121687215865 ) ) ;
#56986 = CARTESIAN_POINT ( 'NONE',  ( -87.50158432319115320, -286.5757132716646538, -212.3944682455413897 ) ) ;
#56987 = CARTESIAN_POINT ( 'NONE',  ( 19.38730561538277897, -279.0973403998557387, -219.7866858338066720 ) ) ;
#56988 = CARTESIAN_POINT ( 'NONE',  ( 33.70108727723620490, -287.7736599881156963, -287.1516616808103777 ) ) ;
#56989 = CARTESIAN_POINT ( 'NONE',  ( -105.8094356715702560, -279.6195923458071206, -297.3341434989458776 ) ) ;
#56990 = CARTESIAN_POINT ( 'NONE',  ( -96.54237104610450615, -279.9552479132331086, -227.3741165733673029 ) ) ;
#56991 = CARTESIAN_POINT ( 'NONE',  ( 13.12619323610478261, -288.7327171141691906, -214.3322335487033854 ) ) ;
#56992 = EDGE_LOOP ( 'NONE', ( #53705, #24618, #58615, #44639, #82212, #22888, #72806, #51742, #10981, #48988, #77880, #88615, #1003, #53828, #73104, #23911, #1131, #36634, #78129 ) ) ;
#56993 = CARTESIAN_POINT ( 'NONE',  ( -85.21476000888939950, -297.2447833527709804, -210.0521622451851442 ) ) ;
#56994 = CARTESIAN_POINT ( 'NONE',  ( -37.24104840482309697, -291.0307759980611308, -345.0058544116742496 ) ) ;
#56995 = CARTESIAN_POINT ( 'NONE',  ( 175.2296996224749250, 275.0000000000000568, -29.99999999999998224 ) ) ;
#56996 = CARTESIAN_POINT ( 'NONE',  ( -111.2586520408596868, -286.6233781216988064, -305.9938812882205070 ) ) ;
#56997 = ORIENTED_EDGE ( 'NONE', *, *, #10314, .T. ) ;
#56998 = CARTESIAN_POINT ( 'NONE',  ( -35.54153654152194264, -272.0745038759882277, -195.2031888215580580 ) ) ;
#56999 = ORIENTED_EDGE ( 'NONE', *, *, #56718, .F. ) ;
#57000 = CARTESIAN_POINT ( 'NONE',  ( 34.72310501556402329, -292.2692172039432421, -295.2836283584013017 ) ) ;
#57001 = CARTESIAN_POINT ( 'NONE',  ( -110.4356889987182768, -296.0813631412486870, -268.7252675560291095 ) ) ;
#57002 = CARTESIAN_POINT ( 'NONE',  ( -33.21904697282409558, -287.6249900601071090, -196.7328961683710133 ) ) ;
#57003 = CARTESIAN_POINT ( 'NONE',  ( 36.03439874259679954, -283.1812574738265766, -260.2895952477425112 ) ) ;
#57004 = CARTESIAN_POINT ( 'NONE',  ( -75.35467898774608386, -290.9739855493204459, -336.6455032572121127 ) ) ;
#57005 = CARTESIAN_POINT ( 'NONE',  ( -75.40371254366711185, -290.8639050383438871, -336.7281390379810091 ) ) ;
#57006 = CARTESIAN_POINT ( 'NONE',  ( -103.5244373229910479, -286.0830144231047711, -305.7539570117792778 ) ) ;
#57007 = CARTESIAN_POINT ( 'NONE',  ( -56.92197987009077309, -277.4644614284491126, -344.8850404908887981 ) ) ;
#57008 = CIRCLE ( 'NONE', #67593, 5.568361562975243650 ) ;
#57009 = CARTESIAN_POINT ( 'NONE',  ( 10.27159629921781026, -292.4814568221828495, -329.0995434034642244 ) ) ;
#57010 = CARTESIAN_POINT ( 'NONE',  ( -6.228421261166688261, -280.2830642313593899, -199.9127353148523412 ) ) ;
#57011 = CARTESIAN_POINT ( 'NONE',  ( -110.3487966584650053, -274.5905835462723985, -256.6384011743670044 ) ) ;
#57012 = CARTESIAN_POINT ( 'NONE',  ( 31.95455697924148097, -295.6233781216988632, -236.9535640164627637 ) ) ;
#57013 = CARTESIAN_POINT ( 'NONE',  ( 2.944996183118116395, -274.7595557134114870, -334.8509593743912092 ) ) ;
#57014 = LINE ( 'NONE', #85850, #81760 ) ;
#57015 = CARTESIAN_POINT ( 'NONE',  ( 35.62706769095613879, -281.1083151865499303, -274.0417924396392095 ) ) ;
#57016 = CARTESIAN_POINT ( 'NONE',  ( -113.9873588511679969, -279.7414350433387540, -271.6172805357961124 ) ) ;
#57017 = CARTESIAN_POINT ( 'NONE',  ( -75.53183120188381849, -298.9575618885363610, -207.3982246520323827 ) ) ;
#57018 = CARTESIAN_POINT ( 'NONE',  ( -78.38650515326199297, -284.5728664480191696, -205.4909076155248613 ) ) ;
#57019 = CARTESIAN_POINT ( 'NONE',  ( -110.2792174653791335, -292.4797049607450390, -257.4945063852299540 ) ) ;
#57020 = CARTESIAN_POINT ( 'NONE',  ( -64.63279250055867919, -275.3018531292676130, -199.2018976324963546 ) ) ;
#57021 = CARTESIAN_POINT ( 'NONE',  ( -41.18486414913537885, -275.3200356171304861, -193.8989300784495526 ) ) ;
#57022 = LINE ( 'NONE', #34750, #21359 ) ;
#57023 = CARTESIAN_POINT ( 'NONE',  ( -25.90265132006070559, -296.9062861093387937, -344.3149994667273859 ) ) ;
#57024 = CARTESIAN_POINT ( 'NONE',  ( -68.57212797090788570, -281.4633582659103013, -338.3661825511899224 ) ) ;
#57025 = CARTESIAN_POINT ( 'NONE',  ( -111.6112754635759075, -290.4730434448304095, -250.0682234348522854 ) ) ;
#57026 = CARTESIAN_POINT ( 'NONE',  ( 26.77580129805163267, -274.0861768400902747, -308.5814373393323535 ) ) ;
#57027 = CARTESIAN_POINT ( 'NONE',  ( 22.35232823133723912, -288.5115964331699274, -222.9793381090060791 ) ) ;
#57028 = CARTESIAN_POINT ( 'NONE',  ( -90.97599986096025759, -290.1882495241550828, -220.3666878367873210 ) ) ;
#57029 = VERTEX_POINT ( 'NONE', #21235 ) ;
#57030 = CARTESIAN_POINT ( 'NONE',  ( -112.7812274638141048, -288.9738315548914898, -282.5054174105057427 ) ) ;
#57031 = CARTESIAN_POINT ( 'NONE',  ( -77.26316839752735177, -291.1671353052126960, -209.2189569319506575 ) ) ;
#57032 = EDGE_LOOP ( 'NONE', ( #56999, #3174, #73074, #33121, #68763, #85187 ) ) ;
#57033 = CARTESIAN_POINT ( 'NONE',  ( 26.09391856048089053, -288.0610159307652225, -227.2399295133388648 ) ) ;
#57034 = CARTESIAN_POINT ( 'NONE',  ( 13.74915395457545664, -276.6453514654967307, -322.6025318019650854 ) ) ;
#57035 = CARTESIAN_POINT ( 'NONE',  ( -22.17218938640405312, -293.7825439556069114, -345.5367686465120869 ) ) ;
#57036 = CARTESIAN_POINT ( 'NONE',  ( -71.68576130064883500, -284.1454699585555659, -339.1637214888811513 ) ) ;
#57037 = CARTESIAN_POINT ( 'NONE',  ( -69.78779512738151425, -285.9698201995951194, -200.5399141243469217 ) ) ;
#57038 = CARTESIAN_POINT ( 'NONE',  ( -58.95034025699933267, -283.6727034005659220, -340.1649311593427569 ) ) ;
#57039 = CARTESIAN_POINT ( 'NONE',  ( -22.29584452022010410, -108.1748762211270076, -362.7363045332584193 ) ) ;
#57040 = CARTESIAN_POINT ( 'NONE',  ( -32.08198064645461756, -123.8691969543307891, -363.6799844872283529 ) ) ;
#57041 = CARTESIAN_POINT ( 'NONE',  ( 24.66845159430726753, -23.60273429576747972, -341.5102311320878812 ) ) ;
#57042 = CARTESIAN_POINT ( 'NONE',  ( -31.31624232178432266, -273.3273285971770292, -197.4355088390831554 ) ) ;
#57043 = CARTESIAN_POINT ( 'NONE',  ( -38.07170090988125821, -272.9631189479677005, -197.0556395139649055 ) ) ;
#57044 = CARTESIAN_POINT ( 'NONE',  ( -107.1132046348760412, -295.6444724115103213, -302.7874045709687039 ) ) ;
#57045 = CARTESIAN_POINT ( 'NONE',  ( -101.4239464694510815, -254.8757987455171303, -324.3748491368189093 ) ) ;
#57046 = ADVANCED_FACE ( 'NONE', ( #57242 ), #91785, .F. ) ;
#57047 = CARTESIAN_POINT ( 'NONE',  ( -76.16792024306317899, -272.2298729070964214, -204.3770549805997803 ) ) ;
#57048 = CARTESIAN_POINT ( 'NONE',  ( -93.69731465116937841, -299.0891298078469731, -222.0206491791082613 ) ) ;
#57049 = EDGE_CURVE ( 'NONE', #61449, #45666, #77320, .T. ) ;
#57050 = CARTESIAN_POINT ( 'NONE',  ( 3.905138949092443301, -289.7993641071265074, -331.2496380871870088 ) ) ;
#57051 = CARTESIAN_POINT ( 'NONE',  ( -108.7316297353748240, -291.8514498473621757, -253.6418770121819364 ) ) ;
#57052 = EDGE_LOOP ( 'NONE', ( #16654, #44899, #26873, #65424 ) ) ;
#57053 = CARTESIAN_POINT ( 'NONE',  ( -82.84078776837078806, -298.3883985450590330, -208.4674559683344910 ) ) ;
#57054 = CARTESIAN_POINT ( 'NONE',  ( 27.08768995313700856, -288.5150020839810736, -304.9193862970209352 ) ) ;
#57055 = CARTESIAN_POINT ( 'NONE',  ( 6.530208131676044303, -295.2756834791700271, -333.5085562059158519 ) ) ;
#57056 = CARTESIAN_POINT ( 'NONE',  ( -81.83100278750610812, -296.1323502263370528, -333.1974273120356429 ) ) ;
#57057 = CARTESIAN_POINT ( 'NONE',  ( 34.21606884034724771, -293.5283579228146777, -255.9220839154837108 ) ) ;
#57058 = ORIENTED_EDGE ( 'NONE', *, *, #18534, .T. ) ;
#57059 = CARTESIAN_POINT ( 'NONE',  ( 37.88121963091056443, -277.3746875442321311, -262.7015421438641738 ) ) ;
#57060 = EDGE_LOOP ( 'NONE', ( #4846, #35829, #83193, #204 ) ) ;
#57061 = CARTESIAN_POINT ( 'NONE',  ( -68.64174411570809298, -279.1593725660400196, -200.0627906718582381 ) ) ;
#57062 = CARTESIAN_POINT ( 'NONE',  ( 35.93446212157289210, -276.5093973065011710, -271.5769497896921507 ) ) ;
#57063 = CARTESIAN_POINT ( 'NONE',  ( -46.77767594461364098, -275.6940480370619184, -194.9626009363000207 ) ) ;
#57064 = CARTESIAN_POINT ( 'NONE',  ( 37.68233627622525006, -273.4752696502167169, -262.7716176065841296 ) ) ;
#57065 = CARTESIAN_POINT ( 'NONE',  ( -34.48323562599132686, -298.7402805562511503, -197.2588576385242050 ) ) ;
#57066 = CARTESIAN_POINT ( 'NONE',  ( -73.60847255458759264, -294.1183427976135363, -334.3931110439744430 ) ) ;
#57067 = DIRECTION ( 'NONE',  ( 0.000000000000000000, 1.000000000000000000, 0.000000000000000000 ) ) ;
#57068 = CARTESIAN_POINT ( 'NONE',  ( -112.9368912412941341, -279.2245402869689315, -255.9765108116061185 ) ) ;
#57069 = CARTESIAN_POINT ( 'NONE',  ( -1.468378563068700071, -276.7293780571827710, -333.9958696484717393 ) ) ;
#57070 = CARTESIAN_POINT ( 'NONE',  ( 24.31583636898643874, -285.6314728445236142, -225.0660137560103067 ) ) ;
#57071 = CARTESIAN_POINT ( 'NONE',  ( -4.439390663982942797, -300.4632727336159519, -195.1832562283304071 ) ) ;
#57072 = LINE ( 'NONE', #28640, #26348 ) ;
#57073 = CARTESIAN_POINT ( 'NONE',  ( 19.64740117131388786, -286.1019006774488957, -224.4626861561665976 ) ) ;
#57074 = CARTESIAN_POINT ( 'NONE',  ( -36.98120204125686428, -278.2965856733780470, -196.3486591815759255 ) ) ;
#57075 = CARTESIAN_POINT ( 'NONE',  ( -110.5503501736334044, -277.2310611430731910, -262.3993772893183518 ) ) ;
#57076 = CARTESIAN_POINT ( 'NONE',  ( -39.26865653978450865, -285.0764670791407411, -345.3489154689093539 ) ) ;
#57077 = CARTESIAN_POINT ( 'NONE',  ( -9.825337146746806027, -277.8896722950271965, -338.4187172147080673 ) ) ;
#57078 = DIRECTION ( 'NONE',  ( 0.000000000000000000, 0.000000000000000000, 1.000000000000000000 ) ) ;
#57079 = CARTESIAN_POINT ( 'NONE',  ( -7.000189698666798854, -274.8993490968689457, -340.0412934062130716 ) ) ;
#57080 = CARTESIAN_POINT ( 'NONE',  ( -46.19934488342533996, -274.5882315184521758, -197.7978021994498192 ) ) ;
#57081 = CARTESIAN_POINT ( 'NONE',  ( 37.70065986253945312, -283.6182716926127227, -275.5093361847587516 ) ) ;
#57082 = CARTESIAN_POINT ( 'NONE',  ( 222.4306832106270804, -142.7221692137691775, 21.50000000000000000 ) ) ;
#57083 = CARTESIAN_POINT ( 'NONE',  ( -6.197271525055271901, -290.5662769388397351, -339.2039735899903121 ) ) ;
#57084 = CARTESIAN_POINT ( 'NONE',  ( 34.38626963407741499, -291.2690379094027548, -248.4064131804255737 ) ) ;
#57085 = CARTESIAN_POINT ( 'NONE',  ( 208.6208076322478746, 32.98517505407394168, 15.00000000000000000 ) ) ;
#57086 = CARTESIAN_POINT ( 'NONE',  ( -46.22187263709554372, -272.6219611984311086, -197.4064333237768381 ) ) ;
#57087 = CARTESIAN_POINT ( 'NONE',  ( 11.76535650949521994, -290.8818022956375557, -214.6205859784895154 ) ) ;
#57088 = CARTESIAN_POINT ( 'NONE',  ( -68.16629546550866792, -198.4621125041185792, -363.1570911012638021 ) ) ;
#57089 = CARTESIAN_POINT ( 'NONE',  ( 113.5000000000000568, -190.7866584945343504, -447.4016117689005796 ) ) ;
#57090 = CARTESIAN_POINT ( 'NONE',  ( -70.35677490696174630, -287.9592243844340373, -339.1701881515262471 ) ) ;
#57091 = CARTESIAN_POINT ( 'NONE',  ( -69.33776954806731396, -285.0804659685678075, -336.8783928411505713 ) ) ;
#57092 = CARTESIAN_POINT ( 'NONE',  ( -1.428432174047877146, -284.7615873765060428, -203.3968648305780675 ) ) ;
#57093 = CARTESIAN_POINT ( 'NONE',  ( -76.42480920467323813, -285.0109203883594660, -332.7742844648213350 ) ) ;
#57094 = CARTESIAN_POINT ( 'NONE',  ( -71.47517675281146410, -284.3180443054658895, -335.0720714670007396 ) ) ;
#57095 = CARTESIAN_POINT ( 'NONE',  ( -72.68506834579171993, -293.5664524536089743, -203.7939000390738613 ) ) ;
#57096 = CARTESIAN_POINT ( 'NONE',  ( 27.28386481134897679, -273.1100762290441821, -231.1094067317442864 ) ) ;
#57097 = CARTESIAN_POINT ( 'NONE',  ( -67.53126134894574761, -274.0000681242288465, -199.5491508804911120 ) ) ;
#57098 = CARTESIAN_POINT ( 'NONE',  ( -109.4158251411403313, -288.3395239986521688, -293.2177928206025967 ) ) ;
#57099 = CARTESIAN_POINT ( 'NONE',  ( -6.574700718552085377, -276.6592058320854903, -340.9614332825877341 ) ) ;
#57100 = CARTESIAN_POINT ( 'NONE',  ( 4.764527462724890583, -296.4602639153259815, -331.9964357683143135 ) ) ;
#57101 = CARTESIAN_POINT ( 'NONE',  ( -48.18343439339133738, -260.4846106489495128, -445.8398854946861434 ) ) ;
#57102 = CARTESIAN_POINT ( 'NONE',  ( 10.64812456238590066, -296.9090924074130271, -330.4860931364851808 ) ) ;
#57103 = CARTESIAN_POINT ( 'NONE',  ( -105.0453732086373719, -283.6197080951067733, -241.6391943592855114 ) ) ;
#57104 = CARTESIAN_POINT ( 'NONE',  ( 0.3904103032349110491, -278.5542552050746963, -205.4846325138206851 ) ) ;
#57105 = DIRECTION ( 'NONE',  ( -0.2156506209390900430, 0.000000000000000000, -0.9764705882352960886 ) ) ;
#57106 = CARTESIAN_POINT ( 'NONE',  ( -96.38714683788903415, -271.6871196828031998, -222.0050020251756564 ) ) ;
#57107 = CARTESIAN_POINT ( 'NONE',  ( -72.89883278356163032, -276.8850848172081101, -334.2471339079709196 ) ) ;
#57108 = CARTESIAN_POINT ( 'NONE',  ( 23.14606162351636343, -294.4908024231062882, -228.2444928478107045 ) ) ;
#57109 = CARTESIAN_POINT ( 'NONE',  ( -1.150794669299052497, -293.4862282978351118, -206.6784984058583632 ) ) ;
#57110 = CARTESIAN_POINT ( 'NONE',  ( -44.73121370613633729, -296.4588562552970643, -346.5633340154544157 ) ) ;
#57111 = CARTESIAN_POINT ( 'NONE',  ( -109.2754964653054799, -296.5494565336858841, -257.9301506416070993 ) ) ;
#57112 = CARTESIAN_POINT ( 'NONE',  ( -23.38877885651763222, -290.8740657422976597, -344.1049187710933097 ) ) ;
#57113 = CARTESIAN_POINT ( 'NONE',  ( -27.36999740024758410, -283.0955926159798537, -346.7660682773487224 ) ) ;
#57114 = CARTESIAN_POINT ( 'NONE',  ( -82.81943784833634936, -271.5776928330944315, -209.6977741619279811 ) ) ;
#57115 = CARTESIAN_POINT ( 'NONE',  ( 18.35296504267913420, -286.6577035833771561, -217.1136988799782443 ) ) ;
#57116 = CARTESIAN_POINT ( 'NONE',  ( -72.93573347164384302, -281.5579298806165411, -204.7492928676206247 ) ) ;
#57117 = CARTESIAN_POINT ( 'NONE',  ( -95.94705082875732671, -284.2254147920054947, -226.4427696760492097 ) ) ;
#57118 = CARTESIAN_POINT ( 'NONE',  ( -10.30860769527706289, -286.6991876892269033, -340.3197669299837003 ) ) ;
#57119 = CARTESIAN_POINT ( 'NONE',  ( 89.65909921107042635, 79.73535476480827811, -300.8268380169218972 ) ) ;
#57120 = CARTESIAN_POINT ( 'NONE',  ( -11.99475968347147692, -285.8988215653403131, -201.8372458521104420 ) ) ;
#57121 = CARTESIAN_POINT ( 'NONE',  ( -10.77218981492375072, -283.6553643448311277, -342.4376012753236296 ) ) ;
#57122 = CARTESIAN_POINT ( 'NONE',  ( -112.9382155646799930, -289.7782652271950496, -257.0199386058425830 ) ) ;
#57123 = CARTESIAN_POINT ( 'NONE',  ( -107.7809798661091492, -280.5255459192690637, -241.2965642502736330 ) ) ;
#57124 = CARTESIAN_POINT ( 'NONE',  ( -84.27768560191996983, -280.7372519531672310, -209.8762566701305445 ) ) ;
#57125 = CARTESIAN_POINT ( 'NONE',  ( 26.85404104593239083, -281.8596809207245997, -305.1160718683655091 ) ) ;
#57126 = CARTESIAN_POINT ( 'NONE',  ( 16.87543678902525457, -276.8239737314597733, -218.4641316652456737 ) ) ;
#57127 = CARTESIAN_POINT ( 'NONE',  ( -61.59156506239160223, -295.3585754478501713, -343.4986196502385383 ) ) ;
#57128 = CARTESIAN_POINT ( 'NONE',  ( -70.73033779678549138, -287.5148011609784362, -337.1364013218289415 ) ) ;
#57129 = CARTESIAN_POINT ( 'NONE',  ( -2.440602311976399541, -294.1061240800694918, -202.6091071351043809 ) ) ;
#57130 = CARTESIAN_POINT ( 'NONE',  ( -108.8965749324479333, -295.2630727645437219, -286.3024468618982041 ) ) ;
#57131 = ORIENTED_EDGE ( 'NONE', *, *, #67705, .T. ) ;
#57132 = CARTESIAN_POINT ( 'NONE',  ( -18.34500948516543062, -284.7257828497566834, -342.3898341017015241 ) ) ;
#57133 = CARTESIAN_POINT ( 'NONE',  ( -109.7566344058575964, -296.3477331068804688, -260.5897039882700028 ) ) ;
#57134 = CARTESIAN_POINT ( 'NONE',  ( 39.29847969715857658, -294.6668356569264802, -273.1495485930986433 ) ) ;
#57135 = CARTESIAN_POINT ( 'NONE',  ( -36.18360817194103163, -283.6886669524637341, -343.4538774841473128 ) ) ;
#57136 = ADVANCED_FACE ( 'NONE', ( #78078, #34975, #14616, #42530, #78540 ), #63889, .T. ) ;
#57137 = CARTESIAN_POINT ( 'NONE',  ( -36.92892426766344016, -273.1159871622386959, -193.5845085195130366 ) ) ;
#57138 = CARTESIAN_POINT ( 'NONE',  ( -51.65818546520302590, -289.8821002412654479, -345.9147481658728793 ) ) ;
#57139 = CARTESIAN_POINT ( 'NONE',  ( -3.466709903770705203, -280.7494329135404314, -338.1456643307538457 ) ) ;
#57140 = CARTESIAN_POINT ( 'NONE',  ( -107.2430110538742554, -291.2994238896230286, -237.9920331185965097 ) ) ;
#57141 = CARTESIAN_POINT ( 'NONE',  ( 12.17325497759521546, -288.6739031020745756, -324.0987852835651779 ) ) ;
#57142 = LINE ( 'NONE', #85983, #18724 ) ;
#57143 = CARTESIAN_POINT ( 'NONE',  ( -22.78264641048746597, -118.9815703160634541, -21.50000000000000000 ) ) ;
#57144 = CARTESIAN_POINT ( 'NONE',  ( 121.4028569870072971, 147.5259734495768669, -260.2187139711599002 ) ) ;
#57145 = CARTESIAN_POINT ( 'NONE',  ( -110.4542110544635705, -270.2666405000204009, -253.6410175316879361 ) ) ;
#57146 = CARTESIAN_POINT ( 'NONE',  ( -108.3312468908004860, -277.5157186597799068, -288.1070286343262410 ) ) ;
#57147 = ORIENTED_EDGE ( 'NONE', *, *, #72919, .F. ) ;
#57148 = CARTESIAN_POINT ( 'NONE',  ( -54.55207517852110755, -278.7462307273775650, -199.0484115112007544 ) ) ;
#57149 = CARTESIAN_POINT ( 'NONE',  ( 37.61529595931217074, -274.9989619022424563, -252.7768409693519800 ) ) ;
#57150 = CARTESIAN_POINT ( 'NONE',  ( 123.2339866187729598, 147.3305397618446761, -261.4581277174236220 ) ) ;
#57151 = ADVANCED_FACE ( 'NONE', ( #85161 ), #59057, .T. ) ;
#57152 = CARTESIAN_POINT ( 'NONE',  ( -68.41615132926648357, -278.2265983074422024, -200.5400767411933600 ) ) ;
#57153 = CARTESIAN_POINT ( 'NONE',  ( -79.32202510925571914, -281.6420802453622514, -332.0822579186136636 ) ) ;
#57154 = CARTESIAN_POINT ( 'NONE',  ( -85.73252688891574280, -297.4716991039567802, -328.9469686353702969 ) ) ;
#57155 = CARTESIAN_POINT ( 'NONE',  ( 33.70613836740976410, -293.8193092850265202, -253.2726355837552887 ) ) ;
#57156 = ORIENTED_EDGE ( 'NONE', *, *, #60783, .F. ) ;
#57157 = CARTESIAN_POINT ( 'NONE',  ( -105.5771151798270751, -288.8724559585137399, -297.7956129173536510 ) ) ;
#57158 = CARTESIAN_POINT ( 'NONE',  ( -35.53450855500613415, -274.7256487033095596, -193.4711760317047720 ) ) ;
#57159 = CARTESIAN_POINT ( 'NONE',  ( -94.61271035972472987, -273.1909261468162526, -225.0948900963422545 ) ) ;
#57160 = ORIENTED_EDGE ( 'NONE', *, *, #79357, .F. ) ;
#57161 = CARTESIAN_POINT ( 'NONE',  ( 157.4970531492008661, 250.0000000000000568, 16.90571646082702983 ) ) ;
#57162 = CARTESIAN_POINT ( 'NONE',  ( 155.3778607292159677, 20.99999999999999645, -15.20506116941400165 ) ) ;
#57163 = B_SPLINE_CURVE_WITH_KNOTS ( 'NONE', 3,
 ( #36804, #21202, #65725, #37716, #836, #66622, #30634, #58600, #88383, #75583, #52402, #38180, #38657, #16425, #45277, #32959 ),
 .UNSPECIFIED., .F., .F.,
 ( 4, 2, 2, 2, 2, 2, 2, 4 ),
 ( 0.1790892544726606084, 0.2192030976635781225, 0.2593169408544956367, 0.2994307840454131231, 0.3395446272363306095, 0.3796584704272480959, 0.4197723136181656378, 0.5000000000000000000 ),
 .UNSPECIFIED. ) ;
#57164 = CARTESIAN_POINT ( 'NONE',  ( -113.5000000000000568, -190.7866584945343220, -490.8867980474134356 ) ) ;
#57165 = CARTESIAN_POINT ( 'NONE',  ( -30.24609430240859353, -281.2235581765413599, -197.3456372872051929 ) ) ;
#57166 = CARTESIAN_POINT ( 'NONE',  ( -28.36722641797974731, -281.9245260274670954, -194.8533604755647559 ) ) ;
#57167 = CARTESIAN_POINT ( 'NONE',  ( -89.06894425974725493, -282.8599196068099104, -322.2753491389266856 ) ) ;
#57168 = CARTESIAN_POINT ( 'NONE',  ( 23.10574395892109578, -282.8205770558491281, -227.2685201845750100 ) ) ;
#57169 = CARTESIAN_POINT ( 'NONE',  ( 12.19962523608213090, -274.8280794452312534, -324.9864160017370978 ) ) ;
#57170 = PLANE ( 'NONE',  #59357 ) ;
#57171 = DIRECTION ( 'NONE',  ( 0.000000000000000000, 0.000000000000000000, 1.000000000000000000 ) ) ;
#57172 = CARTESIAN_POINT ( 'NONE',  ( -110.5097548597353239, -279.0573914041060561, -293.9971085231694019 ) ) ;
#57173 = CARTESIAN_POINT ( 'NONE',  ( 123.4306832106270946, -134.2641364535880939, 0.000000000000000000 ) ) ;
#57174 = ORIENTED_EDGE ( 'NONE', *, *, #72721, .F. ) ;
#57175 = FACE_OUTER_BOUND ( 'NONE', #48130, .T. ) ;
#57176 = CARTESIAN_POINT ( 'NONE',  ( -47.01960340857906573, -285.1543968441169454, -345.0922693801278456 ) ) ;
#57177 = CARTESIAN_POINT ( 'NONE',  ( 21.94154536604866834, -292.1506265979649584, -227.4667592680269195 ) ) ;
#57178 = CARTESIAN_POINT ( 'NONE',  ( 32.76853770057452664, -287.3047797470836144, -301.9501562377100186 ) ) ;
#57179 = CARTESIAN_POINT ( 'NONE',  ( -62.89193534206738434, -283.9548899151191677, -200.8431004805752593 ) ) ;
#57181 = CARTESIAN_POINT ( 'NONE',  ( -26.34618162670978947, -287.1502995099515374, -343.6048999761332539 ) ) ;
#57180 = CARTESIAN_POINT ( 'NONE',  ( -105.1333447811755377, -283.5096275338648297, -241.6003774355187375 ) ) ;
#57182 = CARTESIAN_POINT ( 'NONE',  ( -37.52619258083087317, -284.2596254218029799, -343.7704570217542823 ) ) ;
#57183 = CARTESIAN_POINT ( 'NONE',  ( 16.66751951071931970, -272.8198321970713209, -218.2480451313527396 ) ) ;
#57184 = CARTESIAN_POINT ( 'NONE',  ( -113.1105788464700623, -282.8497328983733041, -278.4554019020054625 ) ) ;
#57185 = CARTESIAN_POINT ( 'NONE',  ( -36.27661821145474619, -297.0389920560507448, -345.3663223176694146 ) ) ;
#57186 = CARTESIAN_POINT ( 'NONE',  ( -67.73552806259097281, -283.6541095752592696, -201.5994054247314580 ) ) ;
#57187 = CARTESIAN_POINT ( 'NONE',  ( -83.59559592967119102, -280.3410856909468976, -213.5153204770480215 ) ) ;
#57188 = EDGE_CURVE ( 'NONE', #30831, #90289, #79925, .T. ) ;
#57189 = CARTESIAN_POINT ( 'NONE',  ( 140.6539576904058606, 249.5000000000000568, -10.49999999999999822 ) ) ;
#57190 = FACE_OUTER_BOUND ( 'NONE', #49853, .T. ) ;
#57191 = CARTESIAN_POINT ( 'NONE',  ( 28.33535374304726417, -295.9679175910864615, -307.8277992328399364 ) ) ;
#57192 = CARTESIAN_POINT ( 'NONE',  ( -110.7268525702525892, -276.3532372884859569, -285.8407837970616470 ) ) ;
#57193 = CARTESIAN_POINT ( 'NONE',  ( -103.0723992339431447, -290.2709716151322823, -230.4636555132805995 ) ) ;
#57194 = CARTESIAN_POINT ( 'NONE',  ( 16.73158051365991739, -292.6661275954513144, -320.5858204322466349 ) ) ;
#57195 = CARTESIAN_POINT ( 'NONE',  ( -43.77769788857359856, -278.6540795477220058, -197.0997434678387208 ) ) ;
#57196 = CARTESIAN_POINT ( 'NONE',  ( -103.2951584642906511, -271.0939850566395535, -235.7320767071639693 ) ) ;
#57197 = CARTESIAN_POINT ( 'NONE',  ( -93.82955868861657223, -292.5300387966336757, -223.3269435335836306 ) ) ;
#57198 = CARTESIAN_POINT ( 'NONE',  ( -85.28047601435906699, -286.1948066931273615, -330.5268031993605859 ) ) ;
#57199 = CARTESIAN_POINT ( 'NONE',  ( -11.31208035220853780, -293.1990793112764209, -342.1469892098484138 ) ) ;
#57200 = CARTESIAN_POINT ( 'NONE',  ( -71.52541129064096026, -291.1116395513638508, -335.7811601952328147 ) ) ;
#57201 = CARTESIAN_POINT ( 'NONE',  ( -34.96929491566408643, -290.3213960246039846, -194.3985150574085878 ) ) ;
#57202 = CARTESIAN_POINT ( 'NONE',  ( -42.68875334143204014, -290.5460647466658770, -343.8068434839705674 ) ) ;
#57203 = DIRECTION ( 'NONE',  ( 0.000000000000000000, 0.000000000000000000, 1.000000000000000000 ) ) ;
#57204 = CARTESIAN_POINT ( 'NONE',  ( -5.713389437453334274, -289.4280564095175237, -336.3327155866107887 ) ) ;
#57205 = FACE_OUTER_BOUND ( 'NONE', #18092, .T. ) ;
#57206 = CARTESIAN_POINT ( 'NONE',  ( -113.7152737123392825, -291.6745858203403827, -276.9348716747363710 ) ) ;
#57208 = CARTESIAN_POINT ( 'NONE',  ( -108.6627219916117895, -290.3460958610340299, -285.9855972731699012 ) ) ;
#57207 = CARTESIAN_POINT ( 'NONE',  ( 18.54631275297971271, -280.2743613275927714, -320.9838113474575039 ) ) ;
#57209 = CARTESIAN_POINT ( 'NONE',  ( -59.30017208588333233, -280.1087202447411073, -196.5805663396793932 ) ) ;
#57210 = CARTESIAN_POINT ( 'NONE',  ( 4.530635706834868159, -282.1707915009040448, -335.0186348953547508 ) ) ;
#57211 = CARTESIAN_POINT ( 'NONE',  ( 21.92257918866998523, -286.1823452636505749, -316.3465169579442886 ) ) ;
#57212 = PLANE ( 'NONE',  #86721 ) ;
#57213 = CARTESIAN_POINT ( 'NONE',  ( 14.77526791730137923, -280.4484569966114123, -323.2982713932576075 ) ) ;
#57214 = CARTESIAN_POINT ( 'NONE',  ( -102.2952847834866930, -283.0536750571794755, -232.7607990155565574 ) ) ;
#57215 = APPLICATION_CONTEXT ( 'automotive_design' ) ;
#57216 = DIRECTION ( 'NONE',  ( 0.000000000000000000, 1.000000000000000000, 0.000000000000000000 ) ) ;
#57217 = CARTESIAN_POINT ( 'NONE',  ( -108.0215781079693897, -276.6634829867090843, -299.1198140572902844 ) ) ;
#57218 = CARTESIAN_POINT ( 'NONE',  ( -12.78960523482254885, -285.2843270950392593, -197.7065438278079910 ) ) ;
#57219 = CARTESIAN_POINT ( 'NONE',  ( -27.27806132797662642, -274.9860188879577549, -197.8440815844289205 ) ) ;
#57220 = CARTESIAN_POINT ( 'NONE',  ( 114.7448031289451222, -299.5541904835127980, -192.4214616598467273 ) ) ;
#57221 = CARTESIAN_POINT ( 'NONE',  ( -47.12041845921879002, -293.5259977270851550, -197.2118385478385676 ) ) ;
#57222 = CARTESIAN_POINT ( 'NONE',  ( 37.90863464353293466, -276.8092866274533321, -257.0202020678862027 ) ) ;
#57223 = CARTESIAN_POINT ( 'NONE',  ( -70.46618380594966879, -277.1681781447261415, -335.4368897254521471 ) ) ;
#57224 = CARTESIAN_POINT ( 'NONE',  ( -111.9950936832419472, -290.9554713978622544, -251.4434639793408053 ) ) ;
#57225 = CARTESIAN_POINT ( 'NONE',  ( 36.84559428790554847, -279.4492764055048042, -256.0237699762428178 ) ) ;
#57226 = CARTESIAN_POINT ( 'NONE',  ( 11.12043451956602169, -292.5350696141254048, -210.4558940542265191 ) ) ;
#57227 = CARTESIAN_POINT ( 'NONE',  ( -83.96965594986329506, -290.4516713222828912, -213.8877421027370076 ) ) ;
#57228 = CARTESIAN_POINT ( 'NONE',  ( 16.11761735759916192, -292.2941826330477397, -323.0382098874331973 ) ) ;
#57229 = ORIENTED_EDGE ( 'NONE', *, *, #16334, .F. ) ;
#57230 = CARTESIAN_POINT ( 'NONE',  ( 189.9243309297870610, 275.5000000000000568, 20.22542485937349355 ) ) ;
#57231 = CARTESIAN_POINT ( 'NONE',  ( 21.85825109088264639, -292.4610618157944941, -227.5221553818784059 ) ) ;
#57232 = DIRECTION ( 'NONE',  ( 0.000000000000000000, 0.000000000000000000, 1.000000000000000000 ) ) ;
#57233 = CARTESIAN_POINT ( 'NONE',  ( -6.941161984400256557, -271.9809262143061233, -207.3071070584150277 ) ) ;
#57234 = CARTESIAN_POINT ( 'NONE',  ( -95.41138479463613464, -294.9306069910667247, -320.5680093043957299 ) ) ;
#57235 = CARTESIAN_POINT ( 'NONE',  ( -109.5176107783252917, -286.1894963474462656, -244.9852200883260593 ) ) ;
#57236 = CARTESIAN_POINT ( 'NONE',  ( -27.83445044074651165, -286.0095681809751227, -197.9828601430970707 ) ) ;
#57237 = CARTESIAN_POINT ( 'NONE',  ( 36.27851160155952925, -277.0163323146715015, -266.0795742938309445 ) ) ;
#57238 = CARTESIAN_POINT ( 'NONE',  ( -7.350068831619500642, -292.6770215717642145, -338.7295805699538391 ) ) ;
#57239 = CARTESIAN_POINT ( 'NONE',  ( -108.4389337298712519, -298.5806465622432029, -249.7903282865496521 ) ) ;
#57240 = CARTESIAN_POINT ( 'NONE',  ( 36.04020802804998169, -274.3274940996295754, -268.8691196571160162 ) ) ;
#57241 = EDGE_LOOP ( 'NONE', ( #5181, #84592, #91534, #9315 ) ) ;
#57242 = FACE_OUTER_BOUND ( 'NONE', #88867, .T. ) ;
#57243 = CARTESIAN_POINT ( 'NONE',  ( -66.92023900696986516, -295.0960279561686548, -341.4446789513162912 ) ) ;
#57244 = CARTESIAN_POINT ( 'NONE',  ( 31.83220830565329607, -289.8347671409260329, -298.0008877410383548 ) ) ;
#57245 = DIRECTION ( 'NONE',  ( 1.000000000000000000, 0.000000000000000000, 0.000000000000000000 ) ) ;
#57246 = CARTESIAN_POINT ( 'NONE',  ( -100.8877902063416485, -274.3247652036166073, -227.4892895565202480 ) ) ;
#57247 = CARTESIAN_POINT ( 'NONE',  ( 31.49817532150609622, -288.5305974993274276, -294.9571383140427656 ) ) ;
#57249 = ORIENTED_EDGE ( 'NONE', *, *, #90014, .F. ) ;
#57248 = EDGE_CURVE ( 'NONE', #75719, #7041, #23081, .T. ) ;
#57250 = CARTESIAN_POINT ( 'NONE',  ( -69.85178790822799044, -278.6932197091731496, -200.8060342518697041 ) ) ;
#57251 = CARTESIAN_POINT ( 'NONE',  ( -64.22277405604366152, -296.0452728255502279, -342.4077740534941086 ) ) ;
#57252 = CARTESIAN_POINT ( 'NONE',  ( -54.24939633010384910, -287.4065000605688738, -344.2691044333760715 ) ) ;
#57253 = CARTESIAN_POINT ( 'NONE',  ( -61.58088049430824640, -295.6918029353748807, -343.4798708562101979 ) ) ;
#57254 = CARTESIAN_POINT ( 'NONE',  ( 20.54256203885854504, -294.5119443429359762, -314.8956309882918845 ) ) ;
#57255 = CARTESIAN_POINT ( 'NONE',  ( 196.2775840954750208, 71.85475162903931334, -11.57395220326623964 ) ) ;
#57256 = FACE_OUTER_BOUND ( 'NONE', #18181, .T. ) ;
#57257 = CARTESIAN_POINT ( 'NONE',  ( 37.34089866539330416, -288.8738484990258257, -254.6385142663085617 ) ) ;
#57258 = CARTESIAN_POINT ( 'NONE',  ( -55.56934967048407970, -289.3380690714490129, -190.3538533559490702 ) ) ;
#57259 = ORIENTED_EDGE ( 'NONE', *, *, #7154, .T. ) ;
#57260 = CARTESIAN_POINT ( 'NONE',  ( -103.3198664937667530, -278.4176495018903665, -230.7583048782927051 ) ) ;
#57261 = CARTESIAN_POINT ( 'NONE',  ( -7.746323770853920543, -284.6635433926473411, -339.0935130160386279 ) ) ;
#57262 = CARTESIAN_POINT ( 'NONE',  ( -106.1406452522187323, -283.5567514552673174, -237.1148935189554550 ) ) ;
#57263 = CARTESIAN_POINT ( 'NONE',  ( -51.03998138331096612, -287.3082637710973586, -343.5826057218839651 ) ) ;
#57264 = CARTESIAN_POINT ( 'NONE',  ( -17.65564194824074562, -278.6612672932710097, -343.5237080903923470 ) ) ;
#57265 = ORIENTED_EDGE ( 'NONE', *, *, #44269, .F. ) ;
#57267 = CARTESIAN_POINT ( 'NONE',  ( -72.17098014583973509, -278.9270496204223377, -206.0897097061223917 ) ) ;
#57266 = CARTESIAN_POINT ( 'NONE',  ( -74.01327642203473545, -277.5540697996185600, -333.4816019169909964 ) ) ;
#57268 = CARTESIAN_POINT ( 'NONE',  ( -46.85633122383234905, -275.0136878641828844, -194.2627322943047261 ) ) ;
#57269 = CARTESIAN_POINT ( 'NONE',  ( -113.6468991498996104, -277.4391573486000766, -263.0365485044620755 ) ) ;
#57270 = CARTESIAN_POINT ( 'NONE',  ( 63.23836714137711112, 47.77599596953215411, -316.5090406242446761 ) ) ;
#57271 = CARTESIAN_POINT ( 'NONE',  ( -67.45441980011311500, -274.6079407048925418, -199.7491903263003792 ) ) ;
#57272 = ADVANCED_FACE ( 'NONE', ( #81770 ), #43924, .T. ) ;
#57273 = CARTESIAN_POINT ( 'NONE',  ( -15.04246470041792705, -299.7514418032953358, -193.9450587403573820 ) ) ;
#57274 = CARTESIAN_POINT ( 'NONE',  ( -54.49178911615187815, -288.3376638359845856, -195.3683826091709363 ) ) ;
#57275 = VERTEX_POINT ( 'NONE', #30198 ) ;
#57276 = CIRCLE ( 'NONE', #10322, 25.00000000000000355 ) ;
#57277 = CARTESIAN_POINT ( 'NONE',  ( 82.65162136640255142, -299.3405935325396854, -192.8643928579782596 ) ) ;
#57278 = CARTESIAN_POINT ( 'NONE',  ( -46.77822599613994470, -287.0093449685113001, -197.6108968973923652 ) ) ;
#57279 = CARTESIAN_POINT ( 'NONE',  ( 0.9908731529661984894, -288.3164198519621095, -204.7366259479212260 ) ) ;
#57280 = CARTESIAN_POINT ( 'NONE',  ( 22.03965603196966683, -287.4959265442595324, -312.9961647043861603 ) ) ;
#57281 = CARTESIAN_POINT ( 'NONE',  ( -114.1473530375246241, -283.9928917890878211, -275.7072527118373273 ) ) ;
#57282 = CARTESIAN_POINT ( 'NONE',  ( -74.89551508447735273, -277.9433878448719497, -206.7716755640965687 ) ) ;
#57283 = CARTESIAN_POINT ( 'NONE',  ( -46.90711468948353513, -287.7899637299429969, -196.6931233092008426 ) ) ;
#57284 = CARTESIAN_POINT ( 'NONE',  ( 33.62192456028797949, -280.2922032504346816, -290.2324975170747052 ) ) ;
#57285 = CARTESIAN_POINT ( 'NONE',  ( -48.66742310038758035, -278.5144238102573695, -343.0280814630534678 ) ) ;
#57286 = CARTESIAN_POINT ( 'NONE',  ( 28.08840541023383253, -276.4863082384095492, -302.9850296949877020 ) ) ;
#57287 = CARTESIAN_POINT ( 'NONE',  ( -71.74197864103589950, -288.2915764510409531, -338.8054717186547578 ) ) ;
#57288 = CARTESIAN_POINT ( 'NONE',  ( -24.55037457845733329, -283.6958537371342572, -346.1814783090250671 ) ) ;
#57289 = CARTESIAN_POINT ( 'NONE',  ( -107.8722291171190193, -285.4382007472626128, -239.4874949684683827 ) ) ;
#57290 = CARTESIAN_POINT ( 'NONE',  ( -24.87847801729734698, -280.3822679026047808, -198.4329030797603650 ) ) ;
#57291 = EDGE_LOOP ( 'NONE', ( #85326, #90368, #4135, #3198, #87233 ) ) ;
#57292 = EDGE_LOOP ( 'NONE', ( #16965, #89466, #2949, #68532 ) ) ;
#57293 = DIRECTION ( 'NONE',  ( 1.000000000000000000, 0.000000000000000000, 0.000000000000000000 ) ) ;
#57294 = CARTESIAN_POINT ( 'NONE',  ( -70.08347964180700274, -291.3392148065165088, -338.7001921549091890 ) ) ;
#57295 = CARTESIAN_POINT ( 'NONE',  ( -93.24398708872134023, -288.5194553016125951, -322.6699744567048356 ) ) ;
#57296 = CARTESIAN_POINT ( 'NONE',  ( -109.8138290549240708, -271.7541084127307158, -259.4698463676803613 ) ) ;
#57297 = CARTESIAN_POINT ( 'NONE',  ( 34.35345792672862331, -293.2534736440766210, -298.1661013100909372 ) ) ;
#57298 = CARTESIAN_POINT ( 'NONE',  ( -45.45785259689345992, -287.6367268037397480, -343.6061575484424111 ) ) ;
#57299 = CARTESIAN_POINT ( 'NONE',  ( 30.79730872466732450, -291.4078086117562520, -241.3326806734435763 ) ) ;
#57300 = CARTESIAN_POINT ( 'NONE',  ( 34.09324062552919088, -288.5353403252199200, -253.4492162859894790 ) ) ;
#57301 = CARTESIAN_POINT ( 'NONE',  ( -110.4683760289727132, -287.2662352645559167, -253.7030783399848985 ) ) ;
#57302 = CARTESIAN_POINT ( 'NONE',  ( -38.85363861546067454, -291.0712801540556711, -345.3458810641479317 ) ) ;
#57303 = CARTESIAN_POINT ( 'NONE',  ( -55.71539521935919481, -289.8161491601089779, -197.4210253949140395 ) ) ;
#57304 = CARTESIAN_POINT ( 'NONE',  ( 21.60561533811403123, -294.9154703852302077, -223.9703455894943716 ) ) ;
#57305 = CARTESIAN_POINT ( 'NONE',  ( -67.87156488716884439, -284.4042948232743697, -336.9293972649542752 ) ) ;
#57306 = CARTESIAN_POINT ( 'NONE',  ( -35.04263018413994502, -294.0810897534220771, -195.2167780110804358 ) ) ;
#57307 = DIRECTION ( 'NONE',  ( 0.5370370370370221025, -0.000000000000000000, 0.8435586647355927115 ) ) ;
#57308 = CARTESIAN_POINT ( 'NONE',  ( 180.6209651459523968, 250.5000000000000568, -24.41176470588238345 ) ) ;
#57309 = CARTESIAN_POINT ( 'NONE',  ( -60.39249233915681714, -275.7347405013114781, -198.5636014117943944 ) ) ;
#57310 = CARTESIAN_POINT ( 'NONE',  ( 34.09587835474437867, -280.9571334538154588, -286.1495348777308436 ) ) ;
#57311 = CARTESIAN_POINT ( 'NONE',  ( -74.81765440468608119, -281.5504951712472348, -335.3860967848603991 ) ) ;
#57312 = CARTESIAN_POINT ( 'NONE',  ( -112.1509457559398015, -295.5287578501248618, -287.9604542025837191 ) ) ;
#57313 = CARTESIAN_POINT ( 'NONE',  ( -63.64619764083871445, -271.9443874272685093, -201.1661740105528793 ) ) ;
#57314 = CARTESIAN_POINT ( 'NONE',  ( -68.66518493698950465, -275.5469084806538831, -337.9040479613337311 ) ) ;
#57315 = CARTESIAN_POINT ( 'NONE',  ( -106.2741744465558469, -298.2066209120147278, -244.7278190104321425 ) ) ;
#57316 = CARTESIAN_POINT ( 'NONE',  ( -49.60663242516901761, -272.4735553194852287, -194.8877169495650037 ) ) ;
#57317 = CARTESIAN_POINT ( 'NONE',  ( -107.2723681662464941, -298.2810192462973191, -247.2848950909272787 ) ) ;
#57318 = DIRECTION ( 'NONE',  ( -1.000000000000000000, -0.000000000000000000, -0.000000000000000000 ) ) ;
#57319 = CARTESIAN_POINT ( 'NONE',  ( 1.664555189878213159, -295.3191778065638573, -332.3171145202270509 ) ) ;
#57320 = CARTESIAN_POINT ( 'NONE',  ( 152.1970976711774597, 130.7369940202023884, 11.50000000000000178 ) ) ;
#57322 = CARTESIAN_POINT ( 'NONE',  ( -110.3416211263863289, -272.4214311790046281, -267.6351414138766245 ) ) ;
#57321 = CARTESIAN_POINT ( 'NONE',  ( 25.77418742970241539, -285.0196521069949540, -229.1932720331928124 ) ) ;
#57323 = CARTESIAN_POINT ( 'NONE',  ( -76.10672076045177903, -285.5495102620312196, -203.7694751957007213 ) ) ;
#57324 = CARTESIAN_POINT ( 'NONE',  ( 18.62652873171720813, -287.9408436094007016, -323.2128128447901645 ) ) ;
#57325 = CARTESIAN_POINT ( 'NONE',  ( 16.40644411584795748, -296.2735937243684816, -323.2514933945663529 ) ) ;
#57326 = CARTESIAN_POINT ( 'NONE',  ( -11.60638090825217894, -290.3877722155161223, -200.0369548763536898 ) ) ;
#57327 = CARTESIAN_POINT ( 'NONE',  ( -100.1111613704287890, -278.3369986359605832, -226.0423459327373337 ) ) ;
#57328 = CARTESIAN_POINT ( 'NONE',  ( -54.42813229853332757, -283.3380690714490129, -195.3538533559490702 ) ) ;
#57329 = CARTESIAN_POINT ( 'NONE',  ( 194.7453183674696220, 20.99999999999998934, 15.62500000000049205 ) ) ;
#57330 = CARTESIAN_POINT ( 'NONE',  ( 28.57768800970790224, -286.7819211596159334, -302.6374989932680819 ) ) ;
#57331 = CARTESIAN_POINT ( 'NONE',  ( 197.0505512480903008, 72.68507397627607247, -12.20517631820067272 ) ) ;
#57332 = CARTESIAN_POINT ( 'NONE',  ( 15.47422765890346419, -286.3052212953550679, -323.6103284888396274 ) ) ;
#57333 = CARTESIAN_POINT ( 'NONE',  ( -109.2611973564170711, -298.3682866332154617, -253.8073771302953219 ) ) ;
#57334 = CARTESIAN_POINT ( 'NONE',  ( -1.428545143471469103, -281.9441730135347370, -202.9159432622016936 ) ) ;
#57336 = CARTESIAN_POINT ( 'NONE',  ( 31.07030355454676496, -281.2106873776272664, -244.7445871767365304 ) ) ;
#57335 = CARTESIAN_POINT ( 'NONE',  ( -98.57007099884434353, -295.1670924467572945, -226.4351187910079659 ) ) ;
#57337 = CARTESIAN_POINT ( 'NONE',  ( -86.39368527885039839, -295.8784943767423670, -329.7151638198332648 ) ) ;
#57338 = CARTESIAN_POINT ( 'NONE',  ( -90.55984317352236701, -298.8016330983899138, -219.3122210049654939 ) ) ;
#57339 = CARTESIAN_POINT ( 'NONE',  ( -15.80013513929826807, -284.4083932734251903, -197.8824834857215080 ) ) ;
#57340 = EDGE_CURVE ( 'NONE', #37982, #91222, #1316, .T. ) ;
#57341 = CARTESIAN_POINT ( 'NONE',  ( -34.02975750886035655, -282.0939795243029380, -195.4342757497672380 ) ) ;
#57343 = CARTESIAN_POINT ( 'NONE',  ( -82.07840579873577269, -296.4840181938811838, -212.3137906870738050 ) ) ;
#57342 = CIRCLE ( 'NONE', #86022, 0.5000000000000014433 ) ;
#57344 = ORIENTED_EDGE ( 'NONE', *, *, #24741, .F. ) ;
#57345 = DIRECTION ( 'NONE',  ( 0.000000000000000000, 0.000000000000000000, 1.000000000000000000 ) ) ;
#57346 = CARTESIAN_POINT ( 'NONE',  ( 8.830721140459937502, -284.3957791549856324, -329.0782714599445740 ) ) ;
#57347 = FACE_OUTER_BOUND ( 'NONE', #64149, .T. ) ;
#57348 = CARTESIAN_POINT ( 'NONE',  ( -20.19161114001082069, -289.7666405000204009, -195.3683826091709363 ) ) ;
#57349 = CARTESIAN_POINT ( 'NONE',  ( 35.57996422771566358, -274.4419066435889363, -245.9737148925808583 ) ) ;
#57350 = CARTESIAN_POINT ( 'NONE',  ( -37.54781906493271038, -291.8828564907146870, -197.3489651963502922 ) ) ;
#57351 = CARTESIAN_POINT ( 'NONE',  ( 31.71327903191885511, -282.7305645020238103, -244.4831765541178754 ) ) ;
#57352 = CARTESIAN_POINT ( 'NONE',  ( 17.13530689902991355, -277.8588632816119457, -320.1664778849046229 ) ) ;
#57353 = CARTESIAN_POINT ( 'NONE',  ( 20.84004401143931773, -279.7205639435949820, -225.5968010284620107 ) ) ;
#57354 = CARTESIAN_POINT ( 'NONE',  ( -109.0207153024304461, -280.2657354849513922, -292.6056084190050797 ) ) ;
#57355 = CARTESIAN_POINT ( 'NONE',  ( -93.17362774639011036, -273.4436849761018493, -217.3155065374579067 ) ) ;
#57356 = CARTESIAN_POINT ( 'NONE',  ( 36.06199122632855847, -275.6777916550140617, -293.6183340681683944 ) ) ;
#57357 = CARTESIAN_POINT ( 'NONE',  ( 15.88844557785086486, -294.7332305639542938, -218.2501570742107617 ) ) ;
#57358 = DIRECTION ( 'NONE',  ( -0.000000000000000000, 1.000000000000000000, -0.000000000000000000 ) ) ;
#57359 = DIRECTION ( 'NONE',  ( 0.000000000000000000, 1.000000000000000000, 0.000000000000000000 ) ) ;
#57360 = EDGE_CURVE ( 'NONE', #67960, #72522, #66653, .T. ) ;
#57361 = CARTESIAN_POINT ( 'NONE',  ( -32.12164970490687210, -293.1265817275605627, -345.9589239379730543 ) ) ;
#57362 = CARTESIAN_POINT ( 'NONE',  ( -93.82195822494607285, -272.7159802506369601, -223.9953725165841831 ) ) ;
#57363 = CARTESIAN_POINT ( 'NONE',  ( 20.85156528479959093, -295.7436086463525839, -319.7195176224915940 ) ) ;
#57364 = CARTESIAN_POINT ( 'NONE',  ( 13.00589969489902309, -293.9424137320066848, -212.6278701126462067 ) ) ;
#57365 = CARTESIAN_POINT ( 'NONE',  ( -39.99812008847871425, -291.0856444114978103, -345.1981128541739281 ) ) ;
#57366 = CARTESIAN_POINT ( 'NONE',  ( -104.7943026507509217, -276.1229172564733858, -302.8875052824417367 ) ) ;
#57367 = CARTESIAN_POINT ( 'NONE',  ( -48.80594869230788646, -279.1193064502305106, -343.9654400944965005 ) ) ;
#57368 = CARTESIAN_POINT ( 'NONE',  ( 4.608112535590461967, -292.5608457392605715, -331.8552430129307140 ) ) ;
#57369 = CARTESIAN_POINT ( 'NONE',  ( 33.16609357196668384, -283.0536411182113170, -242.4879742690613682 ) ) ;
#57370 = CARTESIAN_POINT ( 'NONE',  ( -44.03898481386116259, -284.8858097898379356, -197.3585669899016182 ) ) ;
#57371 = EDGE_LOOP ( 'NONE', ( #4372, #63819, #10538, #27425, #17199 ) ) ;
#57372 = CARTESIAN_POINT ( 'NONE',  ( -18.73434406958133280, -282.4727102347819141, -341.0241147205268248 ) ) ;
#57373 = CARTESIAN_POINT ( 'NONE',  ( -11.62600901684352905, -281.4588816592911371, -198.0544428660961671 ) ) ;
#57374 = CARTESIAN_POINT ( 'NONE',  ( -108.9373471170901126, -282.9988075171709738, -297.7500061991559619 ) ) ;
#57375 = CARTESIAN_POINT ( 'NONE',  ( -100.0636743314286576, -280.0808015610927555, -226.1030772980930408 ) ) ;
#57376 = EDGE_CURVE ( 'NONE', #51665, #60383, #62388, .T. ) ;
#57377 =( NAMED_UNIT ( * ) SI_UNIT ( $, .STERADIAN. ) SOLID_ANGLE_UNIT ( ) );
#57378 = CARTESIAN_POINT ( 'NONE',  ( -41.32868539329093949, -278.6215798546141968, -346.5766469139779815 ) ) ;
#57379 = CARTESIAN_POINT ( 'NONE',  ( 30.89617123739170168, -295.8376638359844719, -254.7536222014695397 ) ) ;
#57380 = ORIENTED_EDGE ( 'NONE', *, *, #60977, .T. ) ;
#57381 = CARTESIAN_POINT ( 'NONE',  ( -35.09767873350384804, -300.0803994080620214, -195.3603442078617718 ) ) ;
#57382 = CARTESIAN_POINT ( 'NONE',  ( -95.19980865361736733, -277.2251811477385672, -223.1987804174864038 ) ) ;
#57383 = CARTESIAN_POINT ( 'NONE',  ( -108.5324448336631065, -292.6544777227440477, -243.6431769258493318 ) ) ;
#57384 = CARTESIAN_POINT ( 'NONE',  ( 35.63700618335886361, -292.8342948545750346, -265.3175621264012420 ) ) ;
#57385 = CARTESIAN_POINT ( 'NONE',  ( -99.82395989759892529, -289.4640339718997097, -315.2779471792813979 ) ) ;
#57386 = DIRECTION ( 'NONE',  ( 0.8620390091940283162, 0.000000000000000000, -0.5068419345592647396 ) ) ;
#57388 = CARTESIAN_POINT ( 'NONE',  ( -77.46712280369970927, -283.9042138801509623, -208.3618886819575096 ) ) ;
#57387 = CARTESIAN_POINT ( 'NONE',  ( -37.70453738457554493, -293.6313106962790584, -346.7840079776721609 ) ) ;
#57389 = CARTESIAN_POINT ( 'NONE',  ( -65.82239643851400501, -293.5360195313533609, -201.7929024901108619 ) ) ;
#57390 = CARTESIAN_POINT ( 'NONE',  ( -2.178076673436025956, -283.8915884332506607, -334.9104808423783197 ) ) ;
#57391 = CARTESIAN_POINT ( 'NONE',  ( -91.42422615991752366, -290.7400045099170143, -324.9143235846171365 ) ) ;
#57392 = CARTESIAN_POINT ( 'NONE',  ( 35.74878500729256103, -282.0209714190897898, -268.5758222161654771 ) ) ;
#57393 = CARTESIAN_POINT ( 'NONE',  ( 6.374744017833825716, -293.2680984406547964, -333.3294880083132057 ) ) ;
#57394 = CARTESIAN_POINT ( 'NONE',  ( -5.683665189520316297, -289.4491361807248495, -340.3748855208001487 ) ) ;
#57395 = CARTESIAN_POINT ( 'NONE',  ( -23.31699491914343980, -289.3699213476267005, -346.0646086733685252 ) ) ;
#57396 = CARTESIAN_POINT ( 'NONE',  ( -65.09518673239152520, -285.8459649828753300, -202.7888379612027450 ) ) ;
#57397 = EDGE_LOOP ( 'NONE', ( #6350, #7139 ) ) ;
#57398 = CARTESIAN_POINT ( 'NONE',  ( 195.9255997734375683, 26.17269670437365647, 13.45023288292440711 ) ) ;
#57399 = CARTESIAN_POINT ( 'NONE',  ( 36.26572443762263731, -295.6413991660483589, -288.3668686721293852 ) ) ;
#57400 = CARTESIAN_POINT ( 'NONE',  ( -113.4543212214506269, -295.1393464300450660, -278.1178687398328861 ) ) ;
#57401 = EDGE_CURVE ( 'NONE', #78639, #10505, #81308, .T. ) ;
#57402 = CARTESIAN_POINT ( 'NONE',  ( -110.3925027004790707, -277.6792061617019840, -265.1660538705651220 ) ) ;
#57403 = CARTESIAN_POINT ( 'NONE',  ( -44.03115407242199808, -273.4775149411224788, -193.6607513434001930 ) ) ;
#57404 = CIRCLE ( 'NONE', #81550, 5.103083949679981579 ) ;
#57405 = CARTESIAN_POINT ( 'NONE',  ( -76.03845361813569070, -294.0587708068583765, -333.1363986272138504 ) ) ;
#57406 = CARTESIAN_POINT ( 'NONE',  ( 18.02894103180391383, -276.6193777428455860, -221.1724151326511674 ) ) ;
#57407 = CARTESIAN_POINT ( 'NONE',  ( -65.00748298105752099, -271.8264483383052266, -201.4600407906339967 ) ) ;
#57408 = CARTESIAN_POINT ( 'NONE',  ( 27.51609864581672582, -295.2240421961290053, -304.8295736465178720 ) ) ;
#57409 = CARTESIAN_POINT ( 'NONE',  ( -73.44270288355812681, -296.6228820809637909, -334.1650651487171331 ) ) ;
#57410 = LINE ( 'NONE', #24181, #49017 ) ;
#57411 = CARTESIAN_POINT ( 'NONE',  ( -102.2534306852048331, -295.0584019366953612, -232.3574701437980536 ) ) ;
#57412 = CIRCLE ( 'NONE', #92178, 4.000000000000003553 ) ;
#57413 = CARTESIAN_POINT ( 'NONE',  ( -20.54592245100773340, -298.9086733388634229, -193.4612474181249411 ) ) ;
#57414 = CARTESIAN_POINT ( 'NONE',  ( -48.16543679440111703, -287.7671422057633208, -343.2014370238063066 ) ) ;
#57415 = DIRECTION ( 'NONE',  ( -0.7806247497997887974, 0.000000000000000000, 0.6250000000000137668 ) ) ;
#57416 = CARTESIAN_POINT ( 'NONE',  ( -104.2578474141468945, -291.0925637964194834, -300.2459760156460788 ) ) ;
#57417 = CARTESIAN_POINT ( 'NONE',  ( -35.53152440351444596, -274.5666084124854365, -193.4308338995453198 ) ) ;
#57418 = CARTESIAN_POINT ( 'NONE',  ( -66.83176999049480571, -297.9880627709171677, -203.5460620145148312 ) ) ;
#57419 = CARTESIAN_POINT ( 'NONE',  ( -89.92879280924441332, -281.2943949284703535, -216.3160927189553320 ) ) ;
#57420 = CARTESIAN_POINT ( 'NONE',  ( 39.12637323140874201, -280.2676361926265258, -272.7966935117529488 ) ) ;
#57421 = CARTESIAN_POINT ( 'NONE',  ( -58.46672194941214684, -282.6667452458896719, -344.3560215239326681 ) ) ;
#57422 = CARTESIAN_POINT ( 'NONE',  ( 38.12032187001884864, -274.7155055850394660, -255.5693627494779321 ) ) ;
#57423 = CARTESIAN_POINT ( 'NONE',  ( 10.33847168575941211, -279.0971034108006279, -210.8540775407469994 ) ) ;
#57424 = CARTESIAN_POINT ( 'NONE',  ( -8.223105111685928392, -278.4323822904095778, -201.0497082722438620 ) ) ;
#57425 = CARTESIAN_POINT ( 'NONE',  ( -35.11229096291037877, -296.7654577688189192, -196.8684749249626691 ) ) ;
#57426 = CARTESIAN_POINT ( 'NONE',  ( 5.250447008766406576, -276.6280386095629069, -208.5661857936225942 ) ) ;
#57427 = LINE ( 'NONE', #78723, #12668 ) ;
#57428 = CARTESIAN_POINT ( 'NONE',  ( 29.45292089579642436, -291.1111051836316506, -235.3648305719601979 ) ) ;
#57429 = CARTESIAN_POINT ( 'NONE',  ( -25.02144037237970764, -292.2051316212854886, -194.3531499821454815 ) ) ;
#57430 = CARTESIAN_POINT ( 'NONE',  ( 33.48234783454029184, -277.8796050543564320, -295.6936990262208269 ) ) ;
#57431 = CARTESIAN_POINT ( 'NONE',  ( 54.50831346207038308, -297.2042866843169691, -195.5591849551906591 ) ) ;
#57432 = CARTESIAN_POINT ( 'NONE',  ( -95.68723369552144220, -284.4261031900746275, -220.2817513086118595 ) ) ;
#57433 = CARTESIAN_POINT ( 'NONE',  ( 165.2424497756046549, 250.5000000000000568, 22.91843887563435800 ) ) ;
#57434 = CARTESIAN_POINT ( 'NONE',  ( -90.81678182791006293, -283.2938892299598592, -217.7009102401183895 ) ) ;
#57435 = CARTESIAN_POINT ( 'NONE',  ( -83.63170945779074827, -296.0521521680024080, -517.1711561948568487 ) ) ;
#57436 = CARTESIAN_POINT ( 'NONE',  ( 35.30292389297547118, -292.2095341346421264, -259.8783175064681359 ) ) ;
#57437 = CARTESIAN_POINT ( 'NONE',  ( -39.99473230775556232, -284.1580448918737147, -196.1733366253405393 ) ) ;
#57438 = CARTESIAN_POINT ( 'NONE',  ( 195.8564219449220616, 25.05878860812877562, 14.12689474711300086 ) ) ;
#57439 = CARTESIAN_POINT ( 'NONE',  ( -26.41588298435790350, -486.4924983417995463, -430.6442049081568939 ) ) ;
#57440 = CARTESIAN_POINT ( 'NONE',  ( -15.02125698019107070, -292.7630281929911575, -342.0174050159408239 ) ) ;
#57441 = CARTESIAN_POINT ( 'NONE',  ( -92.93975391155041166, -282.3120710611309505, -322.6446473009380043 ) ) ;
#57442 = CARTESIAN_POINT ( 'NONE',  ( -104.1021455952084835, -280.5741129216386298, -238.7848775330509454 ) ) ;
#57443 = CARTESIAN_POINT ( 'NONE',  ( -85.27644517237906996, -286.6115746906446020, -210.6093905180191257 ) ) ;
#57444 = CARTESIAN_POINT ( 'NONE',  ( -6.619247236738801554, -278.6898606552815068, -200.8480751687957309 ) ) ;
#57445 = CARTESIAN_POINT ( 'NONE',  ( 35.12421513372721193, -287.6684268581126389, -279.1753749148476231 ) ) ;
#57446 = CARTESIAN_POINT ( 'NONE',  ( -39.15422912802713284, -278.5006164769621932, -343.9280239747898236 ) ) ;
#57447 = CARTESIAN_POINT ( 'NONE',  ( -94.92427309393181645, -279.9900994756662271, -225.2094862833691877 ) ) ;
#57448 = CARTESIAN_POINT ( 'NONE',  ( 6.564666552719763182, -288.6251064464843807, -209.0544150087766297 ) ) ;
#57449 = ORIENTED_EDGE ( 'NONE', *, *, #13625, .F. ) ;
#57450 = CARTESIAN_POINT ( 'NONE',  ( -14.80798891540781703, -298.1603007223051804, -193.3617316766313365 ) ) ;
#57451 = CARTESIAN_POINT ( 'NONE',  ( -34.49047466810819174, -290.9961725953706377, -345.0021454943353092 ) ) ;
#57452 = CARTESIAN_POINT ( 'NONE',  ( 114.7448031289451222, -299.5541904835127980, -195.3611179825600175 ) ) ;
#57453 = CARTESIAN_POINT ( 'NONE',  ( 36.60358173371528068, -284.4805209788416391, -305.9350535429201159 ) ) ;
#57454 = EDGE_LOOP ( 'NONE', ( #92298, #89944, #75739, #68189 ) ) ;
#57455 = CARTESIAN_POINT ( 'NONE',  ( -52.15869887680651829, -271.8628675873937937, -196.6161525834573069 ) ) ;
#57456 = CARTESIAN_POINT ( 'NONE',  ( 12.85337300930843796, -292.7655053564891432, -327.7625101204392308 ) ) ;
#57457 = CARTESIAN_POINT ( 'NONE',  ( 20.87660219277669071, -288.4418524621688675, -225.1799600806849071 ) ) ;
#57458 = CARTESIAN_POINT ( 'NONE',  ( 35.32491623878451037, -283.1285609269580732, -256.2396718144761962 ) ) ;
#57459 = CARTESIAN_POINT ( 'NONE',  ( -3.306755722038154932, -290.0368838014886137, -338.7878341351317886 ) ) ;
#57460 = CARTESIAN_POINT ( 'NONE',  ( 19.27068535932135518, -289.5713675161308061, -321.8426233913722854 ) ) ;
#57461 = CARTESIAN_POINT ( 'NONE',  ( -38.90182529045613080, -285.0718496041399703, -345.3577273792831761 ) ) ;
#57462 = CARTESIAN_POINT ( 'NONE',  ( -77.81309571363084387, -277.7461388081583777, -335.9293076122339698 ) ) ;
#57463 = ORIENTED_EDGE ( 'NONE', *, *, #17448, .F. ) ;
#57464 = CARTESIAN_POINT ( 'NONE',  ( 35.69820681772038995, -291.8788896556168311, -289.7127637497367800 ) ) ;
#57465 = CARTESIAN_POINT ( 'NONE',  ( 34.58674983517818191, -281.7334086162607036, -297.8438050850731429 ) ) ;
#57466 = CARTESIAN_POINT ( 'NONE',  ( -110.8086392094458148, -274.5553242645343062, -259.3566200948133087 ) ) ;
#57467 = CARTESIAN_POINT ( 'NONE',  ( -20.19161114001083490, -297.3376638359846424, -345.3538533559490702 ) ) ;
#57468 = EDGE_CURVE ( 'NONE', #13227, #23700, #30479, .T. ) ;
#57469 = CARTESIAN_POINT ( 'NONE',  ( 33.78127118843386256, -273.4491020623128179, -243.6123429966363290 ) ) ;
#57470 = CARTESIAN_POINT ( 'NONE',  ( 170.7304434856092143, 250.5000000000000568, -24.91818181818181088 ) ) ;
#57471 = CARTESIAN_POINT ( 'NONE',  ( -38.34840713683026081, -279.5468517500289636, -197.2941042146621555 ) ) ;
#57472 = CARTESIAN_POINT ( 'NONE',  ( 38.92044695501905238, -276.6597244229483294, -262.6052091167042590 ) ) ;
#57473 = AXIS2_PLACEMENT_3D ( 'NONE', #3312, #47791, #32201 ) ;
#57474 = CARTESIAN_POINT ( 'NONE',  ( -67.07391652680202299, -299.0798773384724427, -203.0318728111311657 ) ) ;
#57475 = CARTESIAN_POINT ( 'NONE',  ( -102.7239680373683939, -283.0835743896361123, -310.5852308455691855 ) ) ;
#57476 = CARTESIAN_POINT ( 'NONE',  ( -97.59924262571209397, -292.9055114984050761, -227.2976267820473311 ) ) ;
#57477 = CARTESIAN_POINT ( 'NONE',  ( -8.017483454247686936, -276.0299203628094347, -199.9735394664015473 ) ) ;
#57478 = CARTESIAN_POINT ( 'NONE',  ( 75.64300948861529150, -300.6422523422198765, -193.7355811110692514 ) ) ;
#57479 = CARTESIAN_POINT ( 'NONE',  ( 0.1828843131839977265, -296.5518716174549354, -335.1654164980282076 ) ) ;
#57480 = CARTESIAN_POINT ( 'NONE',  ( -21.01236473298763840, -280.8421099590888730, -343.4444356548648329 ) ) ;
#57481 = CARTESIAN_POINT ( 'NONE',  ( -104.5894439127878286, -290.7046806034951487, -232.8979994883202096 ) ) ;
#57482 = CARTESIAN_POINT ( 'NONE',  ( 28.19914733018943309, -274.0504545713945959, -306.1936657736611664 ) ) ;
#57483 = CARTESIAN_POINT ( 'NONE',  ( 21.45970611976892428, -288.4942443646540937, -221.8963365288080070 ) ) ;
#57484 = CARTESIAN_POINT ( 'NONE',  ( -55.07387260789974448, -290.7390208761353847, -199.2288740154367304 ) ) ;
#57485 = VERTEX_POINT ( 'NONE', #74689 ) ;
#57486 = CARTESIAN_POINT ( 'NONE',  ( -102.7023446523637062, -289.6486321728741586, -230.6789404729901491 ) ) ;
#57487 = CARTESIAN_POINT ( 'NONE',  ( -94.96987217696947425, -289.5870084009867469, -315.2264019682011735 ) ) ;
#57488 = VERTEX_POINT ( 'NONE', #2721 ) ;
#57489 = CARTESIAN_POINT ( 'NONE',  ( -33.75559207112330995, -287.1759547169260145, -193.7541186985337163 ) ) ;
#57490 = CARTESIAN_POINT ( 'NONE',  ( -70.45859756778790484, -277.8346326625081701, -335.4407506707237872 ) ) ;
#57491 = CARTESIAN_POINT ( 'NONE',  ( 38.29911383466275510, -292.6322949907391830, -283.0881241972736007 ) ) ;
#57492 = CARTESIAN_POINT ( 'NONE',  ( -69.13672567637179611, -284.1108815746687242, -340.3925753331854480 ) ) ;
#57493 = CARTESIAN_POINT ( 'NONE',  ( -68.49609166267092064, -285.9871739795202643, -199.9539318047604581 ) ) ;
#57494 = CARTESIAN_POINT ( 'NONE',  ( -39.70616826000728850, -280.3549584877739562, -197.3657419946568155 ) ) ;
#57495 = CARTESIAN_POINT ( 'NONE',  ( 189.8312124288175085, 271.3805950635771751, -139.6404239813599304 ) ) ;
#57496 = CARTESIAN_POINT ( 'NONE',  ( -40.70455346190973955, -139.0725253683308722, -363.9141075947721902 ) ) ;
#57497 = CARTESIAN_POINT ( 'NONE',  ( -112.4672374317974288, -270.5562577345839941, -270.3357054654630360 ) ) ;
#57498 = CARTESIAN_POINT ( 'NONE',  ( -110.3491504304166284, -271.8213126082049484, -264.8912199137930088 ) ) ;
#57499 = CARTESIAN_POINT ( 'NONE',  ( 13.72178132048049548, -273.7089601221063617, -217.7612421696789795 ) ) ;
#57500 = CARTESIAN_POINT ( 'NONE',  ( -77.05584084700134895, -295.0765672385900302, -336.3193379948940560 ) ) ;
#57501 = CARTESIAN_POINT ( 'NONE',  ( 203.3291423003342402, 291.9839310567934376, -68.27044577648942436 ) ) ;
#57502 = CARTESIAN_POINT ( 'NONE',  ( -78.56167357764061876, -272.1943012040609915, -205.9079407074285086 ) ) ;
#57503 = CARTESIAN_POINT ( 'NONE',  ( -67.33984280108882103, -299.5149506334882972, -202.4430297835519923 ) ) ;
#57504 = CARTESIAN_POINT ( 'NONE',  ( -13.10958062581066663, -290.0457929119829714, -339.7444579282480390 ) ) ;
#57505 = CARTESIAN_POINT ( 'NONE',  ( -32.14905656049183591, -293.1988296695339500, -197.2234654142295653 ) ) ;
#57506 = VERTEX_POINT ( 'NONE', #40073 ) ;
#57507 = CARTESIAN_POINT ( 'NONE',  ( -113.1590559064126182, -297.6452695913094431, -258.2549207732910190 ) ) ;
#57508 = CARTESIAN_POINT ( 'NONE',  ( -68.80711504432673564, -286.1193169480072243, -204.4085862466549202 ) ) ;
#57509 = CARTESIAN_POINT ( 'NONE',  ( -19.31522148232867409, -295.6289003107107192, -345.1099654740436904 ) ) ;
#57510 = CARTESIAN_POINT ( 'NONE',  ( -19.29562548196082261, -295.3184648878237226, -345.2081133636395975 ) ) ;
#57511 = CARTESIAN_POINT ( 'NONE',  ( -7.272185374082278386, -292.6245777682630660, -203.8417652572911436 ) ) ;
#57512 = ORIENTED_EDGE ( 'NONE', *, *, #39378, .F. ) ;
#57513 = CARTESIAN_POINT ( 'NONE',  ( -73.28189792807118863, -275.4999379333262937, -203.8377942409727552 ) ) ;
#57514 = EDGE_CURVE ( 'NONE', #85888, #86239, #75817, .T. ) ;
#57515 = ORIENTED_EDGE ( 'NONE', *, *, #15094, .F. ) ;
#57516 = CARTESIAN_POINT ( 'NONE',  ( -108.4533884341641681, -278.4334072384455681, -240.9901341833195829 ) ) ;
#57517 = CARTESIAN_POINT ( 'NONE',  ( -32.61971085465124531, -272.5124925270429230, -196.6996715409798071 ) ) ;
#57518 = CARTESIAN_POINT ( 'NONE',  ( -35.82054257266347719, -299.2766886233366677, -196.9637219586092272 ) ) ;
#57519 = CARTESIAN_POINT ( 'NONE',  ( 34.06049168239887592, -276.2786328182733655, -254.0221106799102131 ) ) ;
#57520 = CARTESIAN_POINT ( 'NONE',  ( -60.58279208308476882, -275.5150249246643739, -197.9610297328918023 ) ) ;
#57521 = CARTESIAN_POINT ( 'NONE',  ( 35.69734559211168090, -273.3352183382182830, -251.8218459788683674 ) ) ;
#57522 = CARTESIAN_POINT ( 'NONE',  ( -90.47562891886720138, -296.4807032040559989, -320.6403648810660911 ) ) ;
#57523 = CARTESIAN_POINT ( 'NONE',  ( 36.23026466787008104, -292.1683708186756121, -273.5323196196504227 ) ) ;
#57524 = DIRECTION ( 'NONE',  ( 0.000000000000000000, 0.000000000000000000, 1.000000000000000000 ) ) ;
#57525 = CARTESIAN_POINT ( 'NONE',  ( -98.53123169608137744, -279.6669738137275658, -223.6988127938673188 ) ) ;
#57526 = CARTESIAN_POINT ( 'NONE',  ( -19.01489548267566931, -276.9762709553095874, -341.0231886851154286 ) ) ;
#57527 = CARTESIAN_POINT ( 'NONE',  ( 33.40980844623978641, -285.8630855169132019, -241.1104052066764325 ) ) ;
#57528 = CARTESIAN_POINT ( 'NONE',  ( -95.08626478697190976, -297.8890205379088911, -318.5017388261641713 ) ) ;
#57529 = CARTESIAN_POINT ( 'NONE',  ( 82.67955185657098127, -297.1469379644294690, -196.0571845609111676 ) ) ;
#57530 = CARTESIAN_POINT ( 'NONE',  ( 1.388417528942380130, -287.7172745274576187, -332.4302706520730339 ) ) ;
#57531 = CARTESIAN_POINT ( 'NONE',  ( -101.6818008781638270, -277.2862049186804825, -233.7779873481170796 ) ) ;
#57532 = CARTESIAN_POINT ( 'NONE',  ( -105.8227089317481102, -276.7695067987242510, -297.3004266075571422 ) ) ;
#57534 = CARTESIAN_POINT ( 'NONE',  ( -91.20241366768098601, -285.8174500044536330, -322.6261013126309649 ) ) ;
#57533 = VECTOR ( 'NONE', #43911, 1000.000000000000000 ) ;
#57535 = CARTESIAN_POINT ( 'NONE',  ( -1.261726975119667138, -277.7676061218281802, -334.3355042765239205 ) ) ;
#57536 = CARTESIAN_POINT ( 'NONE',  ( 196.7510731661265595, -143.7221692137691775, 22.50000000000000000 ) ) ;
#57537 = CARTESIAN_POINT ( 'NONE',  ( 15.48722516338289701, -273.1841680084531845, -215.4471391912374827 ) ) ;
#57538 = CIRCLE ( 'NONE', #9164, 1.000000000000000888 ) ;
#57539 = CARTESIAN_POINT ( 'NONE',  ( -14.04079314414769541, -275.0139992882502042, -201.0721549237471493 ) ) ;
#57540 = CARTESIAN_POINT ( 'NONE',  ( 19.65880231802498557, -282.8745502591153809, -221.3418491594536022 ) ) ;
#57541 = DIRECTION ( 'NONE',  ( 1.000000000000000000, 0.000000000000000000, 0.000000000000000000 ) ) ;
#57542 = CARTESIAN_POINT ( 'NONE',  ( 37.91799713514392067, -289.3794014643193009, -263.0714025925938699 ) ) ;
#57543 = CARTESIAN_POINT ( 'NONE',  ( 34.12147472795849978, -291.8476754347890392, -293.2889027800566168 ) ) ;
#57544 = CARTESIAN_POINT ( 'NONE',  ( -3.044879762945660762, -290.6499362809184390, -204.5234874394981830 ) ) ;
#57545 = CARTESIAN_POINT ( 'NONE',  ( 197.0349383350915105, 285.8449894349855640, -111.9383547020201064 ) ) ;
#57546 = CARTESIAN_POINT ( 'NONE',  ( 198.5111534495024159, 66.01618214920664229, -10.78140162895428666 ) ) ;
#57547 = CARTESIAN_POINT ( 'NONE',  ( -29.07173506878448421, -287.4291689893769899, -346.2713652077850384 ) ) ;
#57548 = CARTESIAN_POINT ( 'NONE',  ( -113.3421064416752415, -282.7611768888026518, -272.7941257223787375 ) ) ;
#57549 = CARTESIAN_POINT ( 'NONE',  ( 10.30390055809582073, -283.8052355891049388, -326.5108663641944418 ) ) ;
#57550 = CARTESIAN_POINT ( 'NONE',  ( -110.2558626212838249, -285.2758752858072171, -276.3716615982054918 ) ) ;
#57551 = CARTESIAN_POINT ( 'NONE',  ( -39.19702060236851793, -294.0088967395003579, -195.0160007210211006 ) ) ;
#57552 = CARTESIAN_POINT ( 'NONE',  ( -96.01432809815464964, -273.5575610569894707, -220.5084318510457706 ) ) ;
#57553 = CARTESIAN_POINT ( 'NONE',  ( -94.38751466024767467, -287.9495505450739756, -319.9099751280563737 ) ) ;
#57554 = CARTESIAN_POINT ( 'NONE',  ( -11.86618473281223984, -276.7296215459751352, -343.0806402270740136 ) ) ;
#57555 = CARTESIAN_POINT ( 'NONE',  ( 35.55064936178566626, -295.3238391607541757, -254.2225455095673965 ) ) ;
#57556 = CARTESIAN_POINT ( 'NONE',  ( 85.55100297371609486, -298.0521521680024080, -517.1711561948568487 ) ) ;
#57557 = CARTESIAN_POINT ( 'NONE',  ( 21.27581636871892101, -295.4090924074130839, -223.5744983911110353 ) ) ;
#57558 = CARTESIAN_POINT ( 'NONE',  ( -96.15056012248865613, -283.8515532328726181, -226.2843501182847490 ) ) ;
#57559 = ADVANCED_FACE ( 'NONE', ( #89804 ), #24482, .F. ) ;
#57560 = CARTESIAN_POINT ( 'NONE',  ( -93.44824617194852578, -277.2443382491358079, -220.5910854179329021 ) ) ;
#57561 = EDGE_CURVE ( 'NONE', #49742, #73850, #75613, .T. ) ;
#57562 = CARTESIAN_POINT ( 'NONE',  ( -23.51977760728848565, -296.6223423666537542, -194.1648020273771920 ) ) ;
#57563 = CARTESIAN_POINT ( 'NONE',  ( 35.48054327527929530, -274.8092888467007811, -263.4193056203586139 ) ) ;
#57564 = CARTESIAN_POINT ( 'NONE',  ( 31.46893760137199791, -294.7232905918149299, -243.9830231589062919 ) ) ;
#57565 = CARTESIAN_POINT ( 'NONE',  ( 15.03543220320434060, -293.7544863068172276, -219.1021266316067511 ) ) ;
#57566 = CARTESIAN_POINT ( 'NONE',  ( -110.7375220870011674, -297.5941631761612598, -292.0024666298239708 ) ) ;
#57567 = CARTESIAN_POINT ( 'NONE',  ( -108.5923327975898189, -296.1759162869379907, -286.2465625383132988 ) ) ;
#57568 = CARTESIAN_POINT ( 'NONE',  ( -107.9058994637561426, -292.2229007728791998, -295.7716358734990081 ) ) ;
#57569 = CARTESIAN_POINT ( 'NONE',  ( -58.48471078639734344, -283.4847068076434198, -344.4569637422487176 ) ) ;
#57570 = CARTESIAN_POINT ( 'NONE',  ( -34.13143451227233527, -272.2317130023740219, -194.6643566445341378 ) ) ;
#57571 = CARTESIAN_POINT ( 'NONE',  ( -12.70170037734914459, -286.1971713319660466, -197.4099670884224338 ) ) ;
#57572 = CARTESIAN_POINT ( 'NONE',  ( -109.7618603081762956, -280.2979932529585767, -288.5015011253096873 ) ) ;
#57573 = CARTESIAN_POINT ( 'NONE',  ( -99.80375660342556898, -284.1372199172582214, -232.0297216355389196 ) ) ;
#57574 = CARTESIAN_POINT ( 'NONE',  ( -67.27956021383455720, -287.4445661254218862, -339.1268448000188300 ) ) ;
#57575 = CARTESIAN_POINT ( 'NONE',  ( 0.9968329295543288948, -56.25428601379442028, -352.6033083298257225 ) ) ;
#57576 = CARTESIAN_POINT ( 'NONE',  ( 33.09025846622809297, -286.8033436812949049, -250.9361945500980937 ) ) ;
#57577 = CARTESIAN_POINT ( 'NONE',  ( 31.65710497515726018, -282.3267508583586505, -236.9649168505702050 ) ) ;
#57578 = CARTESIAN_POINT ( 'NONE',  ( -38.92736724058741515, -288.1303435202926266, -347.1094461313792294 ) ) ;
#57579 = CARTESIAN_POINT ( 'NONE',  ( -86.30641667149771479, -280.9862158008576216, -211.9065678579501082 ) ) ;
#57580 = CARTESIAN_POINT ( 'NONE',  ( -79.65209336095861659, -280.8088368804564539, -206.5548815688834736 ) ) ;
#57581 = CARTESIAN_POINT ( 'NONE',  ( -100.8107603293378105, -278.8794095190371536, -234.2961987166378037 ) ) ;
#57582 = CARTESIAN_POINT ( 'NONE',  ( -65.20566783748141404, -275.6661365040711758, -201.0981725180516548 ) ) ;
#57583 = CARTESIAN_POINT ( 'NONE',  ( 38.85189671985328630, -293.4086737227804633, -258.8886978729627231 ) ) ;
#57584 = CARTESIAN_POINT ( 'NONE',  ( 24.86663278337135097, -286.1324089665666293, -311.6393937252423143 ) ) ;
#57585 = CARTESIAN_POINT ( 'NONE',  ( -7.522245727649240266, -294.0367257180901674, -200.2239083111984712 ) ) ;
#57586 = CARTESIAN_POINT ( 'NONE',  ( -92.06652339558283415, -296.1670981600845494, -221.5818212222534953 ) ) ;
#57587 = CARTESIAN_POINT ( 'NONE',  ( -61.98888978234186453, -285.2950950539051291, -340.6566255807605330 ) ) ;
#57588 = CARTESIAN_POINT ( 'NONE',  ( -103.9576467496765844, -295.8146593540945446, -300.3913091889525617 ) ) ;
#57589 = CARTESIAN_POINT ( 'NONE',  ( 3.963421869051978685, -293.6738002830130654, -205.6810023701736156 ) ) ;
#57590 = CARTESIAN_POINT ( 'NONE',  ( -19.51771992270131761, -280.9387964671371378, -199.4130698934563952 ) ) ;
#57591 = CARTESIAN_POINT ( 'NONE',  ( 35.51047184528718503, -274.3035095503947787, -245.9988246046506504 ) ) ;
#57592 = CARTESIAN_POINT ( 'NONE',  ( -102.2108058144700209, -290.6604256641449524, -311.7545139252495687 ) ) ;
#57593 = CARTESIAN_POINT ( 'NONE',  ( -31.75145080200277192, -281.1219192954770847, -345.9324591248744696 ) ) ;
#57594 = CARTESIAN_POINT ( 'NONE',  ( -106.4926509162334014, -290.4496337232558290, -304.3037160059258781 ) ) ;
#57595 = CARTESIAN_POINT ( 'NONE',  ( 34.01576570316509418, -287.6810441981606346, -254.8627452610713249 ) ) ;
#57596 = FACE_OUTER_BOUND ( 'NONE', #21508, .T. ) ;
#57597 = CARTESIAN_POINT ( 'NONE',  ( 63.26945853893380445, 48.02268529798013219, -317.1124933380390871 ) ) ;
#57598 = CARTESIAN_POINT ( 'NONE',  ( 188.3815699774405914, 268.4127512313500006, -137.5006950848226097 ) ) ;
#57599 = CIRCLE ( 'NONE', #12161, 1.000000000000000888 ) ;
#57600 = CARTESIAN_POINT ( 'NONE',  ( -107.9788296581491238, -277.4982106727002247, -289.4136154328065231 ) ) ;
#57601 = EDGE_LOOP ( 'NONE', ( #65563, #58869 ) ) ;
#57602 = CARTESIAN_POINT ( 'NONE',  ( -5.411485193063779064, -279.4027938030335463, -204.3710623003073579 ) ) ;
#57603 = CARTESIAN_POINT ( 'NONE',  ( -15.77921187233445188, -273.9902756953135849, -196.4085443027745441 ) ) ;
#57604 = CARTESIAN_POINT ( 'NONE',  ( 162.4344822024288248, 217.7039127420125055, -203.2254006442507546 ) ) ;
#57605 = CARTESIAN_POINT ( 'NONE',  ( -90.63410881575923383, -277.8897790276416799, -215.5285787958924288 ) ) ;
#57606 = CARTESIAN_POINT ( 'NONE',  ( -43.08405447717554182, -281.1449700493054138, -344.8359323433271584 ) ) ;
#57607 = CARTESIAN_POINT ( 'NONE',  ( -99.11106645259468451, -298.9065216928514133, -226.1059555853186112 ) ) ;
#57608 = CARTESIAN_POINT ( 'NONE',  ( -92.60715282538144777, -291.7248562719928486, -222.5728539424964367 ) ) ;
#57609 = CARTESIAN_POINT ( 'NONE',  ( 19.88702626850750121, -286.8845445538771060, -316.4709472460172606 ) ) ;
#57610 = CARTESIAN_POINT ( 'NONE',  ( 29.85441887773816205, -275.7170070474711565, -232.8618800972456313 ) ) ;
#57611 = CARTESIAN_POINT ( 'NONE',  ( -81.07100676322005484, -273.4395754160483420, -211.8447354645772975 ) ) ;
#57612 = ORIENTED_EDGE ( 'NONE', *, *, #59748, .T. ) ;
#57613 = CARTESIAN_POINT ( 'NONE',  ( 165.2688068684385883, 250.0000000000000568, 21.83530662808711398 ) ) ;
#57614 = DIRECTION ( 'NONE',  ( 0.000000000000000000, 0.000000000000000000, -1.000000000000000000 ) ) ;
#57615 = CARTESIAN_POINT ( 'NONE',  ( -96.58341530287106025, -281.1118303149219173, -223.4598025867872195 ) ) ;
#57616 = CARTESIAN_POINT ( 'NONE',  ( 155.8109286537083733, 19.19772955881940391, 9.232252220100694018 ) ) ;
#57617 = CARTESIAN_POINT ( 'NONE',  ( -4.220160341655663672, -281.5790929561746907, -204.9469422431492092 ) ) ;
#57618 = CARTESIAN_POINT ( 'NONE',  ( -73.30608116431800170, -281.3421103969245110, -203.4095462067143103 ) ) ;
#57619 = CARTESIAN_POINT ( 'NONE',  ( -85.02402419621715524, -282.7882321303009689, -325.9471271835198536 ) ) ;
#57620 = CARTESIAN_POINT ( 'NONE',  ( -108.2902308738619865, -280.1260134859790583, -292.3773211751072267 ) ) ;
#57621 = CARTESIAN_POINT ( 'NONE',  ( -33.98995736025342751, -272.5749491994733376, -196.7440440525120664 ) ) ;
#57622 = CARTESIAN_POINT ( 'NONE',  ( 0.000000000000000000, 0.000000000000000000, -7.500000000000000000 ) ) ;
#57623 = CARTESIAN_POINT ( 'NONE',  ( 188.7149167944524493, -12.49482340714361506, 9.974999999999996092 ) ) ;
#57624 = CARTESIAN_POINT ( 'NONE',  ( -5.342680378161870358, -277.4445369737171632, -340.2197005346345122 ) ) ;
#57625 = CARTESIAN_POINT ( 'NONE',  ( -47.80257052418233599, -229.5268262511776527, 22.50000000000000000 ) ) ;
#57626 = CARTESIAN_POINT ( 'NONE',  ( -77.52063042724746822, -276.1544430970827761, -335.4169187851539391 ) ) ;
#57627 = ORIENTED_EDGE ( 'NONE', *, *, #34351, .T. ) ;
#57628 = DIRECTION ( 'NONE',  ( -1.000000000000000000, 0.000000000000000000, 0.000000000000000000 ) ) ;
#57629 = CARTESIAN_POINT ( 'NONE',  ( -65.92841814486052954, -285.4041819847944907, -340.0973504368578801 ) ) ;
#57630 = CARTESIAN_POINT ( 'NONE',  ( 20.64494854287097425, -293.3760144242928618, -314.9927269770820430 ) ) ;
#57631 = CARTESIAN_POINT ( 'NONE',  ( 38.57299032387706461, -287.0583064800667330, -282.9432084051824177 ) ) ;
#57632 = CARTESIAN_POINT ( 'NONE',  ( -71.62801043384467903, -283.8324818411110755, -204.7682605885046314 ) ) ;
#57634 = CARTESIAN_POINT ( 'NONE',  ( -0.5063166204722437946, -286.7956963449546492, -334.6161180392822416 ) ) ;
#57633 = CARTESIAN_POINT ( 'NONE',  ( -109.7697552912194112, -283.2981983729380318, -257.2691202428175075 ) ) ;
#57635 = CARTESIAN_POINT ( 'NONE',  ( 35.82618576950239486, -282.8413288285244676, -276.7706258523944030 ) ) ;
#57636 = CARTESIAN_POINT ( 'NONE',  ( -60.23573534587868750, -271.7553288428964606, -198.8866080079085066 ) ) ;
#57637 = CARTESIAN_POINT ( 'NONE',  ( -100.7647246949549498, -282.3892267799135993, -312.6927860890463649 ) ) ;
#57638 = CARTESIAN_POINT ( 'NONE',  ( -112.3383107573079798, -298.5614778680699146, -269.6476477581690574 ) ) ;
#57639 = CARTESIAN_POINT ( 'NONE',  ( -3.036338252101231650, -284.5041144381829099, -203.4649488932181782 ) ) ;
#57640 = CARTESIAN_POINT ( 'NONE',  ( -110.2014851540139517, -279.5972040903377547, -262.4675300087862411 ) ) ;
#57641 = CARTESIAN_POINT ( 'NONE',  ( -0.6343007329302595698, -288.5387744382253459, -204.7522600594095081 ) ) ;
#57642 = CARTESIAN_POINT ( 'NONE',  ( 195.8262106289358258, 26.26158389346358746, 13.54803344068640314 ) ) ;
#57643 = DIRECTION ( 'NONE',  ( -0.000000000000000000, -1.000000000000000000, -0.000000000000000000 ) ) ;
#57644 = CARTESIAN_POINT ( 'NONE',  ( 16.44701099991650395, -294.7288609567850131, -217.2206352423231408 ) ) ;
#57645 = CARTESIAN_POINT ( 'NONE',  ( -110.5536585615042071, -276.7617036329259577, -254.0232976385879340 ) ) ;
#57646 = CARTESIAN_POINT ( 'NONE',  ( -105.0185882149049661, -289.2778948186726211, -306.7478963356214194 ) ) ;
#57647 = CARTESIAN_POINT ( 'NONE',  ( 30.21428099867172534, -292.3473855861907964, -300.0702045916698921 ) ) ;
#57648 = CARTESIAN_POINT ( 'NONE',  ( -74.74242456649125188, -278.2282962507962338, -207.0378750661772358 ) ) ;
#57649 = CARTESIAN_POINT ( 'NONE',  ( -60.88556721353560164, -295.8830671455014567, -199.9039678419400445 ) ) ;
#57650 = CARTESIAN_POINT ( 'NONE',  ( -94.68615157272625993, -292.5127691080730870, -224.3752867370811828 ) ) ;
#57651 = CARTESIAN_POINT ( 'NONE',  ( 39.58706461736020543, -278.0519495502701943, -270.3284710469133074 ) ) ;
#57652 = CARTESIAN_POINT ( 'NONE',  ( 0.1825307035090767416, -293.0418556664899938, -336.8189151771805996 ) ) ;
#57653 = CARTESIAN_POINT ( 'NONE',  ( -5.428240273270160898, -290.2252231001308473, -336.9041228582225358 ) ) ;
#57654 = CARTESIAN_POINT ( 'NONE',  ( 22.32648821661240035, -291.1541520665195435, -223.2905424537789827 ) ) ;
#57655 = CARTESIAN_POINT ( 'NONE',  ( 23.24525375620302725, -289.5547145105940672, -312.1516973993332158 ) ) ;
#57656 = CYLINDRICAL_SURFACE ( 'NONE', #3297, 2.000000000000000000 ) ;
#57657 = CARTESIAN_POINT ( 'NONE',  ( -80.49452319113039778, -290.4565588084187198, -329.5040613568885419 ) ) ;
#57658 = LINE ( 'NONE', #20274, #85297 ) ;
#57659 = ADVANCED_BREP_SHAPE_REPRESENTATION ( '', ( #26626, #27724, #18940 ), #37050 ) ;
#57660 = CARTESIAN_POINT ( 'NONE',  ( -54.39819252439830422, -290.4714984615385447, -345.0954274552201468 ) ) ;
#57662 = CARTESIAN_POINT ( 'NONE',  ( -96.76136113481905454, -291.1456545598753110, -227.8692024489122048 ) ) ;
#57661 = CARTESIAN_POINT ( 'NONE',  ( 11.93602529117274003, -278.7532210193863307, -213.3513593664415282 ) ) ;
#57663 = CARTESIAN_POINT ( 'NONE',  ( -31.07971276210952638, -280.4623679564709278, -193.5847048088081124 ) ) ;
#57664 = VECTOR ( 'NONE', #59793, 1000.000000000000000 ) ;
#57665 = CARTESIAN_POINT ( 'NONE',  ( 36.58060354450348228, -280.9489441826681286, -248.8374167656960196 ) ) ;
#57666 = CARTESIAN_POINT ( 'NONE',  ( 14.54099637844502624, -284.7815316527086793, -216.1305425700780347 ) ) ;
#57667 = DIRECTION ( 'NONE',  ( -1.000000000000000000, 0.000000000000000000, 0.000000000000000000 ) ) ;
#57668 = CARTESIAN_POINT ( 'NONE',  ( 4.059782309532352862, -280.6278472192745994, -332.0413240862674229 ) ) ;
#57669 = EDGE_CURVE ( 'NONE', #65802, #56772, #51611, .T. ) ;
#57670 = CARTESIAN_POINT ( 'NONE',  ( -49.00783483711197164, -283.9034929596534766, -196.2216557077590551 ) ) ;
#57671 = CARTESIAN_POINT ( 'NONE',  ( 202.9739431621297854, 291.9636489107636521, -68.24819746054791381 ) ) ;
#57672 = CARTESIAN_POINT ( 'NONE',  ( -94.43010240320995763, -277.7242992126917898, -219.7288942586965845 ) ) ;
#57673 = CARTESIAN_POINT ( 'NONE',  ( -80.75186664459556596, -284.3989256426984866, -207.0747983761724527 ) ) ;
#57674 = CARTESIAN_POINT ( 'NONE',  ( -44.60430831433531296, -298.8993966867382142, -197.4362778230943150 ) ) ;
#57675 = LINE ( 'NONE', #2585, #14074 ) ;
#57676 = CARTESIAN_POINT ( 'NONE',  ( -109.4969901315334084, -292.3544543350430445, -254.8674243629021703 ) ) ;
#57677 = CARTESIAN_POINT ( 'NONE',  ( 24.83677692059092834, -276.3843068797114597, -225.9265440971653049 ) ) ;
#57678 = CARTESIAN_POINT ( 'NONE',  ( 23.99984261568192778, -275.7682446408014130, -310.0687669069876620 ) ) ;
#57679 = CARTESIAN_POINT ( 'NONE',  ( 11.61579823217088325, -296.3728436956533869, -327.1780520793758456 ) ) ;
#57680 = CARTESIAN_POINT ( 'NONE',  ( -54.49954988508929432, -289.4332698593926239, -345.4798568130370313 ) ) ;
#57681 = CARTESIAN_POINT ( 'NONE',  ( 25.51024815650696098, -280.1945943937059269, -312.3009176333296750 ) ) ;
#57682 = CARTESIAN_POINT ( 'NONE',  ( 24.81570823793426328, -292.7820934494729386, -224.9138233464549899 ) ) ;
#57683 = CARTESIAN_POINT ( 'NONE',  ( -22.68185010900764098, -291.3031649485820935, -198.6080884659516528 ) ) ;
#57684 = CARTESIAN_POINT ( 'NONE',  ( -80.73583205035789945, -293.6402437740788400, -331.5960433192204846 ) ) ;
#57685 = EDGE_LOOP ( 'NONE', ( #90605, #46390, #17638, #46250, #77406 ) ) ;
#57686 = CARTESIAN_POINT ( 'NONE',  ( 200.5815643859950512, 65.97596549932490007, 9.780880230328994784 ) ) ;
#57687 = CARTESIAN_POINT ( 'NONE',  ( -20.05152557198974961, -291.7879154240641810, -199.3226196073275389 ) ) ;
#57688 = DIRECTION ( 'NONE',  ( -0.000000000000000000, -1.000000000000000000, -0.000000000000000000 ) ) ;
#57689 = CARTESIAN_POINT ( 'NONE',  ( 7.399455738971487229, -273.9094976428776818, -326.5171145203363494 ) ) ;
#57690 = CARTESIAN_POINT ( 'NONE',  ( -110.5789246492023636, -295.3204737289673858, -293.4079454594493654 ) ) ;
#57691 = CARTESIAN_POINT ( 'NONE',  ( -70.24276363978646032, -284.7917795042565103, -339.4465961953549140 ) ) ;
#57692 = CARTESIAN_POINT ( 'NONE',  ( -79.30754879394638124, -285.3015876465173051, -210.5674323561158303 ) ) ;
#57693 = CARTESIAN_POINT ( 'NONE',  ( 17.96830438507194216, -277.7612621640561201, -319.0783250915033591 ) ) ;
#57694 = CARTESIAN_POINT ( 'NONE',  ( 20.96305535833123912, -292.2163899682133774, -316.9905213263956512 ) ) ;
#57695 = CARTESIAN_POINT ( 'NONE',  ( 34.76771298962304257, -295.5299694093850462, -287.0965520938358964 ) ) ;
#57696 = CARTESIAN_POINT ( 'NONE',  ( -4.904341022967168229, -275.4101915475108058, -336.2154066289202774 ) ) ;
#57697 = ORIENTED_EDGE ( 'NONE', *, *, #48992, .F. ) ;
#57698 = CARTESIAN_POINT ( 'NONE',  ( 195.8598878520694200, 40.68233701717534956, 13.45727524496615324 ) ) ;
#57699 = CARTESIAN_POINT ( 'NONE',  ( 37.07503850517524313, -293.4655059971601645, -290.0561250347504370 ) ) ;
#57700 = CARTESIAN_POINT ( 'NONE',  ( 15.11513296530155337, -290.2249039928973957, -323.1777333471455904 ) ) ;
#57701 = DIRECTION ( 'NONE',  ( -0.000000000000000000, -0.000000000000000000, 1.000000000000000000 ) ) ;
#57702 = CARTESIAN_POINT ( 'NONE',  ( -97.51076072415143869, -274.3945810059534551, -222.9512786293650777 ) ) ;
#57703 = CARTESIAN_POINT ( 'NONE',  ( 6.982152532026011826, -287.3249466757657160, -212.1655164235480981 ) ) ;
#57704 = EDGE_LOOP ( 'NONE', ( #43004, #70659, #54309, #18591 ) ) ;
#57705 = CARTESIAN_POINT ( 'NONE',  ( -96.62803972800544727, -278.2681686192193524, -221.5764506891514714 ) ) ;
#57706 = CARTESIAN_POINT ( 'NONE',  ( 22.21296548495133649, -294.8576103732307843, -319.0290388311582319 ) ) ;
#57707 = CARTESIAN_POINT ( 'NONE',  ( -26.34757877042141772, -287.0532333732097072, -345.3240072952887090 ) ) ;
#57708 = CARTESIAN_POINT ( 'NONE',  ( -50.45974191532993558, -295.5484066936854788, -346.2679400626686288 ) ) ;
#57709 = CARTESIAN_POINT ( 'NONE',  ( 18.49001247015401006, -293.2169807820790197, -223.2983157370485117 ) ) ;
#57710 = FACE_OUTER_BOUND ( 'NONE', #89350, .T. ) ;
#57711 = FACE_OUTER_BOUND ( 'NONE', #17636, .T. ) ;
#57712 = CARTESIAN_POINT ( 'NONE',  ( 139.4823848151520735, 130.0000000000000568, -12.50000000000000000 ) ) ;
#57713 = CARTESIAN_POINT ( 'NONE',  ( -7.631111581328803517, -287.9545692886845814, -200.0199270819602191 ) ) ;
#57714 = CARTESIAN_POINT ( 'NONE',  ( -2.602324593224659921, -283.9809262143061233, -198.2974183793908196 ) ) ;
#57715 = ORIENTED_EDGE ( 'NONE', *, *, #47694, .F. ) ;
#57716 = CARTESIAN_POINT ( 'NONE',  ( -71.18225273169647949, -278.9657088200427779, -201.3094721902065487 ) ) ;
#57717 = CARTESIAN_POINT ( 'NONE',  ( 4.434289685649758006, -284.4878019350697400, -332.5108090149890927 ) ) ;
#57718 = CARTESIAN_POINT ( 'NONE',  ( -60.31533853284810220, -284.3348481670145134, -197.4306112188495206 ) ) ;
#57719 = CARTESIAN_POINT ( 'NONE',  ( 28.28873286595062453, -286.1028890882653286, -305.5985316601507975 ) ) ;
#57720 = CARTESIAN_POINT ( 'NONE',  ( -3.259187464325852268, -278.4673666485829244, -338.0415642729728916 ) ) ;
#57721 = CARTESIAN_POINT ( 'NONE',  ( -102.0511510180885324, -273.3470576681523880, -236.4170738947551058 ) ) ;
#57722 = ORIENTED_EDGE ( 'NONE', *, *, #34673, .T. ) ;
#57723 = CARTESIAN_POINT ( 'NONE',  ( 20.06856784116714820, -292.8810005181583733, -316.2647719631617633 ) ) ;
#57725 = CARTESIAN_POINT ( 'NONE',  ( -64.84678789747771077, -279.0317420668911268, -202.6310447866929962 ) ) ;
#57724 = CARTESIAN_POINT ( 'NONE',  ( -109.1321013365486721, -278.7267303806183349, -257.1271354252457968 ) ) ;
#57726 = CARTESIAN_POINT ( 'NONE',  ( -10.46886258239271861, -275.4742251133558852, -198.4760590332703600 ) ) ;
#57727 = CARTESIAN_POINT ( 'NONE',  ( -112.9099897138440411, -277.1893420362796974, -282.9087204638536832 ) ) ;
#57728 = CARTESIAN_POINT ( 'NONE',  ( 187.5403984051958730, 270.4479071988321266, -138.3868815421773490 ) ) ;
#57729 = CARTESIAN_POINT ( 'NONE',  ( -113.0661588182869934, -297.8437671998181600, -280.9662061453626052 ) ) ;
#57730 = CARTESIAN_POINT ( 'NONE',  ( 10.59707575819634329, -277.1948066931274184, -210.1954327657594490 ) ) ;
#57731 = CIRCLE ( 'NONE', #86419, 6.000000000000005329 ) ;
#57732 = CARTESIAN_POINT ( 'NONE',  ( 82.67702266595013327, -297.3455801312759377, -194.1454284809947524 ) ) ;
#57733 = CIRCLE ( 'NONE', #81829, 4.499999999999993783 ) ;
#57734 = CARTESIAN_POINT ( 'NONE',  ( -85.94131213312373063, -286.4399162487915760, -215.4087993453869956 ) ) ;
#57735 = CARTESIAN_POINT ( 'NONE',  ( -84.89641334288039332, -287.1665508542258749, -211.0945737747394730 ) ) ;
#57736 = CARTESIAN_POINT ( 'NONE',  ( -15.82956068846278264, -288.1151215027998092, -340.2790312140961078 ) ) ;
#57737 = CARTESIAN_POINT ( 'NONE',  ( -105.3747458795350269, -284.5253879910842443, -234.3161349197571326 ) ) ;
#57738 = CARTESIAN_POINT ( 'NONE',  ( 3.159868899270529496, -279.0056476542673067, -208.6064873102757531 ) ) ;
#57739 = CARTESIAN_POINT ( 'NONE',  ( -72.98759480476644512, -287.4349761001529941, -205.2295667998179738 ) ) ;
#57740 = CARTESIAN_POINT ( 'NONE',  ( 34.90661833087635557, -280.2226230419719855, -284.9465326302661197 ) ) ;
#57741 = CARTESIAN_POINT ( 'NONE',  ( -73.06717479543813454, -278.8513544616861282, -334.6012439097072502 ) ) ;
#57742 = CARTESIAN_POINT ( 'NONE',  ( 33.95469671935499179, -276.2556496899053400, -286.3808676455569753 ) ) ;
#57743 = CARTESIAN_POINT ( 'NONE',  ( -59.92493121506618081, -288.1333826715351165, -343.5595222778960647 ) ) ;
#57744 = CIRCLE ( 'NONE', #32032, 4.999999999999985789 ) ;
#57745 = CARTESIAN_POINT ( 'NONE',  ( -69.11033991755203942, -284.2622764521086083, -340.3391509866131059 ) ) ;
#57746 = CARTESIAN_POINT ( 'NONE',  ( -2.914747351707708489, -283.1018153499184677, -339.1820956484730800 ) ) ;
#57747 = VERTEX_POINT ( 'NONE', #47656 ) ;
#57748 = VERTEX_POINT ( 'NONE', #82708 ) ;
#57749 = CARTESIAN_POINT ( 'NONE',  ( 4.888799411908724579, -290.3485496442762042, -333.2649365250067035 ) ) ;
#57750 = EDGE_CURVE ( 'NONE', #75426, #46169, #211, .T. ) ;
#57751 = CARTESIAN_POINT ( 'NONE',  ( -111.8332570173745779, -289.4565636170700031, -252.9167427499722294 ) ) ;
#57752 = CARTESIAN_POINT ( 'NONE',  ( -107.4181753083423132, -271.8937865218068737, -248.9108431243769530 ) ) ;
#57753 = CARTESIAN_POINT ( 'NONE',  ( 32.09749340807007201, -292.4753092350247243, -237.1993157039026698 ) ) ;
#57754 = CARTESIAN_POINT ( 'NONE',  ( -110.9368534842396912, -289.0932929339947464, -265.6723955499365957 ) ) ;
#57755 = CARTESIAN_POINT ( 'NONE',  ( 29.29729805209579041, -292.2232980844642611, -302.6851045285180248 ) ) ;
#57756 = CARTESIAN_POINT ( 'NONE',  ( 34.95582976941094699, -288.5874122432589388, -257.4178429492077385 ) ) ;
#57757 = CARTESIAN_POINT ( 'NONE',  ( 31.98288692825981272, -290.4805209788416391, -303.7098442033569654 ) ) ;
#57758 = CARTESIAN_POINT ( 'NONE',  ( -12.85207459233313720, -290.7341651388443893, -341.3046064698045825 ) ) ;
#57759 = CARTESIAN_POINT ( 'NONE',  ( -112.4213510695021938, -288.5056641635710548, -273.9769772615578631 ) ) ;
#57760 = CARTESIAN_POINT ( 'NONE',  ( -7.664778281854705000, -294.4412563172717796, -201.4686707104418701 ) ) ;
#57761 = CARTESIAN_POINT ( 'NONE',  ( -109.2080877495406952, -285.3080857496458975, -284.4547611934959264 ) ) ;
#57762 = CARTESIAN_POINT ( 'NONE',  ( -40.57956414041738213, -294.0117071850597767, -195.2513479720633711 ) ) ;
#57763 = CARTESIAN_POINT ( 'NONE',  ( -112.7464469908924372, -270.5823899088603071, -270.3360381906339853 ) ) ;
#57764 = APPLICATION_CONTEXT ( 'automotive_design' ) ;
#57765 = CARTESIAN_POINT ( 'NONE',  ( 200.1126601882107252, 214.5000000000000568, -2.416251949619908856 ) ) ;
#57766 = CARTESIAN_POINT ( 'NONE',  ( -86.97243596677564881, -275.3456628214781290, -213.5890167831123279 ) ) ;
#57767 = CARTESIAN_POINT ( 'NONE',  ( 32.38209641834988162, -281.0444801106273189, -292.6889342037769097 ) ) ;
#57768 = CARTESIAN_POINT ( 'NONE',  ( -68.64163157441971919, -281.4633582630633555, -338.5176653127900863 ) ) ;
#57769 = CARTESIAN_POINT ( 'NONE',  ( -61.55040797592001667, -294.5558722014347950, -343.3420285469898090 ) ) ;
#57770 = CARTESIAN_POINT ( 'NONE',  ( -18.99911030312427940, -272.5312068727891983, -198.6035421330635415 ) ) ;
#57771 = CARTESIAN_POINT ( 'NONE',  ( -74.75780986872122469, -275.6342255996005406, -334.7144312626272153 ) ) ;
#57772 = CARTESIAN_POINT ( 'NONE',  ( -109.5332298730474179, -298.0486455991762114, -256.5235197740528861 ) ) ;
#57773 = CARTESIAN_POINT ( 'NONE',  ( 35.05965138847447804, -294.8041841703094974, -257.1222685173057698 ) ) ;
#57774 = EDGE_CURVE ( 'NONE', #15223, #77294, #89386, .T. ) ;
#57775 = CARTESIAN_POINT ( 'NONE',  ( 175.2296996224750103, 250.5000000000000568, 0.000000000000000000 ) ) ;
#57776 = CARTESIAN_POINT ( 'NONE',  ( -20.80175114107759526, -295.6373455389812079, -341.6806661967788159 ) ) ;
#57777 = CARTESIAN_POINT ( 'NONE',  ( 199.6702811234769115, 65.52214591209386185, 9.100946541886349550 ) ) ;
#57779 = CARTESIAN_POINT ( 'NONE',  ( -99.89679438943502987, -297.0710668442935685, -232.6348975792506337 ) ) ;
#57778 = CARTESIAN_POINT ( 'NONE',  ( 35.89966613158416209, -285.7994174933493241, -288.1386740624200797 ) ) ;
#57780 = CARTESIAN_POINT ( 'NONE',  ( -106.6791117930616082, -284.9817943683661383, -236.8749515313063796 ) ) ;
#57781 = CARTESIAN_POINT ( 'NONE',  ( 39.61900482242741361, -287.1979604971948561, -268.6895364089406826 ) ) ;
#57782 = CARTESIAN_POINT ( 'NONE',  ( -52.92396907888562652, -297.2306657816783968, -344.1410116829302410 ) ) ;
#57783 = CARTESIAN_POINT ( 'NONE',  ( 36.01866337056321754, -291.3618678655024041, -255.5866299321801307 ) ) ;
#57784 = CARTESIAN_POINT ( 'NONE',  ( -108.3595099276998326, -278.1229718434256029, -241.0246302697951251 ) ) ;
#57785 = DIRECTION ( 'NONE',  ( 0.000000000000000000, -1.000000000000000000, 0.000000000000000000 ) ) ;
#57786 = CARTESIAN_POINT ( 'NONE',  ( -4.402680322401938184, -285.2912578954010314, -204.7703299076844985 ) ) ;
#57788 = CARTESIAN_POINT ( 'NONE',  ( 196.9830144044668430, 72.62791770022455751, -12.32215356455109578 ) ) ;
#57787 = CARTESIAN_POINT ( 'NONE',  ( -97.92391466445977244, -288.8419787091631861, -317.3854499074386695 ) ) ;
#57789 = CARTESIAN_POINT ( 'NONE',  ( 207.4724402404595196, 29.73442829110643615, 14.90057469441958560 ) ) ;
#57790 = CARTESIAN_POINT ( 'NONE',  ( -108.9561560288349256, -298.3855953646112198, -252.4820924810838960 ) ) ;
#57791 = CARTESIAN_POINT ( 'NONE',  ( -68.44939123727516517, -281.0766820065049956, -200.5548793429686327 ) ) ;
#57793 = CARTESIAN_POINT ( 'NONE',  ( 28.99366614562987365, -280.8057480637577328, -239.7160552336791568 ) ) ;
#57792 = CARTESIAN_POINT ( 'NONE',  ( -105.0246925091827563, -295.0069644303174528, -237.2337978060400587 ) ) ;
#57794 = CARTESIAN_POINT ( 'NONE',  ( -13.78002624022826161, -294.9212698721096899, -343.6676492611216531 ) ) ;
#57795 = EDGE_CURVE ( 'NONE', #19033, #92829, #32543, .T. ) ;
#57796 = CARTESIAN_POINT ( 'NONE',  ( -110.7649813417112341, -280.7495242602191752, -255.0012891508309849 ) ) ;
#57797 = CARTESIAN_POINT ( 'NONE',  ( -108.8241415588536398, -295.4014697618312653, -286.2881081576207976 ) ) ;
#57798 = VECTOR ( 'NONE', #42349, 1000.000000000000000 ) ;
#57799 = FACE_OUTER_BOUND ( 'NONE', #26987, .T. ) ;
#57801 = CARTESIAN_POINT ( 'NONE',  ( -45.80138954890485792, -285.1396813555134031, -344.5771354168640528 ) ) ;
#57800 = AXIS2_PLACEMENT_3D ( 'NONE', #88125, #594, #36561 ) ;
#57802 = DIRECTION ( 'NONE',  ( 0.000000000000000000, 0.000000000000000000, 1.000000000000000000 ) ) ;
#57803 = CARTESIAN_POINT ( 'NONE',  ( -106.6379572354042296, -282.4809262143061233, -236.9535640164627353 ) ) ;
#57804 = CARTESIAN_POINT ( 'NONE',  ( 5.772212440723139437, -275.6810090601581464, -333.9641789397207958 ) ) ;
#57805 = CARTESIAN_POINT ( 'NONE',  ( -41.59071488508229919, -291.8306081738162447, -197.4350347343781493 ) ) ;
#57806 = CARTESIAN_POINT ( 'NONE',  ( 36.25934914640646411, -283.1204603871029235, -274.0480267787647790 ) ) ;
#57807 = CARTESIAN_POINT ( 'NONE',  ( -1.350090298528437760, -276.1380331527329872, -205.9180500180696356 ) ) ;
#57808 = CARTESIAN_POINT ( 'NONE',  ( -13.65111067311097592, -284.3497717476746516, -342.7848460376803814 ) ) ;
#57809 = CARTESIAN_POINT ( 'NONE',  ( 33.12006312800805574, -280.0767053996023037, -249.8118984309327004 ) ) ;
#57810 = CARTESIAN_POINT ( 'NONE',  ( -109.7445322865349482, -280.3007506770264854, -289.9271739634959317 ) ) ;
#57811 = CARTESIAN_POINT ( 'NONE',  ( -114.3417001280813849, -272.7188053819918423, -270.3632355433240946 ) ) ;
#57812 = CARTESIAN_POINT ( 'NONE',  ( 31.25125891221065899, -274.9348930203797181, -235.3753212275701401 ) ) ;
#57813 = CARTESIAN_POINT ( 'NONE',  ( 24.13579854213000075, -296.0460874053790121, -312.4254733604076932 ) ) ;
#57814 = CARTESIAN_POINT ( 'NONE',  ( 200.7065524281981936, 64.16053070458296759, -8.800381594948186503 ) ) ;
#57815 = DIRECTION ( 'NONE',  ( -1.000000000000000000, -0.000000000000000000, -0.000000000000000000 ) ) ;
#57816 = CARTESIAN_POINT ( 'NONE',  ( 1.121622863161765293, -292.6839494628433158, -335.6365211972881752 ) ) ;
#57817 = CARTESIAN_POINT ( 'NONE',  ( -64.58591646424200405, -273.1942962258875696, -202.5557316824814507 ) ) ;
#57818 = CARTESIAN_POINT ( 'NONE',  ( -44.84828177921385617, -293.4790213086195649, -194.3721261434434666 ) ) ;
#57820 = CARTESIAN_POINT ( 'NONE',  ( -25.10009313219005733, -293.4100133111776358, -194.7426561111478520 ) ) ;
#57819 = CARTESIAN_POINT ( 'NONE',  ( -110.4683760289727132, -281.2662352645559167, -253.7030783399848985 ) ) ;
#57821 = CARTESIAN_POINT ( 'NONE',  ( -15.28763104685571150, -290.7662682559471250, -341.9250413499781871 ) ) ;
#57822 = CARTESIAN_POINT ( 'NONE',  ( -111.0972525387210084, -276.3881652039447090, -283.0919244991044934 ) ) ;
#57823 = CARTESIAN_POINT ( 'NONE',  ( -71.08409885277004037, -279.4212488446241309, -336.7144504479687726 ) ) ;
#57824 = CARTESIAN_POINT ( 'NONE',  ( 35.36140050471799157, -291.4244242868235233, -254.3154287362765444 ) ) ;
#57825 = CARTESIAN_POINT ( 'NONE',  ( 35.78647983263250154, -283.1598202765108567, -250.4984772312153325 ) ) ;
#57826 = CARTESIAN_POINT ( 'NONE',  ( -94.53477287839518794, -282.8269493298037105, -316.2415165367745544 ) ) ;
#57827 = ORIENTED_EDGE ( 'NONE', *, *, #4015, .T. ) ;
#57828 = CARTESIAN_POINT ( 'NONE',  ( -34.85006969594519433, -282.6867461291899986, -343.3521801830165145 ) ) ;
#57829 = CARTESIAN_POINT ( 'NONE',  ( 18.92399340976638200, -281.9190673254566946, -218.2490825153763296 ) ) ;
#57830 = CARTESIAN_POINT ( 'NONE',  ( -105.4382413256048636, -282.8912557907726750, -305.5606529913536633 ) ) ;
#57831 = CARTESIAN_POINT ( 'NONE',  ( -79.79068279718737244, -280.4349750822498777, -206.3371713435682295 ) ) ;
#57832 = CARTESIAN_POINT ( 'NONE',  ( 37.50610666046531350, -277.2596719233403064, -285.2108174230646682 ) ) ;
#57833 = CARTESIAN_POINT ( 'NONE',  ( -102.0455923789670294, -275.6237833571633473, -301.4846348637937581 ) ) ;
#57834 = ORIENTED_EDGE ( 'NONE', *, *, #51060, .T. ) ;
#57835 = ORIENTED_EDGE ( 'NONE', *, *, #41133, .T. ) ;
#57836 = CARTESIAN_POINT ( 'NONE',  ( -112.0201622706384086, -274.6238543458640606, -264.8020081627651621 ) ) ;
#57837 = CARTESIAN_POINT ( 'NONE',  ( -72.44959466576179352, -275.5392528130773258, -336.2487682997601723 ) ) ;
#57838 = CARTESIAN_POINT ( 'NONE',  ( -106.3496901585683929, -292.7260543352621767, -238.4257486068886749 ) ) ;
#57839 = CARTESIAN_POINT ( 'NONE',  ( -4.297994806941224155, -293.9532431717657914, -335.5825442155469887 ) ) ;
#57840 = CARTESIAN_POINT ( 'NONE',  ( -113.6042835426848256, -290.1920487732495531, -259.7955929139251339 ) ) ;
#57841 = LINE ( 'NONE', #59234, #56742 ) ;
#57843 = CARTESIAN_POINT ( 'NONE',  ( -93.85471623216888304, -283.6187702111141675, -222.8982964493575594 ) ) ;
#57842 = CARTESIAN_POINT ( 'NONE',  ( 38.91277767054699410, -292.1981209500998489, -276.0137753120155821 ) ) ;
#57844 = CARTESIAN_POINT ( 'NONE',  ( -64.54595376625732683, -293.5536543824113664, -201.2764188900407873 ) ) ;
#57845 = CARTESIAN_POINT ( 'NONE',  ( 0.5415417606193264621, -285.0464291341202738, -207.0911145497513814 ) ) ;
#57846 = CARTESIAN_POINT ( 'NONE',  ( 16.19652850644765607, -283.5879298208346881, -320.7823645135568427 ) ) ;
#57847 = CARTESIAN_POINT ( 'NONE',  ( -113.8768577201574885, -291.4108045686492119, -276.9453784949673150 ) ) ;
#57848 = CARTESIAN_POINT ( 'NONE',  ( -32.96558757828728403, -280.6011196102725762, -197.4307533824961070 ) ) ;
#57849 = CARTESIAN_POINT ( 'NONE',  ( -4.685806924308310251, -293.4264445389100615, -339.6690997346877907 ) ) ;
#57850 = CARTESIAN_POINT ( 'NONE',  ( 24.01944054576840060, -288.9721099633155177, -316.6101097146308803 ) ) ;
#57851 = CARTESIAN_POINT ( 'NONE',  ( 10.19485166872850002, -288.9090950637611286, -330.9252065908653435 ) ) ;
#57852 = CARTESIAN_POINT ( 'NONE',  ( -27.83865374061423381, -286.3428745546037248, -197.9823081425884936 ) ) ;
#57853 = VERTEX_POINT ( 'NONE', #68990 ) ;
#57854 = DIRECTION ( 'NONE',  ( 0.000000000000000000, 1.000000000000000000, 0.000000000000000000 ) ) ;
#57855 = CARTESIAN_POINT ( 'NONE',  ( -0.04654210041249363938, -296.4218478209982095, -336.3258605110382291 ) ) ;
#57856 = CARTESIAN_POINT ( 'NONE',  ( -111.4948433797446654, -294.9992302148526164, -289.2451344136368334 ) ) ;
#57857 = CARTESIAN_POINT ( 'NONE',  ( -92.37736379734205627, -278.2985208206132484, -222.0255447989806328 ) ) ;
#57858 = CARTESIAN_POINT ( 'NONE',  ( -49.70316693167568900, -273.4063302281891765, -194.3684263932130420 ) ) ;
#57859 = CARTESIAN_POINT ( 'NONE',  ( -28.83498333370479116, -293.4223662025949579, -343.6133221923825545 ) ) ;
#57860 = CARTESIAN_POINT ( 'NONE',  ( 22.28441923346398923, -276.7063135000776128, -226.5125158938447498 ) ) ;
#57861 = CARTESIAN_POINT ( 'NONE',  ( -74.87783365778203404, -271.6866688751387073, -206.2554713857131787 ) ) ;
#57862 = CARTESIAN_POINT ( 'NONE',  ( 33.00526069309908195, -294.4795374805362940, -249.2472545493952225 ) ) ;
#57863 = CARTESIAN_POINT ( 'NONE',  ( -7.851396289375895066, -295.7360905516576395, -337.4906842188781297 ) ) ;
#57864 = CARTESIAN_POINT ( 'NONE',  ( -43.41372958812449667, -261.6932476095567495, -437.8285871551558444 ) ) ;
#57865 = VECTOR ( 'NONE', #42987, 1000.000000000000000 ) ;
#57866 = CARTESIAN_POINT ( 'NONE',  ( -110.5268021382999279, -294.3316239338815308, -287.5624013188418644 ) ) ;
#57867 = CARTESIAN_POINT ( 'NONE',  ( 76.19145359092561876, -300.0900639254019779, -193.4507982650258384 ) ) ;
#57868 = CARTESIAN_POINT ( 'NONE',  ( -102.4667466277641665, -275.0496087501944658, -233.0581151396938822 ) ) ;
#57869 = CARTESIAN_POINT ( 'NONE',  ( -109.4083297353386968, -291.3220579673526913, -283.3922094802898641 ) ) ;
#57871 = CARTESIAN_POINT ( 'NONE',  ( 1.584694542675792572, -294.8497020746069666, -332.2014491539438268 ) ) ;
#57870 = AXIS2_PLACEMENT_3D ( 'NONE', #21911, #71646, #79212 ) ;
#57872 = AXIS2_PLACEMENT_3D ( 'NONE', #35379, #44317, #73229 ) ;
#57873 = CARTESIAN_POINT ( 'NONE',  ( -103.3648796476223879, -281.0127494249105666, -234.0383074317571186 ) ) ;
#57874 = CARTESIAN_POINT ( 'NONE',  ( -101.4686624080805046, -277.7896127248654921, -228.5396223160616671 ) ) ;
#57875 = CARTESIAN_POINT ( 'NONE',  ( -4.215270454074896200, -281.9754406002269320, -339.7726506801226378 ) ) ;
#57876 = CARTESIAN_POINT ( 'NONE',  ( 37.84747674733428369, -274.6980745747902688, -254.1774086232588843 ) ) ;
#57877 = CARTESIAN_POINT ( 'NONE',  ( -36.73820986990828175, -278.4594963937113903, -194.1505946666885336 ) ) ;
#57878 = CARTESIAN_POINT ( 'NONE',  ( -9.515542739389985627, -278.4147702630452272, -200.5346660301104009 ) ) ;
#57879 = EDGE_CURVE ( 'NONE', #85558, #52800, #38686, .T. ) ;
#57880 = CARTESIAN_POINT ( 'NONE',  ( -44.60124279313166795, -296.6433344707083393, -197.1766654755183765 ) ) ;
#57881 = CARTESIAN_POINT ( 'NONE',  ( -3.143706023520141279, -278.6006310360558018, -337.1247252722678240 ) ) ;
#57882 = CARTESIAN_POINT ( 'NONE',  ( -74.94434090351494149, -282.8906705383787994, 30.50000000000000000 ) ) ;
#57883 = CARTESIAN_POINT ( 'NONE',  ( -80.54061425516390216, -289.6198778182628644, -334.1660497808048262 ) ) ;
#57884 = CARTESIAN_POINT ( 'NONE',  ( 1.449535284803833424, -276.5694342071365099, -205.9773585294363443 ) ) ;
#57885 = CARTESIAN_POINT ( 'NONE',  ( -68.79545319683467142, -295.6375985316801689, -202.4450512996676821 ) ) ;
#57886 = CARTESIAN_POINT ( 'NONE',  ( -114.1647661948828443, -283.7900534034688462, -267.1110178693853072 ) ) ;
#57887 = CYLINDRICAL_SURFACE ( 'NONE', #41050, 7.999911143031724237 ) ;
#57888 = CARTESIAN_POINT ( 'NONE',  ( -107.4669790830532179, -282.2047231629902626, -297.1033203871699584 ) ) ;
#57889 = VECTOR ( 'NONE', #6794, 1000.000000000000000 ) ;
#57890 = CARTESIAN_POINT ( 'NONE',  ( 9.111952221624832760, -291.5010449112647279, -213.4692338362773967 ) ) ;
#57891 = CARTESIAN_POINT ( 'NONE',  ( -92.42205425272727837, -283.3933965791152900, -220.5159444926252661 ) ) ;
#57892 = CARTESIAN_POINT ( 'NONE',  ( 195.0943219309016001, 27.07095573865049332, 15.17888833493343270 ) ) ;
#57893 = CARTESIAN_POINT ( 'NONE',  ( 73.43068321062709458, -134.2641364535880939, 4.999999999999990230 ) ) ;
#57894 = CARTESIAN_POINT ( 'NONE',  ( -1.460802696476545481, -290.5276815216863611, -204.4863626861958323 ) ) ;
#57895 = CARTESIAN_POINT ( 'NONE',  ( -70.18936673350430056, -281.9569427535006412, -339.2502542054396031 ) ) ;
#57896 = CARTESIAN_POINT ( 'NONE',  ( -37.79443643331234171, -278.6580090122620277, -344.1723217956323992 ) ) ;
#57897 = CARTESIAN_POINT ( 'NONE',  ( -109.8438923513058683, -285.4440442925561001, -295.0884478222125722 ) ) ;
#57898 = CARTESIAN_POINT ( 'NONE',  ( 20.34065409041034656, -286.9219765256700043, -225.6202416856829984 ) ) ;
#57899 = CARTESIAN_POINT ( 'NONE',  ( -67.02381664825605867, -278.8743147684258474, -337.6986771700387067 ) ) ;
#57900 = CARTESIAN_POINT ( 'NONE',  ( -99.30642705152872907, -278.8178961819338042, -309.3526999864703271 ) ) ;
#57901 = EDGE_CURVE ( 'NONE', #47569, #10831, #46710, .T. ) ;
#57902 = EDGE_CURVE ( 'NONE', #65856, #75719, #60695, .T. ) ;
#57903 = CARTESIAN_POINT ( 'NONE',  ( -112.1588004300198094, -286.6284405435655458, -264.4323774020255655 ) ) ;
#57904 = ORIENTED_EDGE ( 'NONE', *, *, #92091, .T. ) ;
#57905 = CARTESIAN_POINT ( 'NONE',  ( -109.8501484178673024, -296.7125833971868474, -244.4473198992276366 ) ) ;
#57906 = CARTESIAN_POINT ( 'NONE',  ( -42.75866125769783821, -291.1005951400370577, -344.8608526396287743 ) ) ;
#57907 = CARTESIAN_POINT ( 'NONE',  ( 222.8344101925596306, 0.000000000000000000, 7.000000000000000000 ) ) ;
#57908 = CARTESIAN_POINT ( 'NONE',  ( -19.05039376806008633, -279.3376638359844719, -350.3538533559490702 ) ) ;
#57909 = ORIENTED_EDGE ( 'NONE', *, *, #70691, .F. ) ;
#57910 = CARTESIAN_POINT ( 'NONE',  ( 38.80667523918234707, -291.9874672286117629, -273.1656397652747614 ) ) ;
#57911 = CARTESIAN_POINT ( 'NONE',  ( 9.456007311339179822, -288.2294416836294886, -213.4341267663791371 ) ) ;
#57912 = CARTESIAN_POINT ( 'NONE',  ( 15.97399349310584959, -282.5804604705991778, -218.9516753940150693 ) ) ;
#57913 = CARTESIAN_POINT ( 'NONE',  ( 22.51886840566906400, -288.3367686659740343, -222.8500748988525118 ) ) ;
#57914 = CARTESIAN_POINT ( 'NONE',  ( 20.21304111122029923, -289.5538065796483806, -320.7867128219516530 ) ) ;
#57915 = CARTESIAN_POINT ( 'NONE',  ( -108.0510130008192817, -286.2266261893999513, -295.5194913067584253 ) ) ;
#57916 = CARTESIAN_POINT ( 'NONE',  ( -112.1746771988216977, -278.4912865205049570, -288.5553989295952420 ) ) ;
#57917 = ORIENTED_EDGE ( 'NONE', *, *, #67180, .F. ) ;
#57918 = CARTESIAN_POINT ( 'NONE',  ( -66.39380901124575018, -293.5094113721327744, -340.1266812087301332 ) ) ;
#57919 = CARTESIAN_POINT ( 'NONE',  ( 39.61973873679414027, -281.4159453059051543, -272.7977000832070189 ) ) ;
#57921 = CARTESIAN_POINT ( 'NONE',  ( -111.1158943255973952, -274.5197282854189780, -262.1007457237456038 ) ) ;
#57920 = VECTOR ( 'NONE', #72887, 1000.000000000000000 ) ;
#57922 = CARTESIAN_POINT ( 'NONE',  ( 196.8102870837257967, 295.2234712781319104, -7.903912273553234336 ) ) ;
#57923 = CARTESIAN_POINT ( 'NONE',  ( -20.19161114001083490, -285.3376638359844719, -345.3538533559490702 ) ) ;
#57924 = CARTESIAN_POINT ( 'NONE',  ( -68.40898256894826091, -271.8894786957691849, -201.0014173510717796 ) ) ;
#57926 = AXIS2_PLACEMENT_3D ( 'NONE', #70235, #27599, #34236 ) ;
#57925 = DIRECTION ( 'NONE',  ( 0.000000000000000000, 1.000000000000000000, 0.000000000000000000 ) ) ;
#57927 = CARTESIAN_POINT ( 'NONE',  ( -98.04124089976497203, -278.6252053204775052, -229.6073770932732998 ) ) ;
#57928 = AXIS2_PLACEMENT_3D ( 'NONE', #34209, #18586, #48387 ) ;
#57929 = CARTESIAN_POINT ( 'NONE',  ( 36.11707773595592386, -277.0316649527828190, -292.1287710924053727 ) ) ;
#57930 = CARTESIAN_POINT ( 'NONE',  ( -110.6821377199610623, -273.9389781816997242, -264.8933313537352774 ) ) ;
#57931 = CARTESIAN_POINT ( 'NONE',  ( -66.49801737263513246, -282.4835095047158688, -341.3874393040812265 ) ) ;
#57932 = CARTESIAN_POINT ( 'NONE',  ( -110.1721191573525260, -292.1408148815614254, -283.5408023120857592 ) ) ;
#57933 = CARTESIAN_POINT ( 'NONE',  ( -77.85093423925658840, -299.0385433309144787, -205.6949776643984364 ) ) ;
#57934 = VECTOR ( 'NONE', #54027, 1000.000000000000000 ) ;
#57935 = CARTESIAN_POINT ( 'NONE',  ( -31.95972564808470651, -299.3231944964703075, -193.7571136113821808 ) ) ;
#57936 = CARTESIAN_POINT ( 'NONE',  ( -2.262357959318330725, -296.5868824734182567, -336.4630709188574542 ) ) ;
#57937 = CARTESIAN_POINT ( 'NONE',  ( -111.3144852122869821, -282.4020810451276020, -282.0104606228945840 ) ) ;
#57938 = VECTOR ( 'NONE', #62211, 1000.000000000000000 ) ;
#57939 = CARTESIAN_POINT ( 'NONE',  ( -114.3475782948352872, -290.2440174991040749, -268.3510277801652251 ) ) ;
#57940 = CARTESIAN_POINT ( 'NONE',  ( -2.115670954142796489, -272.5410678256044434, -204.5509844656145333 ) ) ;
#57941 = CARTESIAN_POINT ( 'NONE',  ( -60.28862596415066122, -287.3597616271641755, -197.6433379493414861 ) ) ;
#57942 = CARTESIAN_POINT ( 'NONE',  ( -57.72776959917503348, -290.7030995603292922, -199.8904496458704614 ) ) ;
#57943 = CARTESIAN_POINT ( 'NONE',  ( 86.00283748409529494, 82.43107403786450504, -302.1230288021248498 ) ) ;
#57944 = ORIENTED_EDGE ( 'NONE', *, *, #26330, .F. ) ;
#57945 = CARTESIAN_POINT ( 'NONE',  ( -112.2936024482960562, -288.9387711388957882, -285.2874840546044766 ) ) ;
#57946 = CARTESIAN_POINT ( 'NONE',  ( 23.52477684991707108, -287.7787543665789940, -310.7244985655486289 ) ) ;
#57947 = ORIENTED_EDGE ( 'NONE', *, *, #36806, .T. ) ;
#57948 = CARTESIAN_POINT ( 'NONE',  ( -63.11056363648066991, -286.8039004798685596, -198.1291431867735753 ) ) ;
#57949 = AXIS2_PLACEMENT_3D ( 'NONE', #82282, #81803, #82738 ) ;
#57950 = CARTESIAN_POINT ( 'NONE',  ( -24.32166502937336006, -277.2147515623557297, -342.2635838837631468 ) ) ;
#57951 = CARTESIAN_POINT ( 'NONE',  ( 34.15832040752763987, -292.8252844319943051, -298.0962864966012944 ) ) ;
#57952 = CARTESIAN_POINT ( 'NONE',  ( -34.47445531282367170, -283.6684072047224277, -347.2057124185507746 ) ) ;
#57953 = CARTESIAN_POINT ( 'NONE',  ( -67.58856242056587860, -284.9619679137530284, -340.4170604531349227 ) ) ;
#57954 = CARTESIAN_POINT ( 'NONE',  ( -83.86704695503310347, -284.0044684746486610, -331.7561795584875313 ) ) ;
#57955 = CARTESIAN_POINT ( 'NONE',  ( 25.15218519376723449, -281.3645076886259631, -232.4927573085191455 ) ) ;
#57956 = CARTESIAN_POINT ( 'NONE',  ( -104.2036854529545877, -256.2936084490758049, -326.7685368105336465 ) ) ;
#57957 = CARTESIAN_POINT ( 'NONE',  ( 152.5227351927868824, 207.2448686218533851, -216.6814332530730667 ) ) ;
#57958 = CARTESIAN_POINT ( 'NONE',  ( -99.20933047681515404, -245.9584877323212879, -331.5210257661068454 ) ) ;
#57959 = AXIS2_PLACEMENT_3D ( 'NONE', #61941, #69979, #62417 ) ;
#57960 = CARTESIAN_POINT ( 'NONE',  ( -21.88997815373728884, -273.4524329690652849, -198.8499579133226973 ) ) ;
#57961 = CARTESIAN_POINT ( 'NONE',  ( -103.0662753845434594, -295.5371147025082905, -310.3587067909311372 ) ) ;
#57962 = CARTESIAN_POINT ( 'NONE',  ( 65.87130157267131381, 45.95421370783718373, -315.7040055182292804 ) ) ;
#57963 = CARTESIAN_POINT ( 'NONE',  ( -83.27058146805659078, -272.1228470166442435, -209.1079281782014050 ) ) ;
#57964 = CARTESIAN_POINT ( 'NONE',  ( -105.9120666866129881, -298.7876250773315405, -241.9187146393726664 ) ) ;
#57965 = CARTESIAN_POINT ( 'NONE',  ( 35.61577882131522443, -288.9833888269830595, -279.2183039413944243 ) ) ;
#57966 = EDGE_LOOP ( 'NONE', ( #17964, #91296, #39618, #24873 ) ) ;
#57967 = CARTESIAN_POINT ( 'NONE',  ( -58.77409896342661000, -296.2638914781307449, -344.1286095331149113 ) ) ;
#57968 = CARTESIAN_POINT ( 'NONE',  ( -85.77162586964622903, -285.8526865714146652, -215.5894649151744318 ) ) ;
#57969 = CARTESIAN_POINT ( 'NONE',  ( -31.27076875955219037, -273.0474397133080515, -193.8976688145276057 ) ) ;
#57970 = AXIS2_PLACEMENT_3D ( 'NONE', #45892, #51594, #22719 ) ;
#57971 = CARTESIAN_POINT ( 'NONE',  ( 11.10444422333766212, -295.2040053080797293, -330.0713715905176286 ) ) ;
#57972 = CARTESIAN_POINT ( 'NONE',  ( 15.44102743755717455, -294.8219663328866318, -326.3388865504052205 ) ) ;
#57973 = CARTESIAN_POINT ( 'NONE',  ( -109.7892537389686822, -290.6005840244441742, -279.3250445941597491 ) ) ;
#57974 = ORIENTED_EDGE ( 'NONE', *, *, #59748, .F. ) ;
#57975 = CARTESIAN_POINT ( 'NONE',  ( -36.97180572203875926, -275.9769297164795034, -194.7892118385888409 ) ) ;
#57976 = CARTESIAN_POINT ( 'NONE',  ( 25.82587467193739172, -273.7719727846267119, -227.0035082255900818 ) ) ;
#57977 = EDGE_CURVE ( 'NONE', #8225, #45777, #83634, .T. ) ;
#57978 = ORIENTED_EDGE ( 'NONE', *, *, #3303, .T. ) ;
#57979 = CARTESIAN_POINT ( 'NONE',  ( -112.7345878779304655, -277.8669404598197161, -285.7702861374085046 ) ) ;
#57980 = UNCERTAINTY_MEASURE_WITH_UNIT (LENGTH_MEASURE( 1.000000000000000082E-05 ), #65421, 'distance_accuracy_value', 'NONE');
#57981 = CARTESIAN_POINT ( 'NONE',  ( -1.314477122054709790, -272.9382931443856819, -205.9379537215812945 ) ) ;
#57982 = CARTESIAN_POINT ( 'NONE',  ( -90.42990050973847360, -274.3579567062921001, -219.7871448756984023 ) ) ;
#57983 = CARTESIAN_POINT ( 'NONE',  ( 33.81800032064830219, -276.7217166434894011, -287.7259852466841039 ) ) ;
#57984 = CARTESIAN_POINT ( 'NONE',  ( -36.21977334332840570, -299.6660977551940164, -194.1608129806244563 ) ) ;
#57985 = CARTESIAN_POINT ( 'NONE',  ( 35.98536907922287753, -273.7948330341387191, -287.7817467990586238 ) ) ;
#57986 = CARTESIAN_POINT ( 'NONE',  ( -108.9829614058983935, -297.0112024697855873, -284.9637921210493232 ) ) ;
#57987 = CARTESIAN_POINT ( 'NONE',  ( 35.29848094363444488, -291.9716832778467506, -258.5017518920986390 ) ) ;
#57988 = DIRECTION ( 'NONE',  ( -1.000000000000000000, 0.000000000000000000, -0.000000000000000000 ) ) ;
#57989 = CARTESIAN_POINT ( 'NONE',  ( -97.87660440787995242, -278.4091601258947435, -317.8485085972333195 ) ) ;
#57990 = CARTESIAN_POINT ( 'NONE',  ( 35.37801293613929943, -275.6272503179661726, -263.4186342899220676 ) ) ;
#57991 = CARTESIAN_POINT ( 'NONE',  ( -85.19136032609551989, -284.0917305533400850, -210.6643149663782140 ) ) ;
#57992 = CARTESIAN_POINT ( 'NONE',  ( -111.7895985030628623, -298.6863644335945196, -259.8976917860873641 ) ) ;
#57993 = CARTESIAN_POINT ( 'NONE',  ( 209.3673903755802428, 36.49853773373599353, 14.70256938371377586 ) ) ;
#57994 = CIRCLE ( 'NONE', #32279, 0.5000000000000004441 ) ;
#57995 = CARTESIAN_POINT ( 'NONE',  ( 4.826764251499326974, -285.8349637300727863, -210.5126447686693041 ) ) ;
#57996 = CARTESIAN_POINT ( 'NONE',  ( -97.72523120260932217, -276.2023397483587814, -313.1827078333365648 ) ) ;
#57997 = CARTESIAN_POINT ( 'NONE',  ( -109.0646139898000655, -276.9106445390127647, -286.8851283024349073 ) ) ;
#57998 = CARTESIAN_POINT ( 'NONE',  ( -52.99558996750827333, -285.2528415699865718, -343.7617614044169727 ) ) ;
#57999 = CARTESIAN_POINT ( 'NONE',  ( -78.84395163397067563, -278.8300969374211604, -330.9597099508901010 ) ) ;
#58000 = CARTESIAN_POINT ( 'NONE',  ( 155.3770881450913066, 21.00000000067704065, 15.20409621215158147 ) ) ;
#58001 = CIRCLE ( 'NONE', #64029, 1.000000000000000888 ) ;
#58002 = CARTESIAN_POINT ( 'NONE',  ( 31.83544251731552066, -273.5375228602582638, -238.2828760193348785 ) ) ;
#58003 = VECTOR ( 'NONE', #69142, 1000.000000000000000 ) ;
#58004 = CARTESIAN_POINT ( 'NONE',  ( -11.46188540723281157, -275.0496619549842308, -201.9394054434694397 ) ) ;
#58005 = CARTESIAN_POINT ( 'NONE',  ( -4.482612943415483109, -282.4842437346626980, -202.7428891052908568 ) ) ;
#58006 = LINE ( 'NONE', #43317, #66517 ) ;
#58007 = CARTESIAN_POINT ( 'NONE',  ( -8.754838620703363716, -290.6012186759199949, -340.3187079258790959 ) ) ;
#58008 = CARTESIAN_POINT ( 'NONE',  ( -5.114983384847434422, -290.4761587534719638, -202.6239211019535276 ) ) ;
#58009 = DIRECTION ( 'NONE',  ( 1.000000000000000000, 0.000000000000000000, 0.000000000000000000 ) ) ;
#58010 = CARTESIAN_POINT ( 'NONE',  ( -47.31157739077964663, -296.7177062594981294, -197.5928365763701891 ) ) ;
#58011 = CARTESIAN_POINT ( 'NONE',  ( -108.9369993599405575, -288.9466569878051132, -250.7402461863096903 ) ) ;
#58012 = CARTESIAN_POINT ( 'NONE',  ( 206.7397234113112461, 289.2571863808457238, -82.84736978277094011 ) ) ;
#58013 = DIRECTION ( 'NONE',  ( 0.000000000000000000, 0.000000000000000000, 1.000000000000000000 ) ) ;
#58014 = CARTESIAN_POINT ( 'NONE',  ( -97.62389091526596019, -288.4015994249926962, -317.1453592308348561 ) ) ;
#58015 = CARTESIAN_POINT ( 'NONE',  ( 3.853494484154238897, -284.0878342660837461, -331.6552591172966800 ) ) ;
#58016 = CARTESIAN_POINT ( 'NONE',  ( -69.34535327703582652, -283.8767370577998008, -201.4285841878118504 ) ) ;
#58017 = AXIS2_PLACEMENT_3D ( 'NONE', #4758, #33638, #62548 ) ;
#58018 = CARTESIAN_POINT ( 'NONE',  ( -38.87933752907440521, -284.4970543968106540, -343.9468747881980448 ) ) ;
#58019 = CARTESIAN_POINT ( 'NONE',  ( -92.67456725497034142, -284.6743141904848926, -318.2432709669318456 ) ) ;
#58020 = CARTESIAN_POINT ( 'NONE',  ( -95.32966075447173182, -293.1933996588815035, -222.2183753510427664 ) ) ;
#58021 = CARTESIAN_POINT ( 'NONE',  ( -21.36332248027393277, -274.5849746800601565, -195.0588222726696017 ) ) ;
#58022 = AXIS2_PLACEMENT_3D ( 'NONE', #66171, #22587, #50074 ) ;
#58023 = CARTESIAN_POINT ( 'NONE',  ( -110.8672560792099517, -288.4093398246986339, -287.8322593850211888 ) ) ;
#58024 = CARTESIAN_POINT ( 'NONE',  ( -89.21211456894610592, -277.7584503748461771, -327.2685876656598793 ) ) ;
#58025 = CARTESIAN_POINT ( 'NONE',  ( -15.07875183164729904, -296.7424399670423441, -341.6630050940867704 ) ) ;
#58026 = CARTESIAN_POINT ( 'NONE',  ( 170.0287519320418426, 214.7033776542919270, -24.48382199637804391 ) ) ;
#58027 = CARTESIAN_POINT ( 'NONE',  ( -95.99890600148557951, -293.6948066931273615, -223.6242672951989618 ) ) ;
#58028 = CARTESIAN_POINT ( 'NONE',  ( -7.065519761082431849, -281.3312207024949885, -337.3420515909402297 ) ) ;
#58029 = CARTESIAN_POINT ( 'NONE',  ( -112.2543317963196756, -276.4651448884366118, -277.1397823103512792 ) ) ;
#58030 = CARTESIAN_POINT ( 'NONE',  ( -87.56534430447884176, -271.8462119899706977, -212.8427033253181833 ) ) ;
#58031 = CARTESIAN_POINT ( 'NONE',  ( 32.19258364702903208, -275.1996099819655228, -292.9193991244355857 ) ) ;
#58032 = CARTESIAN_POINT ( 'NONE',  ( -30.76418577546842670, -293.6569318120509138, -196.9619077869228931 ) ) ;
#58033 = AXIS2_PLACEMENT_3D ( 'NONE', #3639, #18784, #17392 ) ;
#58034 = CARTESIAN_POINT ( 'NONE',  ( 6.808581593899909024, -293.6111131926185749, -211.9302950269529902 ) ) ;
#58035 = ADVANCED_FACE ( 'NONE', ( #17859 ), #40983, .T. ) ;
#58036 = CARTESIAN_POINT ( 'NONE',  ( -27.93973295721343675, -293.5944217172304889, -194.4777209330175651 ) ) ;
#58037 = CARTESIAN_POINT ( 'NONE',  ( 38.74846915369588629, -294.9738405522844573, -278.8235739748855622 ) ) ;
#58038 = CARTESIAN_POINT ( 'NONE',  ( -109.8047542567639567, -296.2635457049055390, -279.6037386176658970 ) ) ;
#58039 = CARTESIAN_POINT ( 'NONE',  ( -75.71797130309303725, -291.5644342604998656, -334.8142557203633487 ) ) ;
#58040 = CARTESIAN_POINT ( 'NONE',  ( -69.18451763150262934, -283.6262268035989678, -340.4828423024381436 ) ) ;
#58041 = CARTESIAN_POINT ( 'NONE',  ( 19.13128258684973559, -272.9949076995151245, -219.7754980095072312 ) ) ;
#58042 = CARTESIAN_POINT ( 'NONE',  ( 1.523511929468046810, -286.3899094786020783, -203.8740162535708578 ) ) ;
#58043 = CARTESIAN_POINT ( 'NONE',  ( -71.17631175773820473, -279.4809773108131026, -336.8973176179463280 ) ) ;
#58044 = EDGE_CURVE ( 'NONE', #20110, #32677, #69819, .T. ) ;
#58045 = CARTESIAN_POINT ( 'NONE',  ( -37.26513326156666039, -284.8480174657229327, -196.9515777883170813 ) ) ;
#58046 = CARTESIAN_POINT ( 'NONE',  ( -20.95875266260309644, -286.8418832604791078, -343.6031557897267703 ) ) ;
#58047 = CARTESIAN_POINT ( 'NONE',  ( -64.28062463050963515, -277.8440752353067182, -199.4919593508309674 ) ) ;
#58048 = CARTESIAN_POINT ( 'NONE',  ( 201.7194887906492795, 294.2213704821156739, -83.28174295417332473 ) ) ;
#58049 = CARTESIAN_POINT ( 'NONE',  ( -100.4574440433205496, -283.5551444016153368, -307.1631737887294662 ) ) ;
#58050 = CARTESIAN_POINT ( 'NONE',  ( 36.94242822685470173, -282.5219717217978541, -251.6561187980134662 ) ) ;
#58051 = CARTESIAN_POINT ( 'NONE',  ( 5.416295624588007840, -287.5473329941611382, -334.1151297126202167 ) ) ;
#58052 = CARTESIAN_POINT ( 'NONE',  ( -50.81836651915342884, -281.4828580095158372, -195.3623188151042882 ) ) ;
#58053 = CARTESIAN_POINT ( 'NONE',  ( -71.33657836451762080, -278.8068300518057185, -338.9004973820360647 ) ) ;
#58054 = CARTESIAN_POINT ( 'NONE',  ( -64.81414821861213227, -279.5163969691662942, -202.7278081387677275 ) ) ;
#58055 = CARTESIAN_POINT ( 'NONE',  ( -93.26683097515734744, -275.2227753164444266, -220.9219984096359042 ) ) ;
#58056 = CARTESIAN_POINT ( 'NONE',  ( 36.28697950038537812, -293.2691941108852234, -247.8263107686384501 ) ) ;
#58057 = CARTESIAN_POINT ( 'NONE',  ( 27.10365975825455109, -286.0790720819892385, -308.1281155714692090 ) ) ;
#58058 = CARTESIAN_POINT ( 'NONE',  ( 1.276894379539621260, -294.1586378531939090, -204.6118266236744034 ) ) ;
#58059 = CARTESIAN_POINT ( 'NONE',  ( -110.5200336616545087, -295.5299702738424230, -265.9841813721533867 ) ) ;
#58060 = CARTESIAN_POINT ( 'NONE',  ( 35.22744216943532081, -293.3317057668817824, -278.9172289681784491 ) ) ;
#58061 = CARTESIAN_POINT ( 'NONE',  ( -104.3466099793609629, -292.1174056806706858, -233.0538189002723186 ) ) ;
#58062 = CARTESIAN_POINT ( 'NONE',  ( 28.24618613459835004, -282.6417707717410508, -302.7579329370664141 ) ) ;
#58063 = CARTESIAN_POINT ( 'NONE',  ( -73.82244513651923512, -272.6389941353839959, -202.7596332637443766 ) ) ;
#58064 = CARTESIAN_POINT ( 'NONE',  ( -46.00603543053564692, -289.8105630052190804, -346.8225642779727877 ) ) ;
#58065 = CARTESIAN_POINT ( 'NONE',  ( -68.69724718499702476, -281.5994587043184083, -339.3472914433079950 ) ) ;
#58066 = CARTESIAN_POINT ( 'NONE',  ( -112.2411303655110117, -290.6624099612610621, -288.1888209112111667 ) ) ;
#58067 = CARTESIAN_POINT ( 'NONE',  ( -41.32832582202011906, -286.3338950261834839, -197.4363790608946658 ) ) ;
#58068 = CARTESIAN_POINT ( 'NONE',  ( 208.4306832106270804, -198.2391364535880598, -7.500000000000012434 ) ) ;
#58069 = TOROIDAL_SURFACE ( 'NONE', #17228, 2.103083949679977582, 2.000000000000000000 ) ;
#58070 = CARTESIAN_POINT ( 'NONE',  ( 4.150380923130051691, -57.95720081330512130, -352.8324262869497829 ) ) ;
#58071 = CARTESIAN_POINT ( 'NONE',  ( 200.7764005794019226, 290.0384947088795116, -82.33303656482503641 ) ) ;
#58072 = CARTESIAN_POINT ( 'NONE',  ( -107.2739951928463853, -277.4631946985408035, -292.0267890297669737 ) ) ;
#58073 = CARTESIAN_POINT ( 'NONE',  ( -9.115677510991886834, -279.3504792048175887, -202.7037627185481199 ) ) ;
#58074 = CARTESIAN_POINT ( 'NONE',  ( 37.26578296297303439, -274.9815630207957042, -251.4014830062171200 ) ) ;
#58075 = CARTESIAN_POINT ( 'NONE',  ( -61.34299255263732675, -183.7475365659067279, -360.0278117845444399 ) ) ;
#58076 = CARTESIAN_POINT ( 'NONE',  ( -50.81774693757084549, -278.4579443672043908, -195.1480708842843512 ) ) ;
#58078 = CARTESIAN_POINT ( 'NONE',  ( -23.79109945897418044, -280.8982609153710541, -343.7656683956664097 ) ) ;
#58077 = AXIS2_PLACEMENT_3D ( 'NONE', #5252, #91389, #10910 ) ;
#58079 = CARTESIAN_POINT ( 'NONE',  ( -34.86492208978587115, -296.7815727770631611, -346.3074120756865000 ) ) ;
#58080 = CARTESIAN_POINT ( 'NONE',  ( -69.04997580472544882, -292.1159276326052918, -204.5250139924184509 ) ) ;
#58081 = CARTESIAN_POINT ( 'NONE',  ( -82.86476396339747907, -288.3748244922185791, -328.0576875132261421 ) ) ;
#58082 = CARTESIAN_POINT ( 'NONE',  ( 37.53375497045848164, -275.9834968945108358, -252.7830485950662762 ) ) ;
#58083 = CARTESIAN_POINT ( 'NONE',  ( -103.9357459632928169, -296.3145401263366807, -300.3884054730339699 ) ) ;
#58084 = EDGE_LOOP ( 'NONE', ( #10048, #34761, #80647, #38102, #66781, #81203 ) ) ;
#58085 = CARTESIAN_POINT ( 'NONE',  ( 125.9462722777150958, 8.500086813760361792, -21.49999999999998579 ) ) ;
#58086 = FACE_OUTER_BOUND ( 'NONE', #19281, .T. ) ;
#58087 = AXIS2_PLACEMENT_3D ( 'NONE', #88494, #8945, #45384 ) ;
#58088 = AXIS2_PLACEMENT_3D ( 'NONE', #27788, #64726, #14043 ) ;
#58089 = CARTESIAN_POINT ( 'NONE',  ( -104.8992630881107289, -280.9172392771650948, -236.4023818595052830 ) ) ;
#58090 = CIRCLE ( 'NONE', #62623, 1.000000000000000888 ) ;
#58091 = CARTESIAN_POINT ( 'NONE',  ( -7.887817190267499612, -281.5270496202666095, -203.2154677488197194 ) ) ;
#58092 = CARTESIAN_POINT ( 'NONE',  ( -81.66617511274853314, -281.2179399937946300, -208.6414701474983815 ) ) ;
#58093 = CARTESIAN_POINT ( 'NONE',  ( 34.93384275606230460, -280.7662886490513756, -282.1786621100433763 ) ) ;
#58094 = CARTESIAN_POINT ( 'NONE',  ( -0.1800722102555995519, -273.0359436540743445, -206.7089669986499985 ) ) ;
#58095 = ADVANCED_FACE ( 'NONE', ( #61883 ), #76557, .T. ) ;
#58096 = PLANE ( 'NONE',  #56388 ) ;
#58097 = ADVANCED_FACE ( 'NONE', ( #17233 ), #15365, .F. ) ;
#58098 = CARTESIAN_POINT ( 'NONE',  ( 189.9243309297870610, 276.0000000000000568, 24.72542485937349710 ) ) ;
#58100 = MANIFOLD_SOLID_BREP ( 'Boss-Extrude20', #20449 ) ;
#58099 = CARTESIAN_POINT ( 'NONE',  ( 37.43709352827445969, -276.5771073813437511, -288.0895771496482780 ) ) ;
#58101 = CIRCLE ( 'NONE', #3679, 2.000000000000000000 ) ;
#58102 = VERTEX_POINT ( 'NONE', #16758 ) ;
#58103 = CARTESIAN_POINT ( 'NONE',  ( 37.32359682799047818, -277.4546810761565894, -262.7571168176075389 ) ) ;
#58104 = CARTESIAN_POINT ( 'NONE',  ( -42.78246696935688931, -275.6942774959569533, -346.5779425637010149 ) ) ;
#58105 = ORIENTED_EDGE ( 'NONE', *, *, #12972, .F. ) ;
#58106 = DIRECTION ( 'NONE',  ( -1.000000000000000000, -0.000000000000000000, -0.000000000000000000 ) ) ;
#58107 = CARTESIAN_POINT ( 'NONE',  ( -108.6596969937836121, -286.2187358259548091, -294.6952529583228397 ) ) ;
#58108 = CARTESIAN_POINT ( 'NONE',  ( 27.63462644800139500, -292.2930568541190723, -236.7355516509282438 ) ) ;
#58109 = CARTESIAN_POINT ( 'NONE',  ( -7.375185896956212517, -285.7833848721528511, -199.4856045071344965 ) ) ;
#58110 = CARTESIAN_POINT ( 'NONE',  ( -59.26944187115613261, -281.5796180740320551, -341.1055124302971535 ) ) ;
#58112 = CARTESIAN_POINT ( 'NONE',  ( -11.49959828440748844, -284.4712449703861807, -200.5506605292513314 ) ) ;
#58111 = CARTESIAN_POINT ( 'NONE',  ( -29.39895045103452986, -281.5244370202834148, -343.5713594295870053 ) ) ;
#58113 = CARTESIAN_POINT ( 'NONE',  ( -40.23472935808855055, -284.2944036596261981, -343.7011540307281621 ) ) ;
#58114 = CARTESIAN_POINT ( 'NONE',  ( 28.21215188203397162, -273.0658602033119564, -233.8167363385458941 ) ) ;
#58115 = CARTESIAN_POINT ( 'NONE',  ( -107.1846265291710267, -283.3460619258278825, -239.7595096511194015 ) ) ;
#58116 = CARTESIAN_POINT ( 'NONE',  ( -44.57666132767873535, -297.1437322776046130, -345.0633607831865675 ) ) ;
#58117 = CARTESIAN_POINT ( 'NONE',  ( -108.8390751952717324, -279.7026395955065823, -254.4438492254772370 ) ) ;
#58118 = CARTESIAN_POINT ( 'NONE',  ( 22.69367743960799899, -290.1692442227603124, -315.5914382344669775 ) ) ;
#58119 = CARTESIAN_POINT ( 'NONE',  ( 195.4888831047267104, 26.84972106461252039, 13.90636001966099222 ) ) ;
#58120 = DIRECTION ( 'NONE',  ( -0.6056179655966479336, 0.7957555401921982963, 0.000000000000000000 ) ) ;
#58121 = CARTESIAN_POINT ( 'NONE',  ( 37.80765212740534764, -295.5787231040843039, -278.7109828355824561 ) ) ;
#58122 = CARTESIAN_POINT ( 'NONE',  ( -96.03366072200009285, -275.9099979583385789, -317.0748345797995853 ) ) ;
#58123 = CARTESIAN_POINT ( 'NONE',  ( -81.82855832738623292, -290.6601124348729854, -207.7106729114560437 ) ) ;
#58124 = CARTESIAN_POINT ( 'NONE',  ( 36.09351406484742597, -291.8499248358819500, -262.5371335739541792 ) ) ;
#58125 = CARTESIAN_POINT ( 'NONE',  ( -108.4454746125458939, -277.4813229767582357, -251.7241876869527175 ) ) ;
#58126 = CARTESIAN_POINT ( 'NONE',  ( -111.6203922558816828, -294.6774983837302671, -271.4581198762632539 ) ) ;
#58127 = CARTESIAN_POINT ( 'NONE',  ( -66.77686560023559537, -292.9733686963554078, -203.0200865626528923 ) ) ;
#58128 = CARTESIAN_POINT ( 'NONE',  ( 21.27581636871892101, -277.4090924074130839, -223.5744983911110353 ) ) ;
#58129 = CARTESIAN_POINT ( 'NONE',  ( -94.14848543269195602, -294.3343536260022120, -321.3285737856231208 ) ) ;
#58130 = CARTESIAN_POINT ( 'NONE',  ( -39.96620742770257806, -290.6856771952818690, -344.1645583920227978 ) ) ;
#58131 = CARTESIAN_POINT ( 'NONE',  ( -96.65829578305333314, -289.4366997935707104, -222.8688502139236221 ) ) ;
#58132 = CARTESIAN_POINT ( 'NONE',  ( -66.54630436392351100, -290.8674575965489453, -337.9615916549828967 ) ) ;
#58133 = DIRECTION ( 'NONE',  ( 0.000000000000000000, 1.000000000000000000, 0.000000000000000000 ) ) ;
#58134 = CARTESIAN_POINT ( 'NONE',  ( -53.43411977051503925, -290.0667442679009582, -341.7308297408944782 ) ) ;
#58135 = CARTESIAN_POINT ( 'NONE',  ( 9.339199855150265961, -282.8906705383787994, 54.50000000000000711 ) ) ;
#58136 = CARTESIAN_POINT ( 'NONE',  ( 30.02086805183671459, -289.2327344315385176, -306.9452775134249123 ) ) ;
#58137 = CARTESIAN_POINT ( 'NONE',  ( -94.63840741837749704, -277.2470690740486248, -221.3975218768623563 ) ) ;
#58138 = CARTESIAN_POINT ( 'NONE',  ( -86.79438808761707946, -279.7195724562905639, -211.2986212505088588 ) ) ;
#58139 = CARTESIAN_POINT ( 'NONE',  ( 38.40400318723140316, -281.3914658198540906, -284.1577490257680552 ) ) ;
#58140 = CARTESIAN_POINT ( 'NONE',  ( 5.898681362571513098, -284.6378285777316819, -209.0172929725891890 ) ) ;
#58141 = DIRECTION ( 'NONE',  ( 0.000000000000000000, 1.000000000000000000, 0.000000000000000000 ) ) ;
#58142 = CARTESIAN_POINT ( 'NONE',  ( 36.93846939916910088, -279.7046024831439581, -271.3535212377353787 ) ) ;
#58143 = CARTESIAN_POINT ( 'NONE',  ( -51.76309827054496537, -283.8676133526888634, -196.7077099370488042 ) ) ;
#58144 = CARTESIAN_POINT ( 'NONE',  ( 219.8344101925596021, 35.72494958537217968, 10.00000000000000000 ) ) ;
#58145 = CARTESIAN_POINT ( 'NONE',  ( -113.6914920201685675, -277.0166758763592156, -271.5778457032989763 ) ) ;
#58146 = AXIS2_PLACEMENT_3D ( 'NONE', #69519, #61956, #34012 ) ;
#58147 = CARTESIAN_POINT ( 'NONE',  ( -114.0461692048122728, -283.4415372073010531, -272.8255267826199884 ) ) ;
#58148 = CARTESIAN_POINT ( 'NONE',  ( -106.4622846741645219, -273.6731683360382021, -246.3830755511384325 ) ) ;
#58149 = CARTESIAN_POINT ( 'NONE',  ( -111.0458907210802693, -292.2130409872805217, -265.7052345044734807 ) ) ;
#58150 = CARTESIAN_POINT ( 'NONE',  ( -113.7524713807139705, -273.9771950811366992, -270.3792247829380813 ) ) ;
#58151 = CARTESIAN_POINT ( 'NONE',  ( -13.78259093020018966, -276.4046617866653150, -339.5305187275776575 ) ) ;
#58152 = CARTESIAN_POINT ( 'NONE',  ( -4.647247290047434198, -296.6216490848483431, -337.8740016912877309 ) ) ;
#58153 = CARTESIAN_POINT ( 'NONE',  ( -41.75843606997117519, -289.2729999745291138, -347.2475633928224283 ) ) ;
#58154 = CARTESIAN_POINT ( 'NONE',  ( 37.24242959245018625, -279.7872982877071308, -282.5463993290489952 ) ) ;
#58155 = VECTOR ( 'NONE', #54087, 1000.000000000000000 ) ;
#58156 = CARTESIAN_POINT ( 'NONE',  ( 21.31182469501179710, -292.7126773535778170, -220.4534602408569981 ) ) ;
#58157 = CARTESIAN_POINT ( 'NONE',  ( -75.09064724807500113, -290.5949536241686815, -207.5450421195383512 ) ) ;
#58158 = CARTESIAN_POINT ( 'NONE',  ( 23.25493510020844568, -292.1544723400600674, -314.5760494118696897 ) ) ;
#58159 = VERTEX_POINT ( 'NONE', #81609 ) ;
#58160 = LINE ( 'NONE', #87005, #86220 ) ;
#58161 = VECTOR ( 'NONE', #24793, 1000.000000000000000 ) ;
#58162 = CARTESIAN_POINT ( 'NONE',  ( -95.15924850839601845, -290.6881560999083263, -225.6943569499026694 ) ) ;
#58163 = CARTESIAN_POINT ( 'NONE',  ( 208.0840766214418522, 28.61636207333354420, 12.00000001296747598 ) ) ;
#58164 = CARTESIAN_POINT ( 'NONE',  ( -87.60495630512930632, -286.3119319893715442, -212.2698325297329518 ) ) ;
#58165 = CARTESIAN_POINT ( 'NONE',  ( -102.0455923789670294, -299.4805209788416391, -239.2376011013261916 ) ) ;
#58166 = CARTESIAN_POINT ( 'NONE',  ( 8.755272314045448923, -293.4960405479972678, -331.7442536467502805 ) ) ;
#58167 = CARTESIAN_POINT ( 'NONE',  ( -97.64531095546610118, -285.2341442602851203, -317.4437346898933470 ) ) ;
#58168 = CARTESIAN_POINT ( 'NONE',  ( -91.51979591788378343, -285.0868590290985480, -221.3610445873512163 ) ) ;
#58169 = CARTESIAN_POINT ( 'NONE',  ( 21.40120753946386856, -277.6916707330460667, -314.8580679110328333 ) ) ;
#58170 = CARTESIAN_POINT ( 'NONE',  ( 19.20224966008033007, -292.2512021112938214, -319.1107590957861930 ) ) ;
#58171 = CARTESIAN_POINT ( 'NONE',  ( -2.649204134466999871, -296.3469020013373552, -335.7400498873485049 ) ) ;
#58172 = AXIS2_PLACEMENT_3D ( 'NONE', #59687, #89920, #45904 ) ;
#58173 = EDGE_CURVE ( 'NONE', #91480, #51603, #45612, .T. ) ;
#58174 = CARTESIAN_POINT ( 'NONE',  ( 35.99787384989392081, -274.3993974097767818, -274.3494230838704766 ) ) ;
#58175 = ORIENTED_EDGE ( 'NONE', *, *, #8991, .T. ) ;
#58176 = CARTESIAN_POINT ( 'NONE',  ( 195.4218348477629092, 41.23934650999667895, 12.97788390064105712 ) ) ;
#58177 = CARTESIAN_POINT ( 'NONE',  ( -27.75467754098094630, -294.6004269303717251, -346.7939301232727871 ) ) ;
#58178 = CARTESIAN_POINT ( 'NONE',  ( 36.98896478362897255, -289.4090146425779153, -265.4681568108989609 ) ) ;
#58179 = CARTESIAN_POINT ( 'NONE',  ( 201.0756561822067283, 294.6070805894804039, -54.00000000001602984 ) ) ;
#58180 = CARTESIAN_POINT ( 'NONE',  ( -108.6064754957646414, -297.9942967510186804, -241.8841888743917252 ) ) ;
#58181 = CARTESIAN_POINT ( 'NONE',  ( -37.28911722089344494, -286.7042057330593821, -197.2467474533602001 ) ) ;
#58182 = CARTESIAN_POINT ( 'NONE',  ( -114.1496692561285897, -277.5954527040032644, -271.5926221306101525 ) ) ;
#58183 = CARTESIAN_POINT ( 'NONE',  ( -2.006923001309273147, -295.2480227849424068, -338.6602125031901664 ) ) ;
#58184 = CARTESIAN_POINT ( 'NONE',  ( 0.08811404618136316202, -286.6994295562074058, -336.2938687728841956 ) ) ;
#58185 = CARTESIAN_POINT ( 'NONE',  ( -109.4162445723863613, -296.5416390757753788, -297.5485770366490215 ) ) ;
#58186 = CARTESIAN_POINT ( 'NONE',  ( -9.723414220745366876, -292.7562889745286157, -202.7105900535066496 ) ) ;
#58187 = CARTESIAN_POINT ( 'NONE',  ( 196.8324751178603833, 70.49344883866203304, -10.86630005027734569 ) ) ;
#58188 = CARTESIAN_POINT ( 'NONE',  ( 199.3125048137908948, 285.7142621462966758, -96.33704470926366525 ) ) ;
#58189 = CARTESIAN_POINT ( 'NONE',  ( -12.94387731139556230, -287.8837015179771015, -198.0599838732290152 ) ) ;
#58190 = CARTESIAN_POINT ( 'NONE',  ( 13.79469577742117181, -291.9094976428775681, -334.5364918783848793 ) ) ;
#58191 = VERTEX_POINT ( 'NONE', #23407 ) ;
#58192 = CARTESIAN_POINT ( 'NONE',  ( -112.6160518909101143, -278.0983804025460699, -254.5787211769742271 ) ) ;
#58193 = CARTESIAN_POINT ( 'NONE',  ( -64.70254933119690577, -285.4104154456896936, -340.0131987695918383 ) ) ;
#58194 = CARTESIAN_POINT ( 'NONE',  ( -57.58224511544654689, -284.3706881286718726, -196.6249433411143741 ) ) ;
#58195 = CARTESIAN_POINT ( 'NONE',  ( -31.78785177576666499, -287.0615003758479133, -344.6452725989614692 ) ) ;
#58196 = CARTESIAN_POINT ( 'NONE',  ( 37.50363879299571579, -277.2619328982166280, -258.5098731277219599 ) ) ;
#58197 = CARTESIAN_POINT ( 'NONE',  ( -109.2015176975791348, -296.8696473118008612, -283.6271734132493521 ) ) ;
#58198 = ORIENTED_EDGE ( 'NONE', *, *, #907, .T. ) ;
#58199 = CARTESIAN_POINT ( 'NONE',  ( -6.573601784386866598, -293.3242419362358078, -337.1036651603427572 ) ) ;
#58200 = CARTESIAN_POINT ( 'NONE',  ( -90.99300181464917614, -279.9661299703982422, -215.1973980773842641 ) ) ;
#58202 = CARTESIAN_POINT ( 'NONE',  ( -106.5385291618271282, -278.2154274947003501, -246.6326131620838851 ) ) ;
#58201 = CARTESIAN_POINT ( 'NONE',  ( -71.65418411124608156, -277.5188250187982248, -334.8085431949305644 ) ) ;
#58203 = CARTESIAN_POINT ( 'NONE',  ( -29.88268093593819330, -275.2241496302303858, -194.0338257326666564 ) ) ;
#58204 = CARTESIAN_POINT ( 'NONE',  ( -31.48763716215004393, -275.9003400867459845, -346.8806632889305774 ) ) ;
#58205 = CARTESIAN_POINT ( 'NONE',  ( 43.54794645580765433, 12.48440977809399044, -329.5723226709832261 ) ) ;
#58206 = CARTESIAN_POINT ( 'NONE',  ( -113.7489416061644079, -297.9866821896073930, -269.6264473118700948 ) ) ;
#58207 = CARTESIAN_POINT ( 'NONE',  ( -4.771743288812468897, -279.1233781216988064, -337.9199732462171255 ) ) ;
#58208 = CARTESIAN_POINT ( 'NONE',  ( 175.2296996224750103, 250.5000000000000568, 24.50000000000000355 ) ) ;
#58209 = CARTESIAN_POINT ( 'NONE',  ( -65.22346980029674057, -286.7588089258796913, -202.5071288061722896 ) ) ;
#58210 = CARTESIAN_POINT ( 'NONE',  ( -37.99650225805415715, -287.8041885670105557, -194.3772693592969745 ) ) ;
#58211 = CARTESIAN_POINT ( 'NONE',  ( -13.26211249848714324, -288.0795226656879322, -339.3833327229949646 ) ) ;
#58212 = CARTESIAN_POINT ( 'NONE',  ( -108.5979489720030386, -276.7010437375448078, -289.5701631780463003 ) ) ;
#58213 = CARTESIAN_POINT ( 'NONE',  ( -99.14837876029218933, -286.9738533148823194, -229.2417799922106951 ) ) ;
#58214 = CARTESIAN_POINT ( 'NONE',  ( -105.0717616871353641, -277.4184846410717000, -241.3206890615510076 ) ) ;
#58215 = EDGE_CURVE ( 'NONE', #39726, #27101, #1162, .T. ) ;
#58216 = CARTESIAN_POINT ( 'NONE',  ( 1.143847806879024098, -277.8422096930956400, -333.0316737654466124 ) ) ;
#58217 = CARTESIAN_POINT ( 'NONE',  ( -1.698082109681582796, -275.0304308408280463, -206.5696738322164947 ) ) ;
#58218 = CARTESIAN_POINT ( 'NONE',  ( 37.71613785676404262, -286.5395197339906304, -285.6689485586093156 ) ) ;
#58219 = CARTESIAN_POINT ( 'NONE',  ( 39.36866596328303558, -282.4211365566412155, -275.6395980569988637 ) ) ;
#58220 = CARTESIAN_POINT ( 'NONE',  ( 17.78656414352937531, -282.7815930854620774, -324.1066213702296750 ) ) ;
#58221 = EDGE_LOOP ( 'NONE', ( #24290, #84005, #58222, #86071 ) ) ;
#58222 = ORIENTED_EDGE ( 'NONE', *, *, #65538, .T. ) ;
#58223 = CARTESIAN_POINT ( 'NONE',  ( -54.94434090351493438, -212.1443419142231051, 25.50000000000000000 ) ) ;
#58224 = CARTESIAN_POINT ( 'NONE',  ( -40.26696085343008491, -290.9489359918557625, -346.0823009421269489 ) ) ;
#58225 = CARTESIAN_POINT ( 'NONE',  ( -89.16978683164447261, -288.4482152006335127, -326.6385353037309187 ) ) ;
#58226 = CARTESIAN_POINT ( 'NONE',  ( -74.20133298768131169, -297.1333645920589106, -337.1120908320992839 ) ) ;
#58227 = CIRCLE ( 'NONE', #61263, 0.4999999999999935052 ) ;
#58228 = CARTESIAN_POINT ( 'NONE',  ( -51.59555791091181476, -272.9242197864306263, -198.4743806370645416 ) ) ;
#58229 = CARTESIAN_POINT ( 'NONE',  ( 19.34613559413926609, -292.1929228355894566, -218.4014983941503658 ) ) ;
#58230 = CARTESIAN_POINT ( 'NONE',  ( 20.04129323010142016, -286.6796297856447495, -316.5985468466306543 ) ) ;
#58231 = CARTESIAN_POINT ( 'NONE',  ( -37.53033859561809749, -290.2896533367708116, -196.3354047945619243 ) ) ;
#58232 = CARTESIAN_POINT ( 'NONE',  ( 33.04642829373552360, -288.4829575368902965, -249.5167688308048071 ) ) ;
#58233 = CARTESIAN_POINT ( 'NONE',  ( -20.25526795762937127, -288.7662352645560304, -195.3538533559490702 ) ) ;
#58234 = CARTESIAN_POINT ( 'NONE',  ( 2.149281404534636231, -290.5239512994888287, -334.1830368055075837 ) ) ;
#58235 = CARTESIAN_POINT ( 'NONE',  ( -107.7474599451786474, -288.8947816879293669, -243.8869396391374949 ) ) ;
#58236 = CARTESIAN_POINT ( 'NONE',  ( -73.06487903641890114, -293.5788905872786358, -204.4008426570613324 ) ) ;
#58237 = CARTESIAN_POINT ( 'NONE',  ( -108.8973677438136463, -285.6992358728543877, -254.7078203641029575 ) ) ;
#58238 = CARTESIAN_POINT ( 'NONE',  ( 37.61099674567384454, -295.4797054373212291, -264.6935209884815663 ) ) ;
#58239 = CARTESIAN_POINT ( 'NONE',  ( 198.5394373321410342, 68.65923120348695363, -9.381478303811002561 ) ) ;
#58240 = DIRECTION ( 'NONE',  ( 0.000000000000000000, 0.000000000000000000, 1.000000000000000000 ) ) ;
#58241 = CARTESIAN_POINT ( 'NONE',  ( -94.79046025150023524, -275.2039058364813968, -221.5760213046299327 ) ) ;
#58242 = AXIS2_PLACEMENT_3D ( 'NONE', #56797, #6592, #43032 ) ;
#58243 = CARTESIAN_POINT ( 'NONE',  ( 3.471842861263185309, -281.6852602607441440, -331.1418827868079120 ) ) ;
#58244 = CARTESIAN_POINT ( 'NONE',  ( -48.65483276734726559, -281.1960574157956785, -344.5029663300841776 ) ) ;
#58245 = CARTESIAN_POINT ( 'NONE',  ( -111.0633602407238669, -295.4764985487591389, -292.0703197071943578 ) ) ;
#58246 = CARTESIAN_POINT ( 'NONE',  ( -1.208604281813214998, -272.7783061427584812, -205.7526923375826868 ) ) ;
#58247 = CARTESIAN_POINT ( 'NONE',  ( -83.92659682963245871, -275.7771677919594708, -328.4891815762184706 ) ) ;
#58248 = CARTESIAN_POINT ( 'NONE',  ( -108.3162505107594740, -298.1181574629493412, -251.2375541694671313 ) ) ;
#58249 = CARTESIAN_POINT ( 'NONE',  ( -111.3244174429133153, -294.5716042925540705, -287.7533129690814917 ) ) ;
#58250 = CARTESIAN_POINT ( 'NONE',  ( -34.25848560582333846, -296.4379044670329790, -343.8857309122151378 ) ) ;
#58251 = CYLINDRICAL_SURFACE ( 'NONE', #5146, 2.842139515347646750 ) ;
#58252 = CLOSED_SHELL ( 'NONE', ( #92683, #58529, #90026, #25257, #82147, #87034, #77003, #41191, #43816, #59205, #67596, #52132, #31682, #31341, #15433, #72327, #17993, #66836, #30221, #41631, #18149, #4837, #5502, #24859, #86183, #51223, #21442, #76775, #45395, #13225, #66737, #13052, #43859, #77537, #70288, #84146, #53185, #52625, #10271, #38489, #56018, #13841, #10942, #29646, #62814, #90829, #14803, #72008, #28527, #38335, #56081, #79860, #64861, #1631, #83076, #59271, #28927, #22669, #76783, #68498, #85346, #38195, #74144, #58937, #85166, #32454, #75267, #44377, #42814, #52270, #30630, #4958, #6973, #92890, #21416, #48436, #46300, #37222, #40296, #7788, #63117, #91854, #3675, #2609, #38970, #63476, #48568, #16586, #82928, #52756, #61417, #71813, #50812, #54454, #68562, #42940, #1831, #17782, #87868, #56189, #2812, #7211, #10178, #63535, #54893, #30283, #48700, #72456, #1134, #85699, #52089, #2312, #75605, #13400, #68094, #8314, #53290, #40719, #1014, #1892, #31175, #67429, #32951, #13626, #45549, #27900, #6143, #8827, #64547, #30099, #59617, #36576, #61256, #90539, #71036, #55846, #77210, #69195, #84997, #76515, #76454, #20466, #63995, #73159, #24600, #81252, #92708, #32311, #89888, #40950, #41758, #30720, #42458, #55145, #66216, #35093, #65915, #47478, #93660, #24690, #92039, #53415, #70885, #58322, #20933, #35611, #84860, #23761, #40192, #53824, #58334, #58444, #77562, #34163, #53164, #2434, #87818, #39778, #83171, #74527, #71360, #52694, #19377, #47387, #35478, #60971, #34616, #36344, #89910, #47528, #58505, #78240, #20022, #23916, #7862, #23002, #58035, #37569, #29801, #32709, #15001, #49369, #18678, #78720, #36172, #87961, #17890, #60271, #10599, #8362, #31672, #60568, #32973, #54354, #15807, #52404, #26565, #28586, #1197, #45203, #24208, #34009, #63880, #69560, #69319, #10065, #2313, #68887, #46741, #55315, #54748, #84092, #5848, #84345, #39026, #84672, #37681, #25727, #70112, #26016, #77023, #85344, #60900, #17776, #60144, #56553, #3608, #17677, #55789, #45266, #74804, #3941, #86713, #87240, #84255, #84490, #81481, #252, #65384, #88007, #75532, #5978, #62812, #61198, #59259, #46843, #90425, #69403, #11435, #77948, #42691, #91502, #21708, #62569, #35201, #61331, #59744, #10468, #36645, #60323, #70920, #64764, #87985, #44278, #37625, #6358, #64359, #92926, #79887, #29347, #40830, #34937, #52105, #45119, #25673, #2438, #20581, #20670, #35229, #83283, #67083, #35412, #43303, #67333, #37647, #72625, #21564, #2508, #86068, #89714, #91293, #36378, #26437, #7209, #21734, #39537, #36468, #27856, #45040, #77757, #57151, #71464, #61972, #13104, #49426, #10404, #27767, #89310, #59198, #62917, #22100, #7668, #70518, #64114, #33097, #38716, #47143, #70036, #1421, #44517, #66466, #25489, #87693, #14921, #30229, #83034, #14701, #7949, #47870, #57272, #30159, #91186, #68020, #20124, #77049, #10542, #55676, #14279, #16836, #4299, #81856, #63762, #8974, #3883, #3670, #45140, #49758, #65467, #16602, #56168 ) ) ;
#58253 = CARTESIAN_POINT ( 'NONE',  ( -82.45135474656788688, -296.4888317288817916, -328.0253619373830247 ) ) ;
#58254 = DIRECTION ( 'NONE',  ( 0.000000000000000000, 0.000000000000000000, 1.000000000000000000 ) ) ;
#58256 = CARTESIAN_POINT ( 'NONE',  ( -86.48997559454481632, -295.7579594095685138, -324.3374740903284419 ) ) ;
#58255 = CARTESIAN_POINT ( 'NONE',  ( -46.28474187098094461, -283.9593236050528162, -195.5384689663494555 ) ) ;
#58257 = CARTESIAN_POINT ( 'NONE',  ( -85.51291023190965745, -285.4066929034167970, -210.2900391081729197 ) ) ;
#58258 = CARTESIAN_POINT ( 'NONE',  ( 20.52330978778046244, -284.1389681587759810, -318.9507756119650139 ) ) ;
#58259 = CARTESIAN_POINT ( 'NONE',  ( 37.69997151749419118, -287.0035354326991524, -253.1418385239699944 ) ) ;
#58260 = CARTESIAN_POINT ( 'NONE',  ( -37.52961080354226908, -290.0496729250559724, -195.5152595537584261 ) ) ;
#58261 = CARTESIAN_POINT ( 'NONE',  ( -79.81299671697057363, -278.6911714272116001, -206.2633394766397146 ) ) ;
#58262 = CARTESIAN_POINT ( 'NONE',  ( -4.829096099716524648, -274.1237833571632905, -337.9475929042657754 ) ) ;
#58263 = DIRECTION ( 'NONE',  ( -1.000000000000000000, 0.000000000000000000, -0.000000000000000000 ) ) ;
#58264 = CARTESIAN_POINT ( 'NONE',  ( 27.37336643614064258, -286.8178523263323427, -305.0971347635345978 ) ) ;
#58266 = CARTESIAN_POINT ( 'NONE',  ( 199.8757083317008494, 66.90342950747972850, -8.069961554617966826 ) ) ;
#58265 = CARTESIAN_POINT ( 'NONE',  ( -112.3347911955533220, -289.6747346766688906, -254.2515097302040488 ) ) ;
#58267 = LINE ( 'NONE', #8039, #47570 ) ;
#58268 = CARTESIAN_POINT ( 'NONE',  ( -99.39504528137669581, -297.6042929491894711, -310.4024476261736822 ) ) ;
#58269 = CARTESIAN_POINT ( 'NONE',  ( 16.79275225609071143, -282.2293584035601270, -216.3604446281086382 ) ) ;
#58271 = CARTESIAN_POINT ( 'NONE',  ( 25.15658005934236741, -280.6980527056792880, -232.5000114213190443 ) ) ;
#58270 = CARTESIAN_POINT ( 'NONE',  ( -93.44423988109707579, -293.8746576548170992, -320.6885192881327953 ) ) ;
#58272 = CARTESIAN_POINT ( 'NONE',  ( -64.26419870252848909, -295.5606178369052941, -342.5011143438870249 ) ) ;
#58273 = CARTESIAN_POINT ( 'NONE',  ( -1.628175471129533314, -284.6016003994726589, -203.7738943087226744 ) ) ;
#58274 = CARTESIAN_POINT ( 'NONE',  ( -111.2694996848005076, -280.7145634904664462, -257.7246191395745996 ) ) ;
#58275 = CARTESIAN_POINT ( 'NONE',  ( -88.28082168808782626, -296.3763200922820715, -217.6727039389922425 ) ) ;
#58276 = ORIENTED_EDGE ( 'NONE', *, *, #41871, .T. ) ;
#58277 = CARTESIAN_POINT ( 'NONE',  ( -23.74162510921650338, -284.8574079056663777, -343.7565181063085902 ) ) ;
#58278 = CARTESIAN_POINT ( 'NONE',  ( 85.55100297371598117, -298.0521521680024080, -417.1172536214571096 ) ) ;
#58279 = CARTESIAN_POINT ( 'NONE',  ( -54.42813229853333468, -289.3380690714489560, -195.3538533559490702 ) ) ;
#58280 = CARTESIAN_POINT ( 'NONE',  ( -41.17446446268515814, -273.2023711190662425, -193.5660932937568361 ) ) ;
#58281 = CARTESIAN_POINT ( 'NONE',  ( -77.25338171711713642, -291.3337096023544177, -209.2378190104927285 ) ) ;
#58282 = CARTESIAN_POINT ( 'NONE',  ( 20.20541809279164269, -282.4280167481900889, -224.3281196089028242 ) ) ;
#58283 = CARTESIAN_POINT ( 'NONE',  ( 5.626158736696218909, -276.2448270859183026, -210.2962727238852096 ) ) ;
#58284 = CARTESIAN_POINT ( 'NONE',  ( 35.71756369356082672, -283.4288389259120891, -292.1942368075359013 ) ) ;
#58285 = CARTESIAN_POINT ( 'NONE',  ( 36.08497729768387075, -280.3238216147161097, -268.5892202236719299 ) ) ;
#58286 = CARTESIAN_POINT ( 'NONE',  ( -112.3522940074298333, -280.5843480021209189, -267.8664730575142698 ) ) ;
#58287 = CARTESIAN_POINT ( 'NONE',  ( -14.81011945751415482, -298.3269540641308026, -193.3611147766884812 ) ) ;
#58288 = CARTESIAN_POINT ( 'NONE',  ( -1.299615256720735079, -274.3501664142771688, -202.3172488785206440 ) ) ;
#58289 = CARTESIAN_POINT ( 'NONE',  ( 37.14909936406689184, -295.4772581778345852, -270.7433852963139884 ) ) ;
#58290 = CARTESIAN_POINT ( 'NONE',  ( 160.5350683151633291, 215.0000000000000568, 20.22542485937379908 ) ) ;
#58291 = CARTESIAN_POINT ( 'NONE',  ( 208.6208076322478746, 32.98517505407394168, 10.50000000000000000 ) ) ;
#58292 = CARTESIAN_POINT ( 'NONE',  ( 29.79665691587037912, -292.1521233984457240, -305.4716077447148450 ) ) ;
#58293 = CARTESIAN_POINT ( 'NONE',  ( -65.83136517139847399, -273.1767455329260770, -203.0831317798035798 ) ) ;
#58294 = CARTESIAN_POINT ( 'NONE',  ( -16.83174482472171718, -293.8325048609812029, -196.8624820461997160 ) ) ;
#58296 = CARTESIAN_POINT ( 'NONE',  ( 27.70702231335044274, -294.2241103729919018, -229.8051125037101770 ) ) ;
#58295 = CARTESIAN_POINT ( 'NONE',  ( -69.91165696735023971, -282.1233781216988064, -202.8022627189028810 ) ) ;
#58297 = CARTESIAN_POINT ( 'NONE',  ( -59.20092442257989518, -291.3357502869835116, -341.9848071854732439 ) ) ;
#58298 = CARTESIAN_POINT ( 'NONE',  ( -105.0172135804407532, -276.9744033416577054, -238.3011358862991074 ) ) ;
#58299 = CARTESIAN_POINT ( 'NONE',  ( -18.63185683874331389, -278.7294627613449620, -342.4114889677319411 ) ) ;
#58300 = CARTESIAN_POINT ( 'NONE',  ( 30.79856729035514817, -292.0274114234154581, -300.3314057892122833 ) ) ;
#58301 = CARTESIAN_POINT ( 'NONE',  ( 18.88305533748748033, -284.1140494761307878, -321.2225697128147317 ) ) ;
#58302 = CIRCLE ( 'NONE', #50718, 5.103083949679981579 ) ;
#58303 = ORIENTED_EDGE ( 'NONE', *, *, #66289, .F. ) ;
#58304 = CARTESIAN_POINT ( 'NONE',  ( -61.54573377576387827, -283.0420229885423282, -339.3074201879663860 ) ) ;
#58305 = CARTESIAN_POINT ( 'NONE',  ( -1.292939957813983964, -281.5986279731169475, -202.6707981383232777 ) ) ;
#58306 = CARTESIAN_POINT ( 'NONE',  ( -37.32979979347020105, -281.8469005615052083, -346.9770435935736259 ) ) ;
#58307 = CARTESIAN_POINT ( 'NONE',  ( -38.52926204500557361, -278.0079491449293414, -347.1166383744142649 ) ) ;
#58308 = EDGE_CURVE ( 'NONE', #60290, #20083, #13866, .T. ) ;
#58309 = CARTESIAN_POINT ( 'NONE',  ( 0.7181685609744621335, -278.0747575706834027, -336.5584474768193672 ) ) ;
#58310 = CARTESIAN_POINT ( 'NONE',  ( -105.5937364680635966, -287.2662352645559167, -254.8156830097664738 ) ) ;
#58311 = ORIENTED_EDGE ( 'NONE', *, *, #51345, .F. ) ;
#58312 = CARTESIAN_POINT ( 'NONE',  ( -96.03189373401131945, -299.1941044660121634, -223.6657024873655928 ) ) ;
#58313 = CARTESIAN_POINT ( 'NONE',  ( -104.6242799427030974, -276.1431822857979910, -302.8057335621401194 ) ) ;
#58314 = CARTESIAN_POINT ( 'NONE',  ( -113.0001561734949718, -292.4086110728650283, -262.7608981482744639 ) ) ;
#58315 = CARTESIAN_POINT ( 'NONE',  ( 32.44163992935142460, -293.1888975920410871, -292.1367492862830773 ) ) ;
#58316 = CARTESIAN_POINT ( 'NONE',  ( -23.32930461582569137, -288.3853854432213666, -346.0668884496899409 ) ) ;
#58317 = CARTESIAN_POINT ( 'NONE',  ( 209.7827226070571385, 36.64741339240061535, 13.08022668053247983 ) ) ;
#58319 = CARTESIAN_POINT ( 'NONE',  ( -103.7412543665334965, -282.5193067332134547, -302.6894106360171577 ) ) ;
#58318 = CARTESIAN_POINT ( 'NONE',  ( -33.48288683644734931, -293.5792349356514706, -346.6874115249253805 ) ) ;
#58320 = CARTESIAN_POINT ( 'NONE',  ( -53.65733380765710336, -291.1241574246280379, -342.7811813286864435 ) ) ;
#58321 = CARTESIAN_POINT ( 'NONE',  ( -84.07272947292911169, -283.8765298433623343, -213.3130897672952528 ) ) ;
#58322 = ADVANCED_FACE ( 'NONE', ( #10112 ), #78874, .T. ) ;
#58323 = CARTESIAN_POINT ( 'NONE',  ( 20.57991198015645651, -283.5006407618025719, -315.5975007996236172 ) ) ;
#58324 = CARTESIAN_POINT ( 'NONE',  ( -114.0157034834198413, -291.4466031181196399, -274.0917240732396181 ) ) ;
#58325 = CARTESIAN_POINT ( 'NONE',  ( 17.10448985719286341, -281.3480500589778899, -221.6415034741993679 ) ) ;
#58326 = CARTESIAN_POINT ( 'NONE',  ( 27.76032930563117418, -292.8789244679813919, -310.8307130154411766 ) ) ;
#58327 = CARTESIAN_POINT ( 'NONE',  ( -51.64520337528083616, -290.0334952358699070, -345.8566053634414743 ) ) ;
#58328 = CARTESIAN_POINT ( 'NONE',  ( 39.28671753018082313, -288.1308634148895749, -277.2612998862767313 ) ) ;
#58329 = CARTESIAN_POINT ( 'NONE',  ( -22.46190960699132333, -286.4145475870277551, -198.8418196244562068 ) ) ;
#58330 = EDGE_LOOP ( 'NONE', ( #21872, #34669 ) ) ;
#58331 = FACE_OUTER_BOUND ( 'NONE', #83906, .T. ) ;
#58332 = CARTESIAN_POINT ( 'NONE',  ( -2.513844428382396412, -296.4568300006881145, -337.6465246511868372 ) ) ;
#58333 = CARTESIAN_POINT ( 'NONE',  ( -90.38233155883600034, -294.4685323130469214, -325.5701738207189919 ) ) ;
#58334 = ADVANCED_FACE ( 'NONE', ( #9648 ), #13721, .T. ) ;
#58335 = CARTESIAN_POINT ( 'NONE',  ( -108.1971956605758862, -277.8551845426517275, -251.7941372455289013 ) ) ;
#58336 = CARTESIAN_POINT ( 'NONE',  ( -93.12322679337654563, -272.7847640493824883, -217.3518174516033525 ) ) ;
#58337 = CARTESIAN_POINT ( 'NONE',  ( 1.923027429044345871, -292.9965976159466550, -332.7833032779283826 ) ) ;
#58338 = CARTESIAN_POINT ( 'NONE',  ( 21.47332155501657525, -276.6888042994611965, -225.4095706447155010 ) ) ;
#58339 = CARTESIAN_POINT ( 'NONE',  ( -111.4196221396391309, -270.7638995432500337, -264.7976786683124146 ) ) ;
#58340 = CARTESIAN_POINT ( 'NONE',  ( 35.93001590074437246, -294.6904849177667529, -265.2736132104790840 ) ) ;
#58341 = CARTESIAN_POINT ( 'NONE',  ( 35.92984866486841611, -294.6010057665943123, -268.0145864630187020 ) ) ;
#58342 = CARTESIAN_POINT ( 'NONE',  ( -43.30994550414099109, -271.7986277240285062, -432.4934747601029699 ) ) ;
#58343 = CARTESIAN_POINT ( 'NONE',  ( -103.6246451176777015, -295.0225600455010522, -234.8022235856830093 ) ) ;
#58344 = CARTESIAN_POINT ( 'NONE',  ( -33.34939872976709552, -298.7523158506616596, -193.4626218776420785 ) ) ;
#58345 = DIRECTION ( 'NONE',  ( -0.6250000000000095479, -0.000000000000000000, -0.7806247497997922391 ) ) ;
#58346 = CARTESIAN_POINT ( 'NONE',  ( -45.37639676859437543, -290.0977039935931430, -343.1543326239825547 ) ) ;
#58347 = CARTESIAN_POINT ( 'NONE',  ( -86.50107905408648890, -296.0911869259354603, -324.3559598687174343 ) ) ;
#58348 = CARTESIAN_POINT ( 'NONE',  ( -110.8040164433576535, -280.7465249094090609, -253.5773493502111364 ) ) ;
#58349 = CARTESIAN_POINT ( 'NONE',  ( -112.5837081757703686, -277.0616934021779798, -284.2873674300295193 ) ) ;
#58350 = ORIENTED_EDGE ( 'NONE', *, *, #3216, .F. ) ;
#58351 = CARTESIAN_POINT ( 'NONE',  ( -2.945886374331133428, -281.9582400045186432, -339.1524971229500807 ) ) ;
#58352 = CARTESIAN_POINT ( 'NONE',  ( 39.03533141284781038, -275.0182385929391558, -279.7437039210689704 ) ) ;
#58353 = CARTESIAN_POINT ( 'NONE',  ( -38.94004221035388014, -281.1521692368178265, -344.7966975744905653 ) ) ;
#58354 = CARTESIAN_POINT ( 'NONE',  ( -97.05712984982912417, -277.5921178540615983, -223.0271146448996546 ) ) ;
#58355 = CARTESIAN_POINT ( 'NONE',  ( 22.30836163735874322, -278.9268243332195425, -224.6028050068051982 ) ) ;
#58356 = CARTESIAN_POINT ( 'NONE',  ( -77.76937007875561392, -296.1818657568402386, -208.9253288462895739 ) ) ;
#58357 = CARTESIAN_POINT ( 'NONE',  ( 2.934614965450828894, -276.5925159262648663, -207.0330154259141864 ) ) ;
#58358 = DIRECTION ( 'NONE',  ( 0.000000000000000000, 1.000000000000000000, 0.000000000000000000 ) ) ;
#58359 = CARTESIAN_POINT ( 'NONE',  ( -33.59536954915453322, -290.1192024457285470, -195.0990969376645126 ) ) ;
#58360 = CARTESIAN_POINT ( 'NONE',  ( -46.02577120096609775, -289.1592547759493073, -346.9229821982838757 ) ) ;
#58361 = CARTESIAN_POINT ( 'NONE',  ( -69.37420419624034196, -275.6318797648829673, -202.3474349208476326 ) ) ;
#58362 = CARTESIAN_POINT ( 'NONE',  ( -37.80903230386057601, -296.0461271034363904, -195.5292395371845089 ) ) ;
#58363 = CARTESIAN_POINT ( 'NONE',  ( -112.0645266158754509, -283.5242046485086007, -288.3237726859858299 ) ) ;
#58364 = CARTESIAN_POINT ( 'NONE',  ( 152.4536156746142410, 275.0000000000000568, 14.50000000000000000 ) ) ;
#58365 = CARTESIAN_POINT ( 'NONE',  ( -73.13966234031319402, -283.5774948242063829, -204.4414870264439230 ) ) ;
#58366 = CARTESIAN_POINT ( 'NONE',  ( -41.60061644141435266, -290.7923801535328039, -197.0375931494471047 ) ) ;
#58367 = CARTESIAN_POINT ( 'NONE',  ( -96.74027365681310187, -283.3063994716749221, -225.8338797403751528 ) ) ;
#58368 = CARTESIAN_POINT ( 'NONE',  ( 41.08708295871279859, -486.4924983417995463, -507.6442049081570076 ) ) ;
#58369 = CARTESIAN_POINT ( 'NONE',  ( 33.70357676229919264, -291.2393223269993996, -246.1666149264316630 ) ) ;
#58370 = CARTESIAN_POINT ( 'NONE',  ( -106.3865933676369337, -282.6121198319348764, -302.8497385815358030 ) ) ;
#58371 = CARTESIAN_POINT ( 'NONE',  ( -51.41368808682262426, -278.8352365515879683, -342.8070948757865608 ) ) ;
#58372 = CARTESIAN_POINT ( 'NONE',  ( -91.63244968300998039, -286.5043490144807947, -216.3192524442690114 ) ) ;
#58373 = CARTESIAN_POINT ( 'NONE',  ( -108.3655117301545090, -284.7753603036408094, -253.4366518807889577 ) ) ;
#58374 = CARTESIAN_POINT ( 'NONE',  ( -24.20674488962405135, -278.3065669367290411, -342.8204983278910731 ) ) ;
#58375 = CARTESIAN_POINT ( 'NONE',  ( -110.0633499866582099, -279.2436668163700233, -278.8186138284518165 ) ) ;
#58376 = CARTESIAN_POINT ( 'NONE',  ( -68.97316281992121390, -287.6364293412214579, -202.3438063100544184 ) ) ;
#58377 = EDGE_LOOP ( 'NONE', ( #78012, #41504, #24595, #55165 ) ) ;
#58378 = CARTESIAN_POINT ( 'NONE',  ( -103.1166882382116228, -295.8627293820108548, -310.3942410634140288 ) ) ;
#58379 = CARTESIAN_POINT ( 'NONE',  ( 24.11818541854335152, -290.1092448805503068, -312.7455431087248030 ) ) ;
#58380 = DIRECTION ( 'NONE',  ( -0.000000000000000000, -1.000000000000000000, -0.000000000000000000 ) ) ;
#58381 = CARTESIAN_POINT ( 'NONE',  ( -37.30987171927208124, -279.5519495502701375, -350.3611179825600175 ) ) ;
#58382 = CARTESIAN_POINT ( 'NONE',  ( -111.5319239254870638, -277.2277796176067000, -289.8370487943196849 ) ) ;
#58383 = CARTESIAN_POINT ( 'NONE',  ( 28.79154415393354327, -291.4550830934755936, -232.5083186862884759 ) ) ;
#58384 = ADVANCED_FACE ( 'NONE', ( #11985 ), #90555, .F. ) ;
#58385 = CARTESIAN_POINT ( 'NONE',  ( 0.5083090456454590900, -288.0861827630913012, -207.0712265881521716 ) ) ;
#58386 = CARTESIAN_POINT ( 'NONE',  ( -108.9587208051619172, -280.5561409695507677, -251.6303671650568106 ) ) ;
#58387 = CARTESIAN_POINT ( 'NONE',  ( 21.62380842631358036, -288.3194165706153740, -221.7640491826302309 ) ) ;
#58388 = CARTESIAN_POINT ( 'NONE',  ( -81.79152836529674175, -285.6572679374419863, -330.8344369047159148 ) ) ;
#58389 = CARTESIAN_POINT ( 'NONE',  ( -100.4642887699044422, -278.1359051998626342, -314.4580431323665266 ) ) ;
#58390 = CARTESIAN_POINT ( 'NONE',  ( -108.0300300901720476, -270.8706271181288230, -245.8012231799324638 ) ) ;
#58391 = CARTESIAN_POINT ( 'NONE',  ( 35.69705332690548261, -291.3844836661102136, -250.9551376928707498 ) ) ;
#58392 = CARTESIAN_POINT ( 'NONE',  ( -36.75042222319528662, -279.8927125155788644, -193.3503426217190793 ) ) ;
#58393 = CARTESIAN_POINT ( 'NONE',  ( -97.29268955086435255, -275.0163984807197153, -226.4950400131153572 ) ) ;
#58394 = CARTESIAN_POINT ( 'NONE',  ( 189.9243309297870610, 250.5000000000000568, 25.22542485937350065 ) ) ;
#58395 = CARTESIAN_POINT ( 'NONE',  ( -106.6379572354042296, -286.6233781216988064, -303.7686719486574702 ) ) ;
#58396 = CARTESIAN_POINT ( 'NONE',  ( -82.95368798358974516, -271.6779514111104277, -209.5209363602475037 ) ) ;
#58397 = CYLINDRICAL_SURFACE ( 'NONE', #24316, 6.286090667950827715 ) ;
#58398 = CARTESIAN_POINT ( 'NONE',  ( -19.51347483645707825, -279.7952200927817330, -199.4558163882677206 ) ) ;
#58399 = CARTESIAN_POINT ( 'NONE',  ( 30.20024625159727094, -277.2279935711843564, -306.6130853767727444 ) ) ;
#58400 = CARTESIAN_POINT ( 'NONE',  ( -40.56177513122295153, -299.4361782809191936, -196.8297219094943955 ) ) ;
#58401 = CARTESIAN_POINT ( 'NONE',  ( -110.4650802941433625, -283.3157995425652302, -293.7666687723445875 ) ) ;
#58402 = CARTESIAN_POINT ( 'NONE',  ( 4.201671596619388716, -290.2442596623231452, -331.6774983679813431 ) ) ;
#58403 = CARTESIAN_POINT ( 'NONE',  ( -80.25128087289158429, -299.0030292917705310, -207.1986425440775861 ) ) ;
#58404 = CARTESIAN_POINT ( 'NONE',  ( -65.41087712666603693, -298.8984625365128522, -199.0293866496947999 ) ) ;
#58405 = CARTESIAN_POINT ( 'NONE',  ( 28.78986439202218861, -296.0189989776899893, -305.4954043938395216 ) ) ;
#58406 = CARTESIAN_POINT ( 'NONE',  ( -18.29294820875840344, -280.8060991768934400, -342.7831508123792901 ) ) ;
#58407 = CARTESIAN_POINT ( 'NONE',  ( -106.9409264893640739, -270.9264703521370734, -243.2409976749496536 ) ) ;
#58408 = CARTESIAN_POINT ( 'NONE',  ( -68.19570451451193094, -287.2538163752089986, -200.6728563515134738 ) ) ;
#58409 = CARTESIAN_POINT ( 'NONE',  ( 22.99653746753078210, -287.0501751632339165, -312.0188389156088533 ) ) ;
#58410 = CARTESIAN_POINT ( 'NONE',  ( 191.0571775945797413, 270.4395961937442507, -139.4957094208748742 ) ) ;
#58411 = ORIENTED_EDGE ( 'NONE', *, *, #66440, .T. ) ;
#58412 = CARTESIAN_POINT ( 'NONE',  ( -77.83962550829022575, -288.1591423404382226, -335.2188682935441193 ) ) ;
#58413 = CARTESIAN_POINT ( 'NONE',  ( -50.75951370256545658, -288.8948812734350895, -342.1905927832334555 ) ) ;
#58414 = ORIENTED_EDGE ( 'NONE', *, *, #41567, .T. ) ;
#58415 = CARTESIAN_POINT ( 'NONE',  ( -52.12721194931695834, -286.9469496106779047, -195.0548270488407354 ) ) ;
#58416 = CARTESIAN_POINT ( 'NONE',  ( 7.596744947866507225, -276.7530111416994032, -327.9809476184909727 ) ) ;
#58417 = CARTESIAN_POINT ( 'NONE',  ( 26.24772262053544125, -293.0396140204292124, -313.2315952860676020 ) ) ;
#58418 = CARTESIAN_POINT ( 'NONE',  ( -94.31804429160564496, -284.5008879551541554, -322.0237375709436947 ) ) ;
#58419 = EDGE_CURVE ( 'NONE', #21613, #28948, #53685, .T. ) ;
#58420 = CARTESIAN_POINT ( 'NONE',  ( 14.67442708935393547, -282.2884918934940970, -214.4585334762561502 ) ) ;
#58421 = CARTESIAN_POINT ( 'NONE',  ( -27.37063287721139915, -283.2621669158975806, -346.7448132276550155 ) ) ;
#58422 = CARTESIAN_POINT ( 'NONE',  ( -7.994842286096558226, -280.7807800616295140, -203.4830312952278746 ) ) ;
#58423 = CARTESIAN_POINT ( 'NONE',  ( -47.91463450998808327, -155.0658791552682771, -365.2963413022445138 ) ) ;
#58424 = CARTESIAN_POINT ( 'NONE',  ( -41.94452411973847461, -279.1104285115721382, -345.0656798433621475 ) ) ;
#58425 = CARTESIAN_POINT ( 'NONE',  ( 172.9411727994402099, 243.4788377357485842, -179.2791985832347450 ) ) ;
#58426 = CARTESIAN_POINT ( 'NONE',  ( -63.90417860558302010, -182.1577870710572427, -358.9045216547217478 ) ) ;
#58427 = CARTESIAN_POINT ( 'NONE',  ( -63.35460015881222517, -272.9015416359167148, -201.9668177545093783 ) ) ;
#58428 = CARTESIAN_POINT ( 'NONE',  ( -64.25054150048123347, -294.9016968972546238, -342.4405266870813875 ) ) ;
#58429 = CARTESIAN_POINT ( 'NONE',  ( 161.5460264286427901, 217.5614978313379027, -202.5778412181095121 ) ) ;
#58430 = CARTESIAN_POINT ( 'NONE',  ( -95.64096031508621820, -271.9093723775093281, -220.7980970025738543 ) ) ;
#58431 = CARTESIAN_POINT ( 'NONE',  ( -73.89024697504872563, -297.4035005713763553, -334.9758934172893419 ) ) ;
#58432 = CARTESIAN_POINT ( 'NONE',  ( 35.24893886790719932, -289.0188369879009542, -281.9237046592797356 ) ) ;
#58433 = EDGE_LOOP ( 'NONE', ( #70432, #16811, #6713, #47090 ) ) ;
#58434 = CARTESIAN_POINT ( 'NONE',  ( -16.55902372496308672, -295.7313776441777122, -344.3140911798018351 ) ) ;
#58435 = VECTOR ( 'NONE', #18328, 1000.000000000000000 ) ;
#58436 = CARTESIAN_POINT ( 'NONE',  ( -52.10749130080926506, -286.3503390200427248, -198.8072232422762227 ) ) ;
#58437 = CARTESIAN_POINT ( 'NONE',  ( -99.30912684682645875, -272.0756134916392170, -225.0897810305235680 ) ) ;
#58438 = CARTESIAN_POINT ( 'NONE',  ( 35.29660418142283618, -294.0366518311817003, -245.1434749720196464 ) ) ;
#58439 = CARTESIAN_POINT ( 'NONE',  ( 39.17656066855866470, -294.1511463385074876, -278.8818188403940894 ) ) ;
#58440 = CARTESIAN_POINT ( 'NONE',  ( -94.29224039994291218, -291.3644611793104104, -224.6724901682865720 ) ) ;
#58441 = EDGE_LOOP ( 'NONE', ( #34404, #71663 ) ) ;
#58442 = CARTESIAN_POINT ( 'NONE',  ( -32.79416743334270734, -276.0291597398052659, -194.9251785916763424 ) ) ;
#58443 = CARTESIAN_POINT ( 'NONE',  ( 25.01266335400542218, -273.7543836994849471, -225.8421324235300744 ) ) ;
#58444 = ADVANCED_FACE ( 'NONE', ( #26189 ), #33054, .T. ) ;
#58445 = ORIENTED_EDGE ( 'NONE', *, *, #35319, .T. ) ;
#58446 = CARTESIAN_POINT ( 'NONE',  ( -97.01064731726852131, -277.4073163381632980, -318.9527672941724745 ) ) ;
#58447 = CARTESIAN_POINT ( 'NONE',  ( 36.49894020260426686, -273.9684258395309371, -271.6187131300891906 ) ) ;
#58448 = CARTESIAN_POINT ( 'NONE',  ( -102.3107407040983645, -274.0933277833743773, -236.2915980912451346 ) ) ;
#58449 = CARTESIAN_POINT ( 'NONE',  ( 29.29517971762503592, -276.0836535979860855, -239.8586449463161046 ) ) ;
#58450 = CARTESIAN_POINT ( 'NONE',  ( -67.15893593552482344, -275.4266976211831093, -200.4690121049508775 ) ) ;
#58451 = EDGE_CURVE ( 'NONE', #65076, #50614, #45588, .T. ) ;
#58452 = CARTESIAN_POINT ( 'NONE',  ( -23.27128463348706688, -274.8933366422025983, -344.4440705731836943 ) ) ;
#58453 = CARTESIAN_POINT ( 'NONE',  ( -109.2408801439398900, -297.0286876214525478, -283.6365004408074242 ) ) ;
#58454 = CARTESIAN_POINT ( 'NONE',  ( -10.29015071914576218, -293.2667493695074654, -338.7978668247616270 ) ) ;
#58455 = CARTESIAN_POINT ( 'NONE',  ( 202.9738562182569694, 293.9636489450776367, -44.00000000000000000 ) ) ;
#58456 = CARTESIAN_POINT ( 'NONE',  ( -25.77302880867310364, -277.4008944307328761, -346.4248593249108126 ) ) ;
#58457 = CARTESIAN_POINT ( 'NONE',  ( -5.309972176139226896, -274.6524803298712527, -204.7502788534600029 ) ) ;
#58458 = CARTESIAN_POINT ( 'NONE',  ( -113.7172154232418251, -283.1701974516616929, -275.6667871009972828 ) ) ;
#58459 = CARTESIAN_POINT ( 'NONE',  ( -103.6486718138149996, -299.0222371873659881, -234.8470467293802812 ) ) ;
#58460 = CARTESIAN_POINT ( 'NONE',  ( 208.4939861239905667, 36.53598741959982732, 14.76870368707861481 ) ) ;
#58461 = CARTESIAN_POINT ( 'NONE',  ( 13.25860137813144846, -285.9786666956291583, -217.4498359795061617 ) ) ;
#58462 = CARTESIAN_POINT ( 'NONE',  ( -105.3646991354110867, -277.1785040204522375, -241.1918598979209207 ) ) ;
#58463 = CARTESIAN_POINT ( 'NONE',  ( -106.8265371811337445, -276.8052927607587321, -294.7486472775113953 ) ) ;
#58464 = CARTESIAN_POINT ( 'NONE',  ( -96.58657296726110530, -285.9215667679726494, -316.3711900782746511 ) ) ;
#58465 = CARTESIAN_POINT ( 'NONE',  ( 13.76218537912401452, -275.9933391362311568, -217.6778816511363743 ) ) ;
#58466 = DIRECTION ( 'NONE',  ( -1.000000000000000000, 0.000000000000000000, 0.000000000000000000 ) ) ;
#58467 = CARTESIAN_POINT ( 'NONE',  ( 20.20258887593741548, -274.6343452175885886, -320.3317878946602377 ) ) ;
#58468 = CARTESIAN_POINT ( 'NONE',  ( -89.79745371018157130, -281.3146599572119726, -216.4515332026948897 ) ) ;
#58469 = DIRECTION ( 'NONE',  ( 0.000000000000000000, 0.000000000000000000, 1.000000000000000000 ) ) ;
#58470 = CARTESIAN_POINT ( 'NONE',  ( -4.144497788464432730, -288.4065301653239430, -202.4700646369654748 ) ) ;
#58471 = CARTESIAN_POINT ( 'NONE',  ( 155.4202369374232262, 19.37982107812039700, -12.54055055082732295 ) ) ;
#58472 = CARTESIAN_POINT ( 'NONE',  ( 13.49681460457306237, -292.3407651114022769, -325.5707990135144883 ) ) ;
#58473 = CARTESIAN_POINT ( 'NONE',  ( 82.17345649163328858, -297.6224838372864951, -195.9197544271459606 ) ) ;
#58474 = CARTESIAN_POINT ( 'NONE',  ( 95.32732251205690943, -298.5441162442227210, -196.9920762313734599 ) ) ;
#58475 = CARTESIAN_POINT ( 'NONE',  ( -110.6424761585032144, -288.5383816393801908, -282.1826822617540529 ) ) ;
#58476 = CARTESIAN_POINT ( 'NONE',  ( -72.39245198575343920, -211.1690049852372226, -355.6323962662157783 ) ) ;
#58477 = CARTESIAN_POINT ( 'NONE',  ( 185.8264795993290477, 215.0000000000000568, 23.09031830825835385 ) ) ;
#58478 = CARTESIAN_POINT ( 'NONE',  ( -111.2553277063197044, -288.7920120299869495, -289.3734906542701424 ) ) ;
#58479 = CARTESIAN_POINT ( 'NONE',  ( -40.24565939529109215, -284.6893924604142967, -344.1039646674390724 ) ) ;
#58480 = CARTESIAN_POINT ( 'NONE',  ( -68.07015418690684783, -283.8940900190387993, -200.8506301183062703 ) ) ;
#58481 = CARTESIAN_POINT ( 'NONE',  ( -59.10521357335203163, -284.7645186904123875, -340.7120839882558130 ) ) ;
#58482 = CARTESIAN_POINT ( 'NONE',  ( -109.1359871761006985, -285.1696887219596874, -284.4388335167977289 ) ) ;
#58483 = CARTESIAN_POINT ( 'NONE',  ( -37.47286432276283108, -291.0336373613998830, -345.7290011042935589 ) ) ;
#58484 = CARTESIAN_POINT ( 'NONE',  ( -36.94410440113354355, -274.3903138879673520, -193.3702402195489469 ) ) ;
#58485 = CARTESIAN_POINT ( 'NONE',  ( -29.15790835359109323, -287.0292013679276693, -345.5291511015668107 ) ) ;
#58486 = CARTESIAN_POINT ( 'NONE',  ( 39.70739121345921774, -275.5622889030945544, -271.1716430989686160 ) ) ;
#58487 = CARTESIAN_POINT ( 'NONE',  ( -9.861535590313803112, -296.6713642364161956, -339.7634764462429189 ) ) ;
#58488 = CARTESIAN_POINT ( 'NONE',  ( 170.2305261370685798, 214.9910457053126720, -24.90909090909089940 ) ) ;
#58489 = CARTESIAN_POINT ( 'NONE',  ( -20.19161114001083490, -291.3376638359845856, -345.3538533559490702 ) ) ;
#58490 = CARTESIAN_POINT ( 'NONE',  ( -69.23824654133224499, -282.1656357340476688, -336.5856934696784606 ) ) ;
#58491 = CARTESIAN_POINT ( 'NONE',  ( -73.24414394369171077, -275.5268462595597612, -336.4139582406987188 ) ) ;
#58492 = CARTESIAN_POINT ( 'NONE',  ( -95.48669588160079513, -271.7044575634330954, -220.9257532575719551 ) ) ;
#58493 = CARTESIAN_POINT ( 'NONE',  ( 0.9177153736660982331, -275.8759394994144145, -332.7111206613425907 ) ) ;
#58494 = CARTESIAN_POINT ( 'NONE',  ( 33.28807357263086431, -294.7945328603215103, -249.1582423563963857 ) ) ;
#58495 = CARTESIAN_POINT ( 'NONE',  ( 30.06764308909870209, -294.1087670657261128, -241.6064579155074341 ) ) ;
#58496 = CARTESIAN_POINT ( 'NONE',  ( -77.61905349252327824, -287.2639421500850858, -208.2059445791758208 ) ) ;
#58497 = CARTESIAN_POINT ( 'NONE',  ( -3.598041709504797403, -293.9140065291185806, -201.7903531791220360 ) ) ;
#58498 = CARTESIAN_POINT ( 'NONE',  ( 35.81051696178221277, -294.5841558577627097, -247.9546142900702250 ) ) ;
#58499 = CARTESIAN_POINT ( 'NONE',  ( -110.3742152570091548, -296.4069778958614165, -268.7307783224857758 ) ) ;
#58500 = CARTESIAN_POINT ( 'NONE',  ( -37.24043142775248327, -291.0510410168107569, -345.3610539718976042 ) ) ;
#58501 = CARTESIAN_POINT ( 'NONE',  ( -8.036919884285145699, -282.8455554193877788, -341.6232045902410732 ) ) ;
#58502 = CARTESIAN_POINT ( 'NONE',  ( -38.31735470500477447, -272.1796342736362817, -194.6025964660167631 ) ) ;
#58503 = CARTESIAN_POINT ( 'NONE',  ( 38.55722148433031293, -287.2222308513680673, -257.3084199529279203 ) ) ;
#58504 = CARTESIAN_POINT ( 'NONE',  ( -64.91784471381103572, -279.3938877601074182, -339.7802786118872405 ) ) ;
#58505 = ADVANCED_FACE ( 'NONE', ( #3481 ), #39109, .T. ) ;
#58506 = CARTESIAN_POINT ( 'NONE',  ( -54.83618902055553690, -284.6172688549650616, -199.0268900767604521 ) ) ;
#58507 = CARTESIAN_POINT ( 'NONE',  ( 8.606103754259725847, -284.6815505852092087, -211.0838039067718341 ) ) ;
#58508 = CARTESIAN_POINT ( 'NONE',  ( -83.79068156146763613, -277.5621729979981751, -210.4382665843251630 ) ) ;
#58509 = CARTESIAN_POINT ( 'NONE',  ( 180.5468918863934960, 256.3577768311903355, -167.2605672291198857 ) ) ;
#58510 = CARTESIAN_POINT ( 'NONE',  ( -109.4808917354702942, -284.2133802210203726, -258.7092963028582631 ) ) ;
#58511 = CARTESIAN_POINT ( 'NONE',  ( 10.56267706767602554, -281.9018561384991131, -210.5170636391363814 ) ) ;
#58512 = CARTESIAN_POINT ( 'NONE',  ( 14.43613390439028699, -287.4040499083869236, -327.1065561166008138 ) ) ;
#58513 = CARTESIAN_POINT ( 'NONE',  ( -53.93696164439098339, -278.8617389779533937, -344.7861343549371895 ) ) ;
#58514 = CARTESIAN_POINT ( 'NONE',  ( -73.84670828488057737, -278.8416451607796489, -337.6120443397962276 ) ) ;
#58515 = CARTESIAN_POINT ( 'NONE',  ( -107.2265035552686641, -278.6647991774414095, -249.2633869563441067 ) ) ;
#58516 = CARTESIAN_POINT ( 'NONE',  ( -38.12434443258450045, -276.0221872799673406, -195.7204167890363351 ) ) ;
#58517 = CARTESIAN_POINT ( 'NONE',  ( 20.37869045009978919, -292.8618381384318923, -219.3769307577513530 ) ) ;
#58518 = CARTESIAN_POINT ( 'NONE',  ( 23.28316454167746485, -286.1676621772494400, -313.9096264323952141 ) ) ;
#58519 =( BOUNDED_CURVE ( )  B_SPLINE_CURVE ( 3, ( #34437, #85077, #27331, #34898 ),
 .UNSPECIFIED., .F., .F. ) 
 B_SPLINE_CURVE_WITH_KNOTS ( ( 4, 4 ),
 ( 3.665191429188093597, 4.712388980384689674 ),
 .UNSPECIFIED. ) 
 CURVE ( )  GEOMETRIC_REPRESENTATION_ITEM ( )  RATIONAL_B_SPLINE_CURVE ( ( 1.000000000000000000, 0.9106836025229593234, 0.9106836025229593234, 1.000000000000000000 ) ) 
 REPRESENTATION_ITEM ( '' )  );
#58520 = CARTESIAN_POINT ( 'NONE',  ( -25.16951929372627461, -293.8050023533035642, -195.1395889667691392 ) ) ;
#58521 = CARTESIAN_POINT ( 'NONE',  ( 32.63779622284481263, -292.7607085117251700, -292.2036490686687671 ) ) ;
#58522 = CARTESIAN_POINT ( 'NONE',  ( 6.072104311234774343, -294.1116789976222776, -329.1380894829464978 ) ) ;
#58523 =( BOUNDED_SURFACE ( )  B_SPLINE_SURFACE ( 3, 2, ( 
 ( #15255, #73490, #73938 ),
 ( #74397, #81042, #2453 ),
 ( #22814, #73019, #60216 ),
 ( #51683, #23286, #1055 ),
 ( #17589, #16641, #87664 ),
 ( #66388, #2902, #37030 ) ),
 .UNSPECIFIED., .F., .F., .F. ) 
 B_SPLINE_SURFACE_WITH_KNOTS ( ( 4, 2, 4 ),
 ( 3, 3 ),
 ( 4.712388980384689674, 5.132923315668655562, 5.553457650952622338 ),
 ( 0.000000000000000000, 1.000000000000000000 ),
 .UNSPECIFIED. ) 
 GEOMETRIC_REPRESENTATION_ITEM ( )  RATIONAL_B_SPLINE_SURFACE ( (
 ( 1.000000000000000000, 0.7071067811865487940, 1.000000000000000000),
 ( 1.000000000000000000, 0.7192895461638224575, 1.000000000000000000),
 ( 1.000000000000000000, 0.7311219824186969696, 1.000000000000000000),
 ( 1.000000000000000000, 0.7523130761999332616, 1.000000000000000000),
 ( 1.000000000000000000, 0.7616706333086389336, 1.000000000000000000),
 ( 1.000000000000000000, 0.7691239371209216413, 1.000000000000000000) ) ) 
 REPRESENTATION_ITEM ( '' )  SURFACE ( )  );
#58524 = CARTESIAN_POINT ( 'NONE',  ( -102.9585227589905685, -292.1531723257456861, -230.5607770174415805 ) ) ;
#58525 = CARTESIAN_POINT ( 'NONE',  ( 24.22075796338032916, -282.7492417371565807, -309.8744442351149928 ) ) ;
#58526 = CARTESIAN_POINT ( 'NONE',  ( -26.25142631353630662, -297.1082790415194950, -193.6722057268607671 ) ) ;
#58527 = CARTESIAN_POINT ( 'NONE',  ( -107.6348193458637326, -290.8036565344600035, -301.6720160924972447 ) ) ;
#58528 = CARTESIAN_POINT ( 'NONE',  ( -52.69091141803813372, -281.3862282238339958, -344.6084534189697592 ) ) ;
#58529 = ADVANCED_FACE ( 'NONE', ( #49832, #93390 ), #57887, .F. ) ;
#58530 = CARTESIAN_POINT ( 'NONE',  ( -60.01699755011050996, -289.6714918272361388, -343.9245272175650712 ) ) ;
#58531 = CARTESIAN_POINT ( 'NONE',  ( -52.09735192134409232, -286.1912986017371736, -198.8463766571815370 ) ) ;
#58532 = CARTESIAN_POINT ( 'NONE',  ( 5.216678999461890953, -58.13084686227820441, -354.5881712518272479 ) ) ;
#58533 = CARTESIAN_POINT ( 'NONE',  ( 166.1111599400100545, 232.1286469159066712, -191.2976056663461861 ) ) ;
#58534 = CARTESIAN_POINT ( 'NONE',  ( -97.95619041649757719, -246.4268646875643469, -331.2869283950922750 ) ) ;
#58535 = CARTESIAN_POINT ( 'NONE',  ( -110.1256530495713690, -277.8534005582075679, -262.4534283055543824 ) ) ;
#58536 = CARTESIAN_POINT ( 'NONE',  ( 9.484504338464780915, -279.6337342798196346, -213.8898574510124888 ) ) ;
#58537 = CARTESIAN_POINT ( 'NONE',  ( -29.83672130469200567, -273.8114249045856923, -193.7489806650517039 ) ) ;
#58538 = CARTESIAN_POINT ( 'NONE',  ( 123.0799137420843294, 147.2756895088847671, -261.2470527563303904 ) ) ;
#58539 = CARTESIAN_POINT ( 'NONE',  ( -36.73883383678317216, -278.6343241528004455, -193.9397768056164466 ) ) ;
#58540 = CARTESIAN_POINT ( 'NONE',  ( -29.29178007417424467, -280.9699065246471719, -344.6222300214747634 ) ) ;
#58541 = CARTESIAN_POINT ( 'NONE',  ( -66.51440299236104181, -297.1891122513745245, -340.5387068283817484 ) ) ;
#58542 = CARTESIAN_POINT ( 'NONE',  ( -52.38856171358685287, -292.3467078529504874, -198.8138550837406626 ) ) ;
#58543 = CARTESIAN_POINT ( 'NONE',  ( -92.79477947521067449, -288.5532671139583272, -318.6678811918050656 ) ) ;
#58544 = CARTESIAN_POINT ( 'NONE',  ( -30.49768110483991279, -298.6280333152058120, -193.4221014502348339 ) ) ;
#58545 = CARTESIAN_POINT ( 'NONE',  ( -104.7630216196258743, -297.0941618583510149, -242.3724521904902360 ) ) ;
#58546 = ORIENTED_EDGE ( 'NONE', *, *, #21848, .T. ) ;
#58547 = DIRECTION ( 'NONE',  ( 0.000000000000000000, 0.000000000000000000, 1.000000000000000000 ) ) ;
#58548 = CARTESIAN_POINT ( 'NONE',  ( -112.9436993789136778, -280.4563983155761093, -271.6094741629862597 ) ) ;
#58549 = EDGE_CURVE ( 'NONE', #11198, #89964, #57733, .T. ) ;
#58550 = CARTESIAN_POINT ( 'NONE',  ( 11.50158399539638232, -281.8285767952877450, -215.6933974442714543 ) ) ;
#58551 = CARTESIAN_POINT ( 'NONE',  ( -107.7094822790085686, -279.9432180013292850, -299.0377504007761900 ) ) ;
#58552 = CARTESIAN_POINT ( 'NONE',  ( -13.46394022879381858, -281.7932397158982099, -339.6482727907780941 ) ) ;
#58553 = CARTESIAN_POINT ( 'NONE',  ( -27.17555842637023389, -272.6634384562116793, -197.3209871789000545 ) ) ;
#58554 = DIRECTION ( 'NONE',  ( -1.000000000000000000, 0.000000000000000000, 0.000000000000000000 ) ) ;
#58555 = CARTESIAN_POINT ( 'NONE',  ( 155.0601170292804625, 20.95974790765943396, 14.78042489204666587 ) ) ;
#58557 = MANIFOLD_SOLID_BREP ( 'Shell2', #73378 ) ;
#58556 = CARTESIAN_POINT ( 'NONE',  ( 23.49870851570914354, -275.7270670020534453, -223.4078021316897491 ) ) ;
#58558 = ADVANCED_FACE ( 'NONE', ( #35649 ), #56976, .F. ) ;
#58559 = DIRECTION ( 'NONE',  ( 0.000000000000000000, 0.000000000000000000, -1.000000000000000000 ) ) ;
#58560 = CARTESIAN_POINT ( 'NONE',  ( 37.62553841112938358, -277.5980497989574474, -273.9229055294348996 ) ) ;
#58561 = CARTESIAN_POINT ( 'NONE',  ( -97.47651404494067151, -276.4918510350735232, -317.5035664825592221 ) ) ;
#58562 = ORIENTED_EDGE ( 'NONE', *, *, #76364, .F. ) ;
#58563 = DIRECTION ( 'NONE',  ( 0.000000000000000000, -1.000000000000000000, 0.000000000000000000 ) ) ;
#58564 = CARTESIAN_POINT ( 'NONE',  ( 6.000033185988877804, -284.4478194515640439, -332.0682771191629286 ) ) ;
#58565 = CARTESIAN_POINT ( 'NONE',  ( -96.88684040607151360, -290.3429516492303151, -227.7668782799815688 ) ) ;
#58566 = EDGE_CURVE ( 'NONE', #6460, #31, #18432, .T. ) ;
#58567 = CARTESIAN_POINT ( 'NONE',  ( -36.55812781050649107, -285.4103347906405475, -193.4540209268634783 ) ) ;
#58568 = CARTESIAN_POINT ( 'NONE',  ( -23.90319559126147553, -281.1179765025152619, -343.1442245866483631 ) ) ;
#58570 = CARTESIAN_POINT ( 'NONE',  ( 12.10855575273215656, -284.8256454208595869, -214.6502524807501402 ) ) ;
#58569 = CARTESIAN_POINT ( 'NONE',  ( -2.162823903857724162, -281.1515848506590487, -335.0115912743746662 ) ) ;
#58571 = CARTESIAN_POINT ( 'NONE',  ( 32.34880888967980894, -282.4512628904454914, -247.1714141487681502 ) ) ;
#58572 = CARTESIAN_POINT ( 'NONE',  ( -77.74220388725862563, -271.5094251216670500, -207.1725118625857931 ) ) ;
#58573 = CARTESIAN_POINT ( 'NONE',  ( -112.8100083746973468, -282.8141768368542444, -281.2689785234019269 ) ) ;
#58574 = CARTESIAN_POINT ( 'NONE',  ( -37.65439156176088886, -297.0561888963941328, -345.3732096272007652 ) ) ;
#58575 = CARTESIAN_POINT ( 'NONE',  ( -98.19578601263224016, -280.0585732387698386, -229.5256365944144363 ) ) ;
#58576 = CARTESIAN_POINT ( 'NONE',  ( -86.56897677220887033, -287.3706700716140858, -213.4881093479861249 ) ) ;
#58577 = DIRECTION ( 'NONE',  ( 0.000000000000000000, 1.000000000000000000, -0.000000000000000000 ) ) ;
#58578 = DIRECTION ( 'NONE',  ( 0.000000000000000000, 0.000000000000000000, 1.000000000000000000 ) ) ;
#58579 = CARTESIAN_POINT ( 'NONE',  ( 19.28303206256286728, -294.7816820182009678, -220.3120476382606228 ) ) ;
#58580 = CARTESIAN_POINT ( 'NONE',  ( -95.16380222357950913, -275.8927509602522150, -318.1473996638956123 ) ) ;
#58581 = CARTESIAN_POINT ( 'NONE',  ( 7.831303977691545626, -287.6500501471978168, -332.5842551510345970 ) ) ;
#58582 = CARTESIAN_POINT ( 'NONE',  ( 36.22024433781560049, -292.0293028138454474, -276.2840176252884703 ) ) ;
#58583 = CARTESIAN_POINT ( 'NONE',  ( -69.48210493171671942, -276.1690247434627281, -336.4676957458291895 ) ) ;
#58584 = CARTESIAN_POINT ( 'NONE',  ( -95.40283238755658601, -295.3341532651323291, -224.1034655898878611 ) ) ;
#58585 = CARTESIAN_POINT ( 'NONE',  ( -34.85727438330356875, -293.3991895667081735, -196.9099702185754097 ) ) ;
#58586 = CARTESIAN_POINT ( 'NONE',  ( 31.95455697924148097, -283.6233781216988064, -236.9535640164627353 ) ) ;
#58587 = DIRECTION ( 'NONE',  ( -0.4472135954999804652, 0.4472135955001954599, -0.7745966692413333021 ) ) ;
#58588 = CARTESIAN_POINT ( 'NONE',  ( -58.67620262530888908, -293.8029137561102857, -343.6797370096682585 ) ) ;
#58589 = CARTESIAN_POINT ( 'NONE',  ( 33.43143252167217128, -288.8779464051774539, -249.3975920073466170 ) ) ;
#58590 = CARTESIAN_POINT ( 'NONE',  ( -111.2819287127388037, -288.5693267298611318, -287.9330410642306219 ) ) ;
#58591 = CARTESIAN_POINT ( 'NONE',  ( 24.74513969528323543, -289.5192455207957778, -309.8655384630407639 ) ) ;
#58592 = DIRECTION ( 'NONE',  ( 0.000000000000000000, 0.000000000000000000, 1.000000000000000000 ) ) ;
#58593 = CARTESIAN_POINT ( 'NONE',  ( -34.56164648202492629, -289.8193032128233426, -343.5194473649704605 ) ) ;
#58594 = CYLINDRICAL_SURFACE ( 'NONE', #91155, 3.000000000000000000 ) ;
#58595 = CARTESIAN_POINT ( 'NONE',  ( 12.17092328126948964, -289.5858704919950810, -328.8120276471631200 ) ) ;
#58596 = CARTESIAN_POINT ( 'NONE',  ( -39.51402739835575062, -278.0451456051525838, -195.0244597577606100 ) ) ;
#58597 = CARTESIAN_POINT ( 'NONE',  ( -77.48511365191963307, -279.8627412386069295, -204.6164518453301469 ) ) ;
#58598 = CARTESIAN_POINT ( 'NONE',  ( 39.59853839682320853, -281.2493709843002989, -272.7991473443757400 ) ) ;
#58599 = CARTESIAN_POINT ( 'NONE',  ( 37.65485837510035338, -285.5612182998773960, -271.0800465722693389 ) ) ;
#58600 = CARTESIAN_POINT ( 'NONE',  ( -110.6019403019620171, -273.5598536869071609, -270.3739484367653745 ) ) ;
#58601 = CARTESIAN_POINT ( 'NONE',  ( -94.01815770130332339, -277.3619936420787440, -222.3973899133826251 ) ) ;
#58602 = CARTESIAN_POINT ( 'NONE',  ( -49.78737457124737631, -281.2106031406761417, -344.3737597120046985 ) ) ;
#58603 = DIRECTION ( 'NONE',  ( -0.3024135303179465439, -0.9531768234071978929, 0.000000000000000000 ) ) ;
#58604 = CARTESIAN_POINT ( 'NONE',  ( -84.45365961702597701, -276.1668855571060135, -330.4546906633462982 ) ) ;
#58605 = CARTESIAN_POINT ( 'NONE',  ( -96.04262244044051045, -282.8050836573171409, -319.7341946126602465 ) ) ;
#58606 = CARTESIAN_POINT ( 'NONE',  ( -108.0988892504093286, -273.6023889806285752, -251.5650875456485380 ) ) ;
#58607 = CARTESIAN_POINT ( 'NONE',  ( -113.7531456745012690, -274.0130566916598696, -267.5337022576003960 ) ) ;
#58608 = CARTESIAN_POINT ( 'NONE',  ( 16.54389171315690632, -275.9257658279097996, -319.6588741575004065 ) ) ;
#58609 = CARTESIAN_POINT ( 'NONE',  ( 9.496526050936175523, -296.4087377645370793, -329.0041672289834196 ) ) ;
#58610 = CARTESIAN_POINT ( 'NONE',  ( -89.48992366539307852, -289.9298306164640735, -327.0141213132939697 ) ) ;
#58611 = CARTESIAN_POINT ( 'NONE',  ( 14.19733570862872618, -278.8487698430856767, -215.0352322596864951 ) ) ;
#58612 = CARTESIAN_POINT ( 'NONE',  ( -70.89579604493113152, -291.4549373071619698, -201.0565535460021351 ) ) ;
#58613 = CARTESIAN_POINT ( 'NONE',  ( -42.69303489604784829, -288.1799223578173610, -343.4514063856719304 ) ) ;
#58614 = CARTESIAN_POINT ( 'NONE',  ( 5.451403755680182428, -292.4731416865045617, -332.0178163447873771 ) ) ;
#58615 = ORIENTED_EDGE ( 'NONE', *, *, #57902, .F. ) ;
#58616 = DIRECTION ( 'NONE',  ( 0.000000000000000000, 0.000000000000000000, 1.000000000000000000 ) ) ;
#58617 = CARTESIAN_POINT ( 'NONE',  ( -98.16537690546653039, -289.4981136238827162, -310.8619005052901230 ) ) ;
#58618 = CARTESIAN_POINT ( 'NONE',  ( 208.4306832106270804, -198.2391364535880598, 0.000000000000000000 ) ) ;
#58619 = CARTESIAN_POINT ( 'NONE',  ( -63.13369544164111602, -286.6655033851706094, -198.0590212603191276 ) ) ;
#58620 = CARTESIAN_POINT ( 'NONE',  ( -67.74223827176244583, -288.1233781216987495, -207.3071070584150277 ) ) ;
#58621 = CARTESIAN_POINT ( 'NONE',  ( 22.97931751020588464, -293.2480101418277627, -317.8605678744572742 ) ) ;
#58622 = CARTESIAN_POINT ( 'NONE',  ( 25.53465373807715721, -283.4470714877490423, -313.9715765906631759 ) ) ;
#58623 = CARTESIAN_POINT ( 'NONE',  ( -59.97661420160818579, -285.5838041910504330, -200.9589518104834553 ) ) ;
#58624 = CARTESIAN_POINT ( 'NONE',  ( 25.69022420480298408, -276.3497976632214659, -232.4707842078587419 ) ) ;
#58625 = CARTESIAN_POINT ( 'NONE',  ( -38.39012820922796720, -293.0854690731818550, -344.9985590232853951 ) ) ;
#58626 = CARTESIAN_POINT ( 'NONE',  ( -40.53833682900900470, -275.8881287627837082, -343.7010801597880914 ) ) ;
#58627 = ORIENTED_EDGE ( 'NONE', *, *, #50291, .F. ) ;
#58628 = CARTESIAN_POINT ( 'NONE',  ( 113.5000000000000568, -296.0521521680024080, -537.7509286889328450 ) ) ;
#58629 = CARTESIAN_POINT ( 'NONE',  ( -16.51668032641892481, -294.4570496281735927, -344.5247878499865237 ) ) ;
#58630 = CARTESIAN_POINT ( 'NONE',  ( -5.198574295426515945, -288.3985923036784129, -203.2044271127489026 ) ) ;
#58631 = CARTESIAN_POINT ( 'NONE',  ( -112.3001062314025091, -297.4282858397923519, -286.5700619827166520 ) ) ;
#58632 = CARTESIAN_POINT ( 'NONE',  ( -10.72057016878578040, -287.0601374721277352, -202.2652112457444673 ) ) ;
#58633 = CARTESIAN_POINT ( 'NONE',  ( -56.87576311536285090, -276.3567077033968644, -344.6537351831965452 ) ) ;
#58634 = CARTESIAN_POINT ( 'NONE',  ( -50.44198420407452232, -295.8664875174620761, -346.1889661637607674 ) ) ;
#58635 = CARTESIAN_POINT ( 'NONE',  ( 9.446252132475636998, -286.5567105174837934, -330.0197317783017752 ) ) ;
#58636 = CARTESIAN_POINT ( 'NONE',  ( 38.79625857030477221, -294.0273815859306978, -281.7081676768841021 ) ) ;
#58637 = PLANE ( 'NONE',  #91134 ) ;
#58638 = PLANE ( 'NONE',  #32667 ) ;
#58639 = CARTESIAN_POINT ( 'NONE',  ( 193.6786666067652618, 275.6390347797879485, -124.0807961620095767 ) ) ;
#58640 = CARTESIAN_POINT ( 'NONE',  ( -5.084794639619390821, -287.9892316847883649, -201.2076668493518810 ) ) ;
#58641 = CARTESIAN_POINT ( 'NONE',  ( -88.47809603358389552, -288.9094976428775681, -206.1857440867352693 ) ) ;
#58642 = VERTEX_POINT ( 'NONE', #42256 ) ;
#58643 = CARTESIAN_POINT ( 'NONE',  ( -94.88000257100489421, -278.5928676406996942, -219.3448799917398446 ) ) ;
#58644 = CARTESIAN_POINT ( 'NONE',  ( 35.10463050943396013, -283.7943648817204121, -289.1620979309058157 ) ) ;
#58645 = CARTESIAN_POINT ( 'NONE',  ( 204.9738562186072670, 293.9637359089629172, -68.56503966176641995 ) ) ;
#58646 = CARTESIAN_POINT ( 'NONE',  ( -108.4732631611209825, -283.4850257510628921, -242.3084064562328592 ) ) ;
#58647 = CARTESIAN_POINT ( 'NONE',  ( 21.48058208509784350, -286.2623387316310755, -316.0025022166556141 ) ) ;
#58648 = CARTESIAN_POINT ( 'NONE',  ( -38.36488130185693990, -275.8998640020965922, -194.6032234466659361 ) ) ;
#58649 = PRODUCT_DEFINITION_SHAPE ( 'NONE', 'NONE',  #69577 ) ;
#58650 = CARTESIAN_POINT ( 'NONE',  ( -108.8406547349348585, -297.2433762930133412, -255.2713699362329010 ) ) ;
#58651 = CARTESIAN_POINT ( 'NONE',  ( -0.5253180154882282071, -293.2370720750670898, -334.0257783518213728 ) ) ;
#58652 = CARTESIAN_POINT ( 'NONE',  ( -88.86929690035373142, -280.0018916324025895, -213.2803019653650267 ) ) ;
#58654 = CARTESIAN_POINT ( 'NONE',  ( -107.7141891568926297, -278.1625026371798413, -250.5257187786494342 ) ) ;
#58653 = CARTESIAN_POINT ( 'NONE',  ( -43.20708927548842837, -277.1282792697838886, -343.1251009009618542 ) ) ;
#58655 = CARTESIAN_POINT ( 'NONE',  ( -34.12995575822717598, -275.1713252126160114, -193.7375105987864856 ) ) ;
#58656 = CARTESIAN_POINT ( 'NONE',  ( 12.49328479277501458, -275.2967510603361916, -328.6531996647869960 ) ) ;
#58657 = CARTESIAN_POINT ( 'NONE',  ( 158.6539576904058606, 276.0000000000000568, 11.60392986742922616 ) ) ;
#58658 = CARTESIAN_POINT ( 'NONE',  ( 36.97544691305154174, -273.6863813148131044, -280.8278042308323279 ) ) ;
#58659 = CARTESIAN_POINT ( 'NONE',  ( -102.6028375552395744, -297.4544252039078742, -310.1051770813055555 ) ) ;
#58660 = DIRECTION ( 'NONE',  ( 0.000000000000000000, 0.000000000000000000, -1.000000000000000000 ) ) ;
#58661 = CARTESIAN_POINT ( 'NONE',  ( -109.0101294763935016, -268.7602059993127455, -295.2240039188629339 ) ) ;
#58662 = CARTESIAN_POINT ( 'NONE',  ( -22.41025438098025546, -287.3273920472772147, -198.5366155816941216 ) ) ;
#58663 = CARTESIAN_POINT ( 'NONE',  ( -110.8884383366877415, -286.0694397909495592, -289.5137248042375973 ) ) ;
#58664 = CARTESIAN_POINT ( 'NONE',  ( -46.72975171978337272, -285.2785392073601543, -197.8136710112836738 ) ) ;
#58665 = CARTESIAN_POINT ( 'NONE',  ( -101.4973222647122668, -277.4461919903855005, -233.8851455921334548 ) ) ;
#58666 = CARTESIAN_POINT ( 'NONE',  ( -79.05140265793581023, -285.4817698924738352, -331.7709396172847960 ) ) ;
#58667 = CARTESIAN_POINT ( 'NONE',  ( -46.52383406957923739, -278.4135240327029805, -197.1904769732057048 ) ) ;
#58668 = CARTESIAN_POINT ( 'NONE',  ( -7.368742320941616519, -277.7292432341420749, -337.2628957969927228 ) ) ;
#58669 = DIRECTION ( 'NONE',  ( 0.000000000000000000, 0.000000000000000000, 1.000000000000000000 ) ) ;
#58670 = CARTESIAN_POINT ( 'NONE',  ( 35.76051435095966724, -276.0605647392807214, -271.5797414414307696 ) ) ;
#58671 = CARTESIAN_POINT ( 'NONE',  ( 1.283936995486041344, -281.3567960196212994, -203.8760080598230218 ) ) ;
#58672 = CARTESIAN_POINT ( 'NONE',  ( 28.25581962852276519, -282.5713643484444901, -310.6677197834216599 ) ) ;
#58673 = VERTEX_POINT ( 'NONE', #50300 ) ;
#58674 = EDGE_LOOP ( 'NONE', ( #59728, #29494 ) ) ;
#58675 = DIRECTION ( 'NONE',  ( 1.000000000000000000, 0.000000000000000000, 0.000000000000000000 ) ) ;
#58676 = CARTESIAN_POINT ( 'NONE',  ( -51.43198739208584414, -291.0909083632765260, -344.8041786581816837 ) ) ;
#58677 = CARTESIAN_POINT ( 'NONE',  ( -98.64410457595269577, -288.6238502468863771, -316.1573824283742624 ) ) ;
#58678 = CARTESIAN_POINT ( 'NONE',  ( -105.9537099180454618, -296.0889554714380552, -244.8183167242063121 ) ) ;
#58679 = EDGE_CURVE ( 'NONE', #88979, #30715, #6298, .T. ) ;
#58680 = CARTESIAN_POINT ( 'NONE',  ( -70.84579838389640827, -290.9702826215589084, -201.1455981385965686 ) ) ;
#58681 = CARTESIAN_POINT ( 'NONE',  ( 14.55807695652621270, -286.7851824383562303, -322.6786187862156225 ) ) ;
#58682 = VECTOR ( 'NONE', #33418, 1000.000000000000000 ) ;
#58683 = CARTESIAN_POINT ( 'NONE',  ( 35.35578512918814909, -288.8910776122786501, -280.5624664279043827 ) ) ;
#58684 = CARTESIAN_POINT ( 'NONE',  ( -106.6379572354042296, -292.6233781216987495, -303.7686719486574702 ) ) ;
#58685 = CARTESIAN_POINT ( 'NONE',  ( 31.05176525278180577, -289.9559266763461096, -301.1399181365704862 ) ) ;
#58686 = CARTESIAN_POINT ( 'NONE',  ( -41.68080614407671902, -287.1065093820386664, -345.4153511425020611 ) ) ;
#58687 = CARTESIAN_POINT ( 'NONE',  ( -107.9849569948173382, -285.2385268511987420, -289.7200563243366105 ) ) ;
#58688 = CARTESIAN_POINT ( 'NONE',  ( -106.0450824460865675, -292.1521867671137329, -300.9828664745254514 ) ) ;
#58689 = CARTESIAN_POINT ( 'NONE',  ( 82.16214272339226454, -298.5110651170496112, -193.6458011586250620 ) ) ;
#58690 = CARTESIAN_POINT ( 'NONE',  ( 196.0143093133015384, 42.36571313990103249, 11.99999999999998757 ) ) ;
#58691 = CARTESIAN_POINT ( 'NONE',  ( -33.45209830827303676, -300.0206301958165795, -194.7998491850339349 ) ) ;
#58692 = CARTESIAN_POINT ( 'NONE',  ( 14.03080343361200910, -281.5058699449105006, -322.5233926421246906 ) ) ;
#58693 = CARTESIAN_POINT ( 'NONE',  ( -104.8230045105705557, -282.1193390145845115, -303.2107995657173660 ) ) ;
#58694 = CARTESIAN_POINT ( 'NONE',  ( 34.29724498811630440, -293.1020786641420841, -298.1463723948273810 ) ) ;
#58695 = CARTESIAN_POINT ( 'NONE',  ( -107.2563597055038969, -271.1106076826631011, -246.0729647200678869 ) ) ;
#58696 = CARTESIAN_POINT ( 'NONE',  ( 35.57016313946201080, -273.8261203508047288, -285.3669300508146875 ) ) ;
#58697 = CARTESIAN_POINT ( 'NONE',  ( -110.2918884991095609, -297.7451608369148062, -279.6849122192661525 ) ) ;
#58698 = FACE_OUTER_BOUND ( 'NONE', #63874, .T. ) ;
#58699 = CARTESIAN_POINT ( 'NONE',  ( -36.92458206176511482, -272.6320452602067235, -193.9385305194504951 ) ) ;
#58700 = CARTESIAN_POINT ( 'NONE',  ( -107.9387177782732010, -295.1549413519128393, -242.1122626865557095 ) ) ;
#58701 = CARTESIAN_POINT ( 'NONE',  ( -20.69739856007482004, -296.2596851056119931, -342.0958768259982321 ) ) ;
#58702 = DIRECTION ( 'NONE',  ( 0.000000000000000000, 0.000000000000000000, 1.000000000000000000 ) ) ;
#58703 = CARTESIAN_POINT ( 'NONE',  ( -41.03717211239619900, -295.9026467098473177, -343.4417992770300998 ) ) ;
#58704 = CARTESIAN_POINT ( 'NONE',  ( -112.3417001280820386, -272.5521521680024648, -270.3611179825637691 ) ) ;
#58706 = CARTESIAN_POINT ( 'NONE',  ( -95.28906866339589499, -297.1769671618695838, -225.9436502477421129 ) ) ;
#58705 = CARTESIAN_POINT ( 'NONE',  ( -112.7106217909955319, -282.5414612805869865, -272.7709295338436277 ) ) ;
#58707 = CARTESIAN_POINT ( 'NONE',  ( -112.9982418408954885, -284.7346790332960040, -255.7628116991040201 ) ) ;
#58708 = CARTESIAN_POINT ( 'NONE',  ( -24.74903386559984497, -284.8129953649403774, -344.9175061051861348 ) ) ;
#58709 = AXIS2_PLACEMENT_3D ( 'NONE', #66771, #44516, #17043 ) ;
#58710 = CARTESIAN_POINT ( 'NONE',  ( 39.32600644743844498, -287.3053680525313780, -277.2753829408665069 ) ) ;
#58711 = CARTESIAN_POINT ( 'NONE',  ( -32.00166042297281166, -290.1194948919369949, -195.7056164148254709 ) ) ;
#58712 = CARTESIAN_POINT ( 'NONE',  ( -112.8356090845500574, -277.9295698575354550, -255.9789674237104009 ) ) ;
#58713 = CARTESIAN_POINT ( 'NONE',  ( -4.829096099716524648, -280.1237833571632336, -337.9475929042657754 ) ) ;
#58714 = CARTESIAN_POINT ( 'NONE',  ( -48.18343439338448775, -253.8987417476172368, -491.5047106340448977 ) ) ;
#58715 = CARTESIAN_POINT ( 'NONE',  ( -5.613176773358834915, -285.2738687217776601, -204.1624310261117330 ) ) ;
#58716 = CARTESIAN_POINT ( 'NONE',  ( -111.6260730152491192, -289.2323913693102782, -289.4747624125574816 ) ) ;
#58717 = DIRECTION ( 'NONE',  ( 1.000000000000000000, 0.000000000000000000, 0.000000000000000000 ) ) ;
#58718 = CARTESIAN_POINT ( 'NONE',  ( -110.8490849169315169, -298.2451752035632921, -263.2425357576393026 ) ) ;
#58719 = CARTESIAN_POINT ( 'NONE',  ( -112.6587840659604183, -280.1397681681479526, -257.4792252402149870 ) ) ;
#58721 = CARTESIAN_POINT ( 'NONE',  ( 32.25017604882551581, -281.5139557742043053, -292.6404277766109203 ) ) ;
#58720 = CARTESIAN_POINT ( 'NONE',  ( -33.54350951435366568, -293.0247046419877393, -345.6333789947981359 ) ) ;
#58722 = CARTESIAN_POINT ( 'NONE',  ( -41.94343917727029947, -295.2751768993224459, -347.2758820249123346 ) ) ;
#58723 = CARTESIAN_POINT ( 'NONE',  ( 8.948227545833848495, -284.7615441348500553, -210.6404616641188170 ) ) ;
#58724 = CARTESIAN_POINT ( 'NONE',  ( -71.61615328812959547, -281.5995509780946691, -203.6365573256980781 ) ) ;
#58725 = CARTESIAN_POINT ( 'NONE',  ( -41.06312668853401959, -294.1588438930530174, -343.5144081940376850 ) ) ;
#58726 = VERTEX_POINT ( 'NONE', #70703 ) ;
#58727 = FACE_BOUND ( 'NONE', #30005, .T. ) ;
#58728 = CARTESIAN_POINT ( 'NONE',  ( 33.53049388703569633, -283.2259544132777478, -246.7680799888565844 ) ) ;
#58729 = CARTESIAN_POINT ( 'NONE',  ( -110.2733433894352686, -296.1171999221894566, -266.0063673927788841 ) ) ;
#58730 = FACE_OUTER_BOUND ( 'NONE', #82938, .T. ) ;
#58731 = CARTESIAN_POINT ( 'NONE',  ( -85.28047601435909542, -276.9094976428776249, -210.1954327657594206 ) ) ;
#58732 = CARTESIAN_POINT ( 'NONE',  ( -46.85086058707742040, -273.1314872313794240, -194.1132676026062427 ) ) ;
#58733 = ADVANCED_FACE ( 'NONE', ( #79206 ), #35167, .T. ) ;
#58734 = EDGE_CURVE ( 'NONE', #68290, #307, #6365, .T. ) ;
#58735 = CARTESIAN_POINT ( 'NONE',  ( -94.28957238991719692, -291.0311551039254709, -224.6691645873775940 ) ) ;
#58736 = CARTESIAN_POINT ( 'NONE',  ( -95.34849404617020241, -280.7072726407316168, -224.8884114915677515 ) ) ;
#58737 = CARTESIAN_POINT ( 'NONE',  ( -0.1606389987241754747, -276.1556905325818434, -206.5967880756469128 ) ) ;
#58738 = CARTESIAN_POINT ( 'NONE',  ( 11.00096335931202063, -283.9964246375881203, -329.3312574431718645 ) ) ;
#58739 = CARTESIAN_POINT ( 'NONE',  ( -2.252258150526716296, -281.3717458410600329, -334.8414557679255950 ) ) ;
#58740 = CARTESIAN_POINT ( 'NONE',  ( -39.18198955426010599, -279.0754116970554151, -345.3385411640683174 ) ) ;
#58741 = ORIENTED_EDGE ( 'NONE', *, *, #21988, .T. ) ;
#58742 = CARTESIAN_POINT ( 'NONE',  ( -24.15751981521545488, -274.0492385822398660, -194.4440659278375563 ) ) ;
#58743 = CARTESIAN_POINT ( 'NONE',  ( 2.358090243491804294, -296.4363192216363814, -333.3923367251136369 ) ) ;
#58744 = CARTESIAN_POINT ( 'NONE',  ( 201.2104617360081704, 60.19600395700752671, -9.000000000000000000 ) ) ;
#58745 = DIRECTION ( 'NONE',  ( 0.000000000000000000, 1.000000000000000000, 0.000000000000000000 ) ) ;
#58746 = CARTESIAN_POINT ( 'NONE',  ( 36.57356121965458584, -291.9039657184482621, -287.0580946508957254 ) ) ;
#58747 = AXIS2_PLACEMENT_3D ( 'NONE', #52382, #67074, #59980 ) ;
#58748 = CARTESIAN_POINT ( 'NONE',  ( -69.51241316975526274, -273.1245046829878902, -204.7636053447631923 ) ) ;
#58749 = FACE_OUTER_BOUND ( 'NONE', #71330, .T. ) ;
#58750 = CARTESIAN_POINT ( 'NONE',  ( -22.34913209683123725, -293.7607615265937397, -195.4879632618886092 ) ) ;
#58752 = CARTESIAN_POINT ( 'NONE',  ( -73.26117819295754430, -292.7917612346524265, -202.6868537666159682 ) ) ;
#58751 = CARTESIAN_POINT ( 'NONE',  ( -69.85430415644619018, -279.9805209788416391, -337.9475929042657754 ) ) ;
#58753 = CARTESIAN_POINT ( 'NONE',  ( -0.05642167294575807512, -290.5553912146856987, -335.3040271737373246 ) ) ;
#58754 = CARTESIAN_POINT ( 'NONE',  ( 37.20693045233825558, -273.4607588499176813, -263.2717800785143822 ) ) ;
#58755 = CARTESIAN_POINT ( 'NONE',  ( -77.10474928617466617, -279.5092683629496833, -333.3519622508209181 ) ) ;
#58756 = CARTESIAN_POINT ( 'NONE',  ( 35.73339942444705741, -291.8155604207780129, -284.5506925276579864 ) ) ;
#58757 = CARTESIAN_POINT ( 'NONE',  ( -28.39476240270343510, -282.0247845828132540, -195.0736700449982379 ) ) ;
#58758 = ORIENTED_EDGE ( 'NONE', *, *, #9285, .T. ) ;
#58759 = CARTESIAN_POINT ( 'NONE',  ( -53.69853189574080687, -282.9344640767532724, -341.5788105460835027 ) ) ;
#58760 = CARTESIAN_POINT ( 'NONE',  ( -96.58744848056015542, -280.2887644847710362, -221.6433232711877110 ) ) ;
#58761 = CARTESIAN_POINT ( 'NONE',  ( -10.85381177139242403, -281.5093827006601828, -342.2951447254273489 ) ) ;
#58762 = CARTESIAN_POINT ( 'NONE',  ( -97.73634555628086673, -278.8579922585502686, -317.7457886862556506 ) ) ;
#58763 = DIRECTION ( 'NONE',  ( 0.000000000000000000, 0.000000000000000000, 1.000000000000000000 ) ) ;
#58764 = CARTESIAN_POINT ( 'NONE',  ( 27.07403079322463668, -277.6143581862805831, -311.3656259189516504 ) ) ;
#58765 = CARTESIAN_POINT ( 'NONE',  ( -21.33282851196159058, -285.3376638359844719, -340.3538533559490702 ) ) ;
#58766 = ORIENTED_EDGE ( 'NONE', *, *, #45672, .F. ) ;
#58767 = ORIENTED_EDGE ( 'NONE', *, *, #36940, .F. ) ;
#58768 = CARTESIAN_POINT ( 'NONE',  ( -50.32449358500621628, -299.8865635524892923, -196.4933461189164632 ) ) ;
#58769 = CARTESIAN_POINT ( 'NONE',  ( -68.75199337118469600, -275.4871800172071516, -338.0895803231078389 ) ) ;
#58770 = CARTESIAN_POINT ( 'NONE',  ( -111.2715053261624973, -292.0890388265043498, -287.9768470182414717 ) ) ;
#58771 = CARTESIAN_POINT ( 'NONE',  ( -20.04000514735208327, -291.6288750002951247, -199.2838207606529863 ) ) ;
#58772 = CARTESIAN_POINT ( 'NONE',  ( 19.57449628544570430, -287.7641381107038683, -322.1501660396597231 ) ) ;
#58773 = DIRECTION ( 'NONE',  ( 0.8435586647355688417, 0.000000000000000000, -0.5370370370370596280 ) ) ;
#58775 = CARTESIAN_POINT ( 'NONE',  ( -83.30875802780741424, -282.0935637074011879, -328.1629184752833339 ) ) ;
#58774 = CARTESIAN_POINT ( 'NONE',  ( 38.64224064724579222, -292.0191144916779535, -261.8100281653390766 ) ) ;
#58776 = CARTESIAN_POINT ( 'NONE',  ( -95.91071519575355353, -291.7803499911562426, -315.9945386638127047 ) ) ;
#58777 = CARTESIAN_POINT ( 'NONE',  ( -97.91490516879137829, -283.6115695659032099, -228.3674661123548049 ) ) ;
#58778 = CARTESIAN_POINT ( 'NONE',  ( 28.60090835284257338, -283.3054247765423383, -302.9237864254142210 ) ) ;
#58779 = CARTESIAN_POINT ( 'NONE',  ( -87.22241725032165505, -290.6685511483703976, -328.7810283087312655 ) ) ;
#58780 = CARTESIAN_POINT ( 'NONE',  ( 20.56085653619570763, -281.4177116615019827, -225.7842793140839888 ) ) ;
#58781 = CARTESIAN_POINT ( 'NONE',  ( 13.02897779753327079, -291.5326502509920488, -212.6480040234442299 ) ) ;
#58782 = CARTESIAN_POINT ( 'NONE',  ( -2.305675900842721227, -287.3066541688756956, -201.9604641642754359 ) ) ;
#58783 = CARTESIAN_POINT ( 'NONE',  ( 35.78857806957747556, -287.7415676724920104, -246.2849360227185116 ) ) ;
#58784 = CARTESIAN_POINT ( 'NONE',  ( -57.39642358597571103, -285.9528206369439545, -200.1172791368904313 ) ) ;
#58785 = ORIENTED_EDGE ( 'NONE', *, *, #54006, .F. ) ;
#58786 = CARTESIAN_POINT ( 'NONE',  ( 194.9126400680597442, 26.32064278049061912, 13.74612429362717769 ) ) ;
#58787 = CARTESIAN_POINT ( 'NONE',  ( 8.183167501695949753, -296.2972575327050890, -330.9234157028564596 ) ) ;
#58788 = CARTESIAN_POINT ( 'NONE',  ( -113.7424321250618249, -295.1749299433818692, -275.2907988800445196 ) ) ;
#58789 = CARTESIAN_POINT ( 'NONE',  ( -105.4911208791931330, -277.2534491571777835, -297.1765034712289548 ) ) ;
#58790 = CARTESIAN_POINT ( 'NONE',  ( -37.59898510129450955, -297.3976003181313672, -193.4634808821086267 ) ) ;
#58791 = CARTESIAN_POINT ( 'NONE',  ( 19.89643698911766023, -291.3813244230000805, -223.9245243118323287 ) ) ;
#58792 = CARTESIAN_POINT ( 'NONE',  ( -6.121646524917198740, -276.2283127508886196, -203.2546185259684250 ) ) ;
#58793 = CARTESIAN_POINT ( 'NONE',  ( -106.9477354740237445, -294.4596834732561774, -295.6709159691966988 ) ) ;
#58794 = CARTESIAN_POINT ( 'NONE',  ( 16.46059319169603441, -295.4708789818221817, -320.2854981851360776 ) ) ;
#58795 = CARTESIAN_POINT ( 'NONE',  ( 1.746232537962481013, -295.5959720133897690, -332.4402717917050154 ) ) ;
#58796 = DIRECTION ( 'NONE',  ( 0.000000000000000000, 0.000000000000000000, 1.000000000000000000 ) ) ;
#58797 = CARTESIAN_POINT ( 'NONE',  ( -78.49503503040311614, -293.6046204367660835, -333.2612885011664048 ) ) ;
#58798 = CARTESIAN_POINT ( 'NONE',  ( -107.1689386346646131, -298.9101366648176850, -242.8500217586268377 ) ) ;
#58799 = CARTESIAN_POINT ( 'NONE',  ( -105.3270168392380697, -291.1285187111868140, -297.7259222133938579 ) ) ;
#58800 = CARTESIAN_POINT ( 'NONE',  ( -88.51363961834874772, -296.1270039214653025, -322.5236324848327740 ) ) ;
#58801 = CARTESIAN_POINT ( 'NONE',  ( -103.5188299238998297, -280.0554358438674285, -306.4026813794088184 ) ) ;
#58802 = CARTESIAN_POINT ( 'NONE',  ( -94.58163516429823403, -277.9292140568590526, -219.5980594611044694 ) ) ;
#58803 = ORIENTED_EDGE ( 'NONE', *, *, #1737, .F. ) ;
#58804 = CARTESIAN_POINT ( 'NONE',  ( -97.72786026384194713, -272.5383926024172183, -222.7499380851481021 ) ) ;
#58805 = CARTESIAN_POINT ( 'NONE',  ( 1.838847016384126176, -280.6038627548596764, -333.7158386789578799 ) ) ;
#58806 = CARTESIAN_POINT ( 'NONE',  ( -111.6173244878300466, -277.1670840823454114, -253.3443014483818274 ) ) ;
#58807 = CARTESIAN_POINT ( 'NONE',  ( -40.89560963756561307, -278.0074011126604887, -195.2656276319985693 ) ) ;
#58808 = CARTESIAN_POINT ( 'NONE',  ( -110.9309288753746898, -271.1271092316917475, -270.3430129928519818 ) ) ;
#58809 = CARTESIAN_POINT ( 'NONE',  ( 26.16589086450915147, -277.0148976564033205, -230.3685084577820703 ) ) ;
#58810 = VECTOR ( 'NONE', #121, 1000.000000000000114 ) ;
#58811 = CARTESIAN_POINT ( 'NONE',  ( 170.2297021224755724, 215.0000000000000568, -25.00499999999998835 ) ) ;
#58812 = CARTESIAN_POINT ( 'NONE',  ( -110.0392043883640554, -288.8266985274099170, -250.4758942532522781 ) ) ;
#58813 = CARTESIAN_POINT ( 'NONE',  ( -69.35730438698212197, -289.4618734955298578, -340.4041149107267756 ) ) ;
#58814 = CARTESIAN_POINT ( 'NONE',  ( 16.75210782339269855, -276.8195081143772427, -218.0955442132021744 ) ) ;
#58815 = CARTESIAN_POINT ( 'NONE',  ( -35.74177478704485367, -296.0720672345574940, -195.5283229024749687 ) ) ;
#58816 = CARTESIAN_POINT ( 'NONE',  ( -46.47613981931052507, -285.1361935216064012, -194.0674692839361342 ) ) ;
#58817 = CARTESIAN_POINT ( 'NONE',  ( 175.2296996224749250, 250.0000000000000568, -24.99999999999999289 ) ) ;
#58818 = CARTESIAN_POINT ( 'NONE',  ( 33.32110402717074038, -279.8794175166545983, -295.6474551530456552 ) ) ;
#58819 = CARTESIAN_POINT ( 'NONE',  ( -54.94434090351493438, -212.1443419142231051, 25.50000000000000000 ) ) ;
#58820 = CARTESIAN_POINT ( 'NONE',  ( 27.84619894006351259, -291.8908784391032896, -236.6317788436040246 ) ) ;
#58821 = CARTESIAN_POINT ( 'NONE',  ( -70.51346805374795679, -283.7497013960384606, -203.9353496555264371 ) ) ;
#58822 = CARTESIAN_POINT ( 'NONE',  ( 189.4188515237862589, 293.9636489450775798, 9.103929867429222611 ) ) ;
#58823 = CARTESIAN_POINT ( 'NONE',  ( 170.2305261370685798, 215.0000000000000568, -24.90909090909089940 ) ) ;
#58824 = CARTESIAN_POINT ( 'NONE',  ( 36.45556163586699228, -291.3793049181351762, -256.9118003839631683 ) ) ;
#58825 = CARTESIAN_POINT ( 'NONE',  ( -43.25105288263891623, -278.7281494628791734, -343.9241519424434728 ) ) ;
#58826 = CARTESIAN_POINT ( 'NONE',  ( -102.5718806867889157, -285.2295562291566284, -310.5236908862099767 ) ) ;
#58828 = CARTESIAN_POINT ( 'NONE',  ( -65.09322017174044106, -285.6793118563542180, -202.7880304802292244 ) ) ;
#58827 = CARTESIAN_POINT ( 'NONE',  ( -16.15719934957107995, -272.4036582613009045, -197.7772889889810131 ) ) ;
#58829 = CARTESIAN_POINT ( 'NONE',  ( 30.71286712240053518, -276.6035724799260151, -242.2282736131600132 ) ) ;
#58830 = CARTESIAN_POINT ( 'NONE',  ( -21.60835272250183792, -277.6482301879192391, -341.8629542140679973 ) ) ;
#58831 = CARTESIAN_POINT ( 'NONE',  ( -103.9947421547751674, -286.0959762084872295, -304.8600033902848736 ) ) ;
#58832 = ORIENTED_EDGE ( 'NONE', *, *, #30098, .T. ) ;
#58833 = LINE ( 'NONE', #81057, #87569 ) ;
#58834 = CARTESIAN_POINT ( 'NONE',  ( -114.2339486883503525, -296.3232390150516267, -275.3372576180619831 ) ) ;
#58835 = CARTESIAN_POINT ( 'NONE',  ( 14.25876389451109638, -288.7609432617553580, -216.3524702753543636 ) ) ;
#58836 = CARTESIAN_POINT ( 'NONE',  ( 156.4947056272797852, 20.00000000000000000, 15.00000000000000000 ) ) ;
#58837 = CARTESIAN_POINT ( 'NONE',  ( -111.2869819898779866, -275.4805209788415823, -234.7871824221999191 ) ) ;
#58838 = CARTESIAN_POINT ( 'NONE',  ( -105.8930810127271656, -277.9178965313490721, -235.8597397996663290 ) ) ;
#58839 = EDGE_CURVE ( 'NONE', #64509, #62133, #36556, .T. ) ;
#58840 = CARTESIAN_POINT ( 'NONE',  ( -90.21600432072389708, -289.7196670843477477, -215.4176193140183670 ) ) ;
#58841 = CARTESIAN_POINT ( 'NONE',  ( -27.76544216599693726, -287.6960984288273835, -197.2926361664710555 ) ) ;
#58842 = PRODUCT_DEFINITION_SHAPE ( 'NONE', 'NONE',  #93724 ) ;
#58843 = CARTESIAN_POINT ( 'NONE',  ( -97.23878091489238784, -280.9124018662243429, -226.8833796760500832 ) ) ;
#58844 = CARTESIAN_POINT ( 'NONE',  ( 14.21959363584990932, -289.7701931812119938, -326.8246708749955474 ) ) ;
#58845 = CARTESIAN_POINT ( 'NONE',  ( -112.2268251196354498, -286.6165758677043414, -265.3564490736544599 ) ) ;
#58846 = CARTESIAN_POINT ( 'NONE',  ( -67.70665367776241794, -277.6064314581030317, -341.1210614565739547 ) ) ;
#58847 = CARTESIAN_POINT ( 'NONE',  ( -111.7048106414051176, -270.6597741438939124, -261.9851869764115122 ) ) ;
#58848 = CARTESIAN_POINT ( 'NONE',  ( -114.2107287594964191, -278.4416154957397112, -265.8719708753156965 ) ) ;
#58849 = CARTESIAN_POINT ( 'NONE',  ( -104.3297122676974737, -274.8380146674984985, -238.3693736255214048 ) ) ;
#58850 = DIRECTION ( 'NONE',  ( -0.000000000000000000, 1.000000000000000000, -0.000000000000000000 ) ) ;
#58851 = CARTESIAN_POINT ( 'NONE',  ( -114.2704648735229114, -293.0519495502703080, -270.3937649182068981 ) ) ;
#58852 = CARTESIAN_POINT ( 'NONE',  ( -87.35236720989755099, -271.6062313604928136, -213.0818519771601132 ) ) ;
#58853 = FACE_OUTER_BOUND ( 'NONE', #81698, .T. ) ;
#58854 = CARTESIAN_POINT ( 'NONE',  ( -107.2842172096729172, -278.3391845951010168, -249.2416306304934892 ) ) ;
#58855 = CARTESIAN_POINT ( 'NONE',  ( -9.342588710788406914, -277.8992396139075822, -341.6637019363044487 ) ) ;
#58856 = CARTESIAN_POINT ( 'NONE',  ( -33.08381711170639505, -282.0585357233502464, -347.0207434526104180 ) ) ;
#58857 = CARTESIAN_POINT ( 'NONE',  ( 1.867139148768091284, -290.2798351753844486, -333.1356425550720246 ) ) ;
#58858 = CARTESIAN_POINT ( 'NONE',  ( -82.57529162147292823, -298.9671753574708077, -208.8411628457500058 ) ) ;
#58859 = CARTESIAN_POINT ( 'NONE',  ( -36.56115842718850928, -299.2667895415283397, -193.7580317958743024 ) ) ;
#58860 = CARTESIAN_POINT ( 'NONE',  ( 25.99212602163962060, -296.0905427348685066, -310.3189504394732694 ) ) ;
#58861 = CARTESIAN_POINT ( 'NONE',  ( 35.42707195648210217, -279.7773365963826677, -287.8721973614415219 ) ) ;
#58862 = CARTESIAN_POINT ( 'NONE',  ( -38.07375235313784856, -272.0630438585761226, -195.7199034539361264 ) ) ;
#58863 = CARTESIAN_POINT ( 'NONE',  ( 19.67446189663232659, -288.4595402276223695, -219.7303333684118343 ) ) ;
#58864 = CARTESIAN_POINT ( 'NONE',  ( 6.016423568887450557, -287.3689832375177389, -329.5369704759186220 ) ) ;
#58865 = CARTESIAN_POINT ( 'NONE',  ( 181.6150490960993409, 253.0111652753101907, -166.4923282781097384 ) ) ;
#58866 = ORIENTED_EDGE ( 'NONE', *, *, #84969, .F. ) ;
#58867 = CARTESIAN_POINT ( 'NONE',  ( 26.93920550320910579, -286.6741355203776607, -311.7693127202081200 ) ) ;
#58868 = CARTESIAN_POINT ( 'NONE',  ( -58.69936711498971249, -289.0026843312401184, -340.2418521902753810 ) ) ;
#58869 = ORIENTED_EDGE ( 'NONE', *, *, #49629, .F. ) ;
#58870 = CARTESIAN_POINT ( 'NONE',  ( -40.81628656781045805, -287.0892088255094450, -193.6969965600665375 ) ) ;
#58871 = CARTESIAN_POINT ( 'NONE',  ( -41.85365194326441696, -277.4438183483711668, -343.2553328600326381 ) ) ;
#58872 = CARTESIAN_POINT ( 'NONE',  ( 38.05083012601117076, -292.6498234575138895, -284.4840148903589920 ) ) ;
#58873 = CARTESIAN_POINT ( 'NONE',  ( 0.8249828439521571521, -283.2083820463604411, -337.1342299560292304 ) ) ;
#58874 = CARTESIAN_POINT ( 'NONE',  ( -6.528251926897602253, -281.9695935441709480, -200.5383867449178865 ) ) ;
#58875 = CARTESIAN_POINT ( 'NONE',  ( -69.17383618124584643, -283.7928009957932431, -340.4644669373690817 ) ) ;
#58877 = CARTESIAN_POINT ( 'NONE',  ( -38.35841236828841261, -280.3723462835667419, -197.3346479459443401 ) ) ;
#58876 = AXIS2_PLACEMENT_3D ( 'NONE', #17129, #87221, #45053 ) ;
#58878 = CARTESIAN_POINT ( 'NONE',  ( -85.28047601435909542, -276.9094976428776249, -210.1954327657594206 ) ) ;
#58879 = CARTESIAN_POINT ( 'NONE',  ( -77.88764424958249322, -208.6185847378275753, -357.2361643103192250 ) ) ;
#58880 = CARTESIAN_POINT ( 'NONE',  ( -95.00277939147495943, -279.8924247011059379, -318.0805402447278425 ) ) ;
#58881 = CARTESIAN_POINT ( 'NONE',  ( -96.26398026058502921, -239.2304635698770596, -341.1080143852184392 ) ) ;
#58882 = CARTESIAN_POINT ( 'NONE',  ( 201.0615148111058659, 293.2992890834858599, -53.99999999998998845 ) ) ;
#58883 = CARTESIAN_POINT ( 'NONE',  ( -51.58290462532085030, -273.0626169235216025, -198.5471792455737727 ) ) ;
#58884 = CARTESIAN_POINT ( 'NONE',  ( 26.44539895100070481, -292.4914513847094781, -227.2472432484072158 ) ) ;
#58885 = CARTESIAN_POINT ( 'NONE',  ( 65.71733346673669018, 45.99507470247991847, -315.6009874211030137 ) ) ;
#58887 = CARTESIAN_POINT ( 'NONE',  ( -7.918068316848774657, -287.0600984320034286, -338.0965385527741773 ) ) ;
#58886 = CARTESIAN_POINT ( 'NONE',  ( -37.58741160275177151, -296.6238665303497442, -193.9507396201146889 ) ) ;
#58888 = CARTESIAN_POINT ( 'NONE',  ( -76.28622154589834281, -297.4387637551195667, -333.6206400863862314 ) ) ;
#58889 = CARTESIAN_POINT ( 'NONE',  ( 33.13817507458800549, -288.5930380422211670, -249.4881567817710675 ) ) ;
#58890 = VERTEX_POINT ( 'NONE', #66386 ) ;
#58891 = CARTESIAN_POINT ( 'NONE',  ( -79.33818940139086351, -296.5455590026169261, -334.6193089097985194 ) ) ;
#58892 = CARTESIAN_POINT ( 'NONE',  ( -27.83474727839874774, -286.6684892426094962, -197.9207543095453445 ) ) ;
#58893 = CARTESIAN_POINT ( 'NONE',  ( 7.714195481699801960, -297.3993742180124400, -193.7671669734811530 ) ) ;
#58894 = CARTESIAN_POINT ( 'NONE',  ( -40.63575174420508773, -292.8145727743919906, -193.5800792851728147 ) ) ;
#58895 = CARTESIAN_POINT ( 'NONE',  ( 32.17710917916402735, -294.4686750548817145, -303.4498905156735873 ) ) ;
#58896 = CARTESIAN_POINT ( 'NONE',  ( -72.62881040321610726, -291.7381120840700532, -206.3995418752397768 ) ) ;
#58897 = ORIENTED_EDGE ( 'NONE', *, *, #67975, .T. ) ;
#58898 = CARTESIAN_POINT ( 'NONE',  ( -109.6660728353854211, -274.7541755011000078, -248.3074431420216115 ) ) ;
#58899 = CARTESIAN_POINT ( 'NONE',  ( 38.33773321966071990, -274.1969360720172517, -258.4176196307475379 ) ) ;
#58900 = EDGE_LOOP ( 'NONE', ( #38425, #36578, #29412, #78084 ) ) ;
#58901 = CARTESIAN_POINT ( 'NONE',  ( -59.65315930053900217, -276.8412712734797765, -343.9934864945411732 ) ) ;
#58902 = CARTESIAN_POINT ( 'NONE',  ( -108.7084954828143282, -271.1998180051596137, -251.3711846281036628 ) ) ;
#58903 = CARTESIAN_POINT ( 'NONE',  ( -64.81189032102298597, -275.5541994271221142, -339.3813183339466946 ) ) ;
#58904 = CARTESIAN_POINT ( 'NONE',  ( -46.22983261089778750, -275.0164206954806332, -197.5928063750375827 ) ) ;
#58905 = CARTESIAN_POINT ( 'NONE',  ( -110.1209284606944152, -273.6007124993415687, -262.2007030896518245 ) ) ;
#58906 = CARTESIAN_POINT ( 'NONE',  ( -107.1554795946085221, -274.7010474325054474, -240.2277889138057390 ) ) ;
#58907 = CARTESIAN_POINT ( 'NONE',  ( -20.51837627309085477, -274.8573997149402999, -343.8679314951482979 ) ) ;
#58908 = CARTESIAN_POINT ( 'NONE',  ( -75.70449723772257755, -296.2299559285264081, -332.6470406701505453 ) ) ;
#58909 = CARTESIAN_POINT ( 'NONE',  ( 1.868557943611208305, -293.0914319994585071, -332.6944925141015119 ) ) ;
#58910 = CARTESIAN_POINT ( 'NONE',  ( 197.4027394742815602, 40.84896208771628068, 12.00000000000000000 ) ) ;
#58911 = CARTESIAN_POINT ( 'NONE',  ( -77.77722091240910629, -278.0717534652443419, -335.8790847320632906 ) ) ;
#58912 = CARTESIAN_POINT ( 'NONE',  ( -14.06745114323619994, -274.5293442224414662, -201.1707332554465495 ) ) ;
#58913 = CARTESIAN_POINT ( 'NONE',  ( -60.34558280998903257, -284.4449287181309387, -197.3393371099973024 ) ) ;
#58914 = CARTESIAN_POINT ( 'NONE',  ( -93.27002073957315531, -297.8540675986060933, -320.6003165645169020 ) ) ;
#58915 = CARTESIAN_POINT ( 'NONE',  ( 208.3202200382901026, 36.51146326664311914, 14.79041613504217167 ) ) ;
#58916 = CARTESIAN_POINT ( 'NONE',  ( -17.11745018910179894, -285.5170379074419316, -199.9975442642219150 ) ) ;
#58917 = CARTESIAN_POINT ( 'NONE',  ( -108.5877533675832609, -277.0539537357707331, -250.2649094742505724 ) ) ;
#58918 = CARTESIAN_POINT ( 'NONE',  ( -110.4918092254458202, -277.0159210547054158, -278.8398254466879962 ) ) ;
#58919 = CARTESIAN_POINT ( 'NONE',  ( -111.0342782519586535, -286.7322029505577916, -256.3507368174655880 ) ) ;
#58920 = CARTESIAN_POINT ( 'NONE',  ( -16.54275820508942729, -275.5319100150848044, -199.9196723137866343 ) ) ;
#58921 = FACE_OUTER_BOUND ( 'NONE', #9488, .T. ) ;
#58922 = CARTESIAN_POINT ( 'NONE',  ( 22.87321032881527927, -274.5823657021647932, -317.0792212899704623 ) ) ;
#58923 = CARTESIAN_POINT ( 'NONE',  ( -97.96472585476233519, -281.1571022409814304, -225.8997953493799287 ) ) ;
#58924 = LINE ( 'NONE', #51794, #31701 ) ;
#58925 = CARTESIAN_POINT ( 'NONE',  ( 30.12485052753528691, -289.0261334428945474, -236.3379091713467801 ) ) ;
#58926 = CARTESIAN_POINT ( 'NONE',  ( 184.7149167944524493, -12.49482340714361506, 13.00000000000000178 ) ) ;
#58927 = CARTESIAN_POINT ( 'NONE',  ( -0.2253787972388012761, -290.5452444218242931, -205.1311799287882423 ) ) ;
#58928 = CARTESIAN_POINT ( 'NONE',  ( 76.08708295871279859, -293.9068999365417199, -465.6442049081569508 ) ) ;
#58929 = CARTESIAN_POINT ( 'NONE',  ( -99.69004999088407715, -271.7704218601475645, -231.4519063876864209 ) ) ;
#58930 = CARTESIAN_POINT ( 'NONE',  ( -52.60091212836192653, -289.9943232883415476, -197.6583465907052641 ) ) ;
#58931 = CARTESIAN_POINT ( 'NONE',  ( -87.71122462277782006, -229.8683413793775117, -344.1918058839762011 ) ) ;
#58932 = CARTESIAN_POINT ( 'NONE',  ( -41.96691551842204859, -295.9936855049469386, -195.5038669475833615 ) ) ;
#58933 = CARTESIAN_POINT ( 'NONE',  ( -5.929753362886146739, -287.1265573385318248, -339.9024535689309801 ) ) ;
#58934 = CARTESIAN_POINT ( 'NONE',  ( -54.71092135828460812, -284.0717335456884598, -196.3862292355044303 ) ) ;
#58935 = CARTESIAN_POINT ( 'NONE',  ( -96.38372556260050317, -285.3662044427798605, -314.2862150345133045 ) ) ;
#58936 = CARTESIAN_POINT ( 'NONE',  ( 14.04536185640826140, -283.1112763957603988, -322.5090513385317763 ) ) ;
#58937 = ADVANCED_FACE ( 'NONE', ( #44584 ), #81039, .F. ) ;
#58938 = CARTESIAN_POINT ( 'NONE',  ( -77.24360547928358756, -291.5637579885327000, -334.3457171614279559 ) ) ;
#58939 = AXIS2_PLACEMENT_3D ( 'NONE', #78177, #13315, #27993 ) ;
#58940 = CARTESIAN_POINT ( 'NONE',  ( -93.15975833594943367, -273.6102592397122635, -217.3316112663529793 ) ) ;
#58941 = ORIENTED_EDGE ( 'NONE', *, *, #19812, .T. ) ;
#58942 = CARTESIAN_POINT ( 'NONE',  ( 22.13848541245901558, -286.2669767911008307, -316.9804598304331762 ) ) ;
#58943 = CARTESIAN_POINT ( 'NONE',  ( 22.75835106102748284, -274.9071595080717429, -222.2051508334540415 ) ) ;
#58945 = CARTESIAN_POINT ( 'NONE',  ( 22.66338385601455485, -296.1407979237416725, -314.7597294620327943 ) ) ;
#58944 = AXIS2_PLACEMENT_3D ( 'NONE', #74047, #9166, #38044 ) ;
#58946 = CARTESIAN_POINT ( 'NONE',  ( -48.18343439339132317, -264.7419918502895371, -441.7985027590103186 ) ) ;
#58947 = CARTESIAN_POINT ( 'NONE',  ( -110.4683760289727132, -299.2662352645559167, -253.7030783399848985 ) ) ;
#58948 = CARTESIAN_POINT ( 'NONE',  ( -16.00521877666289683, -281.4551766739191407, -340.6889079416566233 ) ) ;
#58949 = CARTESIAN_POINT ( 'NONE',  ( -111.9498558912070649, -276.4295217776416962, -279.9204617637812476 ) ) ;
#58950 = CARTESIAN_POINT ( 'NONE',  ( -41.13872418729586400, -272.4851975925565739, -194.0971875971027885 ) ) ;
#58951 = CARTESIAN_POINT ( 'NONE',  ( 32.99366675342397315, -275.1642690305820906, -290.3274708819642456 ) ) ;
#58952 = CARTESIAN_POINT ( 'NONE',  ( 11.37477944881166003, -294.2617961111847080, -214.9991687206116637 ) ) ;
#58953 = CARTESIAN_POINT ( 'NONE',  ( 23.53017672154262740, -293.9297270521788619, -229.6422887141216336 ) ) ;
#58954 = CARTESIAN_POINT ( 'NONE',  ( -110.4252592086296829, -286.4655049725199092, -258.5859294606688650 ) ) ;
#58955 = CARTESIAN_POINT ( 'NONE',  ( 36.89193095903815589, -295.2063259400989637, -288.5259821930274029 ) ) ;
#58956 = CARTESIAN_POINT ( 'NONE',  ( 37.59099979720906504, -295.0616616678769333, -285.8009611269818606 ) ) ;
#58957 = CARTESIAN_POINT ( 'NONE',  ( -105.8050899075722242, -296.7250055449352431, -244.8822574279839728 ) ) ;
#58958 = CARTESIAN_POINT ( 'NONE',  ( -93.90371999971841888, -291.8680659380046905, -319.6904826566554334 ) ) ;
#58959 = CARTESIAN_POINT ( 'NONE',  ( -71.73683551964978733, -283.6608152228989752, -339.2521527108037844 ) ) ;
#58960 = CARTESIAN_POINT ( 'NONE',  ( -67.57832461212092312, -295.7385586132759840, -201.0590153170460894 ) ) ;
#58961 = CARTESIAN_POINT ( 'NONE',  ( -113.4871014224534207, -284.5329444566350503, -258.5694012711036862 ) ) ;
#58962 = CARTESIAN_POINT ( 'NONE',  ( -36.42115123335905480, -279.0204850422260279, -345.0129935741259715 ) ) ;
#58963 = EDGE_CURVE ( 'NONE', #42078, #14296, #48645, .T. ) ;
#58964 = CARTESIAN_POINT ( 'NONE',  ( -95.26098864176314862, -283.9790968634272303, -225.2576083044342568 ) ) ;
#58965 = CARTESIAN_POINT ( 'NONE',  ( 27.17011911388962631, -286.0636770660341313, -308.6132528892103437 ) ) ;
#58966 = CARTESIAN_POINT ( 'NONE',  ( -20.01529863951607879, -278.4119629748929583, -196.5501794976063081 ) ) ;
#58967 = CARTESIAN_POINT ( 'NONE',  ( 60.10016229265469434, 49.69813606028536412, -316.8989054076328671 ) ) ;
#58968 = CARTESIAN_POINT ( 'NONE',  ( -109.6722641815814256, -284.1956824531847587, -260.0519984572719636 ) ) ;
#58969 = CARTESIAN_POINT ( 'NONE',  ( 38.03760809406004029, -282.9295741673332714, -284.0710867462686338 ) ) ;
#58970 = CARTESIAN_POINT ( 'NONE',  ( -51.65322569755518600, -288.2896914087506843, -345.7799514937378262 ) ) ;
#58971 = CARTESIAN_POINT ( 'NONE',  ( 3.094430122261770499, -278.1192837331672081, -335.0093045963768077 ) ) ;
#58972 = CARTESIAN_POINT ( 'NONE',  ( -28.64038288085472672, -278.2593049187998417, -346.4247803407751007 ) ) ;
#58973 = CARTESIAN_POINT ( 'NONE',  ( -106.4440393492983361, -278.7000825332641512, -246.6715273318023662 ) ) ;
#58974 = CARTESIAN_POINT ( 'NONE',  ( 25.71465333278364085, -294.1367638121599271, -314.5757150828541739 ) ) ;
#58975 = CARTESIAN_POINT ( 'NONE',  ( 37.10069150266329530, -285.4536822671885830, -262.7218278711971493 ) ) ;
#58976 = CARTESIAN_POINT ( 'NONE',  ( -33.59925002363613089, -293.6986446575913305, -194.2530731798775321 ) ) ;
#58977 = CARTESIAN_POINT ( 'NONE',  ( -3.011119155476607467, -293.5075484080761612, -335.1348571395924409 ) ) ;
#58978 = EDGE_CURVE ( 'NONE', #19412, #90166, #87966, .T. ) ;
#58979 = CARTESIAN_POINT ( 'NONE',  ( -4.330896837207037997, -294.2713237353578393, -335.5086316512798703 ) ) ;
#58980 = CARTESIAN_POINT ( 'NONE',  ( -110.4828615250422672, -291.3388655520912494, -293.5966631804272993 ) ) ;
#58981 = CARTESIAN_POINT ( 'NONE',  ( -4.308920300665096015, -281.1509040530035008, -205.1342636821833878 ) ) ;
#58982 = CARTESIAN_POINT ( 'NONE',  ( -112.8346684315676214, -271.7890231973934760, -256.1623847164062227 ) ) ;
#58983 = CARTESIAN_POINT ( 'NONE',  ( 38.99043517742371989, -288.3255484588295303, -280.1020315264777309 ) ) ;
#58984 = CARTESIAN_POINT ( 'NONE',  ( 10.69093041217995577, -280.5364371622299018, -329.0222660641302923 ) ) ;
#58985 = CARTESIAN_POINT ( 'NONE',  ( 16.67414502254573350, -288.6426288854995619, -325.2807812701290686 ) ) ;
#58986 = CARTESIAN_POINT ( 'NONE',  ( -19.81488969910387610, -286.6170453603684791, -199.4746002033248260 ) ) ;
#58987 = CARTESIAN_POINT ( 'NONE',  ( 189.2871950347832524, 271.4890288426949496, -139.5295763808702532 ) ) ;
#58988 = CARTESIAN_POINT ( 'NONE',  ( -90.91305330213944558, -228.9931328718925272, -345.8290054490478269 ) ) ;
#58989 = CARTESIAN_POINT ( 'NONE',  ( -93.95058081101505820, -238.6390622938258161, -338.4896325803341597 ) ) ;
#58990 = CARTESIAN_POINT ( 'NONE',  ( -110.3302377797428164, -277.6740220409643598, -276.0813506845647112 ) ) ;
#58991 = CARTESIAN_POINT ( 'NONE',  ( -110.4660108335609578, -277.5408090408507746, -265.1590744632180758 ) ) ;
#58992 = CARTESIAN_POINT ( 'NONE',  ( -60.86062103588250949, -273.4219396883899549, -197.0074507838691602 ) ) ;
#58993 = CARTESIAN_POINT ( 'NONE',  ( 203.9605228849236482, 292.2036489450777026, -53.99999999999079137 ) ) ;
#58994 = CARTESIAN_POINT ( 'NONE',  ( -112.1370031990514207, -277.3246467595996023, -254.6689879938084289 ) ) ;
#58995 = APPLICATION_CONTEXT ( 'automotive_design' ) ;
#58996 = CARTESIAN_POINT ( 'NONE',  ( -67.79916128539190368, -297.2065701210532325, -339.9766124903949844 ) ) ;
#58997 = CARTESIAN_POINT ( 'NONE',  ( -55.03332002274466106, -292.3107864874427264, -199.4739186658815981 ) ) ;
#58998 = CARTESIAN_POINT ( 'NONE',  ( -44.03422780989043162, -274.9108829038041222, -193.8355570673414547 ) ) ;
#58999 = CARTESIAN_POINT ( 'NONE',  ( -50.85848890386299104, -287.9131464509084708, -342.6526103191416723 ) ) ;
#59000 = CARTESIAN_POINT ( 'NONE',  ( -87.97549789000325404, -274.0173976530444975, -212.4151804432509891 ) ) ;
#59001 = CARTESIAN_POINT ( 'NONE',  ( -98.44873424958512942, -297.2733939395707807, -230.3330594901038353 ) ) ;
#59002 = ORIENTED_EDGE ( 'NONE', *, *, #43223, .T. ) ;
#59003 = DIRECTION ( 'NONE',  ( 0.3262578496237564796, 0.000000000000000000, 0.9452808130703185263 ) ) ;
#59004 = CARTESIAN_POINT ( 'NONE',  ( -58.91484553012831782, -281.6953376119867016, -197.9462466288546807 ) ) ;
#59005 = VECTOR ( 'NONE', #19816, 1000.000000000000114 ) ;
#59006 = CARTESIAN_POINT ( 'NONE',  ( -89.70395773035794207, -280.3720065990585226, -218.9820465119535982 ) ) ;
#59007 = CARTESIAN_POINT ( 'NONE',  ( -101.0539782450407245, -280.8644320843680475, -228.8566927599659664 ) ) ;
#59008 = CIRCLE ( 'NONE', #27241, 6.649382010133625620 ) ;
#59009 = CARTESIAN_POINT ( 'NONE',  ( -66.06570792790306257, -272.1491368199127692, -202.4962586705537149 ) ) ;
#59010 = DIRECTION ( 'NONE',  ( 0.000000000000000000, 0.000000000000000000, 1.000000000000000000 ) ) ;
#59011 = CARTESIAN_POINT ( 'NONE',  ( 140.6539576904058606, 249.5000000000000568, 10.50000000000000000 ) ) ;
#59012 = CARTESIAN_POINT ( 'NONE',  ( 17.06139564414758780, -281.0224355033984693, -221.6856295421403900 ) ) ;
#59013 = CARTESIAN_POINT ( 'NONE',  ( 3.424515937575832059, -277.3221164316823319, -335.5565000873030499 ) ) ;
#59014 = CARTESIAN_POINT ( 'NONE',  ( 37.55540866634535035, -277.4904424956212665, -265.5422211869925491 ) ) ;
#59015 = CARTESIAN_POINT ( 'NONE',  ( -64.89963812391857800, -275.9797482302329286, -341.6852499300943009 ) ) ;
#59016 = ORIENTED_EDGE ( 'NONE', *, *, #19908, .T. ) ;
#59017 = DIRECTION ( 'NONE',  ( -0.8457827187922968282, -0.5335274993777835428, -5.868796551457945175E-15 ) ) ;
#59018 = CARTESIAN_POINT ( 'NONE',  ( 1.273400189806133120, -284.5189617964918511, -335.0703200330463574 ) ) ;
#59019 = CARTESIAN_POINT ( 'NONE',  ( -66.61932730203763242, -290.8557044940275773, -203.3132076913531989 ) ) ;
#59020 = CARTESIAN_POINT ( 'NONE',  ( -15.43454434066708991, -285.6769298719635231, -196.5942692700515977 ) ) ;
#59021 = CARTESIAN_POINT ( 'NONE',  ( -111.4045987207254598, -282.7850627247556190, -270.8945385973955240 ) ) ;
#59023 = CARTESIAN_POINT ( 'NONE',  ( 34.42391937420377701, -285.3757675322946739, -250.5871437428761510 ) ) ;
#59022 = CARTESIAN_POINT ( 'NONE',  ( -100.9192527532075303, -282.6223695539415530, -307.4187719590406687 ) ) ;
#59024 = CARTESIAN_POINT ( 'NONE',  ( -54.60096772788035935, -281.0306102546521743, -198.9696671825705607 ) ) ;
#59025 = CARTESIAN_POINT ( 'NONE',  ( -94.48684376863917578, -271.2244966748070283, -221.7673554892992343 ) ) ;
#59026 = CARTESIAN_POINT ( 'NONE',  ( -87.80713208062361730, -282.1430848468509680, -327.5252007734106883 ) ) ;
#59027 = CARTESIAN_POINT ( 'NONE',  ( 26.41942082615214815, -296.0836441883024008, -309.9494991486461117 ) ) ;
#59028 = CARTESIAN_POINT ( 'NONE',  ( -35.22598679939277844, -288.0787840986485548, -195.2113975730414666 ) ) ;
#59029 = CARTESIAN_POINT ( 'NONE',  ( 153.1588060538193190, 19.71797249535330465, 10.20021433907233899 ) ) ;
#59030 = CARTESIAN_POINT ( 'NONE',  ( -50.34307550991074010, -293.8075671654117400, -195.9280713320153779 ) ) ;
#59031 = CARTESIAN_POINT ( 'NONE',  ( 24.08975459295512067, -274.1370893516504452, -313.4755456552930468 ) ) ;
#59032 = CARTESIAN_POINT ( 'NONE',  ( -82.76543319232921192, -288.8529912497588725, -332.3356554518549046 ) ) ;
#59033 = CARTESIAN_POINT ( 'NONE',  ( 36.33472413660140887, -291.8857324229359165, -265.2813576249653806 ) ) ;
#59034 = CARTESIAN_POINT ( 'NONE',  ( -97.29764994530189881, -276.6472350943205925, -312.8862461990938755 ) ) ;
#59035 = CARTESIAN_POINT ( 'NONE',  ( -104.8318481053914439, -295.1032419795643591, -239.3191104695110027 ) ) ;
#59036 = CARTESIAN_POINT ( 'NONE',  ( -84.99212525919708128, -291.0406806839543492, -326.3807604979632515 ) ) ;
#59037 = SURFACE_STYLE_FILL_AREA ( #10687 ) ;
#59038 = CYLINDRICAL_SURFACE ( 'NONE', #11067, 5.999999999999998224 ) ;
#59039 = CARTESIAN_POINT ( 'NONE',  ( -79.11374627568183371, -294.0845816161651669, -334.2188028154411086 ) ) ;
#59040 = CARTESIAN_POINT ( 'NONE',  ( 24.92413337914894811, -289.6940734194641323, -309.9768521332014188 ) ) ;
#59041 = CARTESIAN_POINT ( 'NONE',  ( -100.8248704200626662, -289.3494045767073999, -228.5071736212836129 ) ) ;
#59042 = CARTESIAN_POINT ( 'NONE',  ( -58.84410339083934360, -290.7609546723720086, -340.7920499248559167 ) ) ;
#59043 = CARTESIAN_POINT ( 'NONE',  ( 123.4306832106270946, -134.2391364535880882, 0.000000000000000000 ) ) ;
#59044 = CARTESIAN_POINT ( 'NONE',  ( -97.47581569208040264, -290.7754018532565965, -312.0543351086399184 ) ) ;
#59045 = EDGE_CURVE ( 'NONE', #71577, #6380, #44113, .T. ) ;
#59046 = DIRECTION ( 'NONE',  ( 0.000000000000000000, 0.000000000000000000, 1.000000000000000000 ) ) ;
#59047 = CARTESIAN_POINT ( 'NONE',  ( -48.79439720628084132, -290.3998488215689804, -346.1567423622017259 ) ) ;
#59048 = CARTESIAN_POINT ( 'NONE',  ( -6.871820801296058434, -278.4701452238938373, -201.4269532034054748 ) ) ;
#59049 = CARTESIAN_POINT ( 'NONE',  ( -48.12002027596228260, -280.2520172715671833, -194.0867388308380157 ) ) ;
#59050 = CARTESIAN_POINT ( 'NONE',  ( -64.73083512763891179, -279.3709636644597936, -198.3634043056420069 ) ) ;
#59051 = CARTESIAN_POINT ( 'NONE',  ( -70.85383957383592701, -283.6099794496257118, -203.2503172555763626 ) ) ;
#59052 = CARTESIAN_POINT ( 'NONE',  ( 196.2236821186898794, 42.37849173453419382, 11.63735566334416660 ) ) ;
#59053 = CARTESIAN_POINT ( 'NONE',  ( -49.31824139127019180, -278.0374561077733802, -197.0983857279997267 ) ) ;
#59054 = CARTESIAN_POINT ( 'NONE',  ( -1.357977749472828455, -280.5748210327720926, -336.1797120751910484 ) ) ;
#59055 = CARTESIAN_POINT ( 'NONE',  ( 207.9698821865255525, 1.063508326896293932, 7.500000000000007105 ) ) ;
#59056 = CARTESIAN_POINT ( 'NONE',  ( -101.5244020387511341, -276.4845445126429127, -311.7284878036716691 ) ) ;
#59057 =( BOUNDED_SURFACE ( )  B_SPLINE_SURFACE ( 3, 2, ( 
 ( #28352, #34516, #27896 ),
 ( #84680, #55824, #78999 ),
 ( #71441, #63423, #86084 ),
 ( #13679, #12751, #50104 ),
 ( #14153, #20314, #93654 ),
 ( #56785, #41592, #92252 ),
 ( #43018, #70514, #49184 ),
 ( #64830, #43473, #13221 ),
 ( #42057, #72370, #35456 ),
 ( #28814, #85627, #57698 ),
 ( #86541, #21711, #7487 ),
 ( #45778, #58176, #9813 ),
 ( #80853, #16000, #72820 ),
 ( #390, #7945, #51961 ),
 ( #37745, #29279, #45306 ),
 ( #87930, #36840, #87018 ) ),
 .UNSPECIFIED., .F., .F., .F. ) 
 B_SPLINE_SURFACE_WITH_KNOTS ( ( 4, 2, 2, 2, 2, 2, 2, 4 ),
 ( 3, 3 ),
 ( 0.000000000000000000, 0.0006169105258908347050, 0.001233821051781669410, 0.001850731577672504007, 0.002467642103563338820, 0.003084552629454173633, 0.003701463155345008013, 0.004935284207126677640 ),
 ( 0.000000000000000000, 1.000000000000000000 ),
 .UNSPECIFIED. ) 
 GEOMETRIC_REPRESENTATION_ITEM ( )  RATIONAL_B_SPLINE_SURFACE ( (
 ( 1.000000000000000000, 0.8966167345234253849, 1.000000000000000000),
 ( 1.000000000000000000, 0.9004139148593394149, 1.000000000000000000),
 ( 1.000000000000000000, 0.9032061010809223633, 1.000000000000000000),
 ( 1.000000000000000000, 0.9067734849426619670, 1.000000000000000000),
 ( 1.000000000000000000, 0.9075308745978637459, 1.000000000000000000),
 ( 1.000000000000000000, 0.9069696504598226960, 1.000000000000000000),
 ( 1.000000000000000000, 0.9056888044671186355, 1.000000000000000000),
 ( 1.000000000000000000, 0.9012558131653337634, 1.000000000000000000),
 ( 1.000000000000000000, 0.8981641526238748341, 1.000000000000000000),
 ( 1.000000000000000000, 0.8905754532997738337, 1.000000000000000000),
 ( 1.000000000000000000, 0.8860218362694791683, 1.000000000000000000),
 ( 1.000000000000000000, 0.8759703649558354677, 1.000000000000000000),
 ( 1.000000000000000000, 0.8704567387601739314, 1.000000000000000000),
 ( 1.000000000000000000, 0.8526573370801874274, 1.000000000000000000),
 ( 1.000000000000000000, 0.8394012181881534973, 1.000000000000000000),
 ( 1.000000000000000000, 0.8255171224912161154, 1.000000000000000000) ) ) 
 REPRESENTATION_ITEM ( '' )  SURFACE ( )  );
#59058 = CARTESIAN_POINT ( 'NONE',  ( -52.79923344721267853, -299.3707396034314456, -198.2547823274953771 ) ) ;
#59059 = CARTESIAN_POINT ( 'NONE',  ( -94.17934335839788673, -282.7700828251171856, -321.8682173719171260 ) ) ;
#59060 = CARTESIAN_POINT ( 'NONE',  ( -43.50590004731491689, -274.7752731851270482, -197.4089617291056129 ) ) ;
#59061 = CARTESIAN_POINT ( 'NONE',  ( -83.24075413761218556, -274.8628523080236050, -209.2057428890541075 ) ) ;
#59062 = CARTESIAN_POINT ( 'NONE',  ( 22.48071900126181433, -275.8036995446516357, -312.3211292519922040 ) ) ;
#59063 = CARTESIAN_POINT ( 'NONE',  ( -20.37153152378789400, -296.8344807776048810, -343.4695247431674261 ) ) ;
#59064 = CARTESIAN_POINT ( 'NONE',  ( -38.91804670270450117, -289.2380963281947857, -347.3449808111181483 ) ) ;
#59065 =( BOUNDED_CURVE ( )  B_SPLINE_CURVE ( 3, ( #51533, #37788, #16041, #1823 ),
 .UNSPECIFIED., .F., .F. ) 
 B_SPLINE_CURVE_WITH_KNOTS ( ( 4, 4 ),
 ( 0.5235987755983022574, 1.570796326794897224 ),
 .UNSPECIFIED. ) 
 CURVE ( )  GEOMETRIC_REPRESENTATION_ITEM ( )  RATIONAL_B_SPLINE_CURVE ( ( 1.000000000000000000, 0.9106836025229594345, 0.9106836025229594345, 1.000000000000000000 ) ) 
 REPRESENTATION_ITEM ( '' )  );
#59066 = CARTESIAN_POINT ( 'NONE',  ( -50.66131443997187489, -277.9631422608254070, -195.9843603897674029 ) ) ;
#59067 = CARTESIAN_POINT ( 'NONE',  ( -109.4730951778205394, -290.7279668149149074, -243.2636462022585420 ) ) ;
#59068 = ADVANCED_FACE ( 'NONE', ( #15723, #87204, #8145 ), #74394, .F. ) ;
#59069 = EDGE_CURVE ( 'NONE', #38347, #14152, #90998, .T. ) ;
#59071 = CARTESIAN_POINT ( 'NONE',  ( -108.8951816176935097, -289.4049964021939445, -286.0241950955173706 ) ) ;
#59070 = AXIS2_PLACEMENT_3D ( 'NONE', #54176, #83046, #32871 ) ;
#59072 = CARTESIAN_POINT ( 'NONE',  ( -9.236426670508436132, -290.4194269153589971, -200.8262759705705207 ) ) ;
#59073 = ORIENTED_EDGE ( 'NONE', *, *, #17361, .F. ) ;
#59074 = PLANE ( 'NONE',  #89247 ) ;
#59075 = CARTESIAN_POINT ( 'NONE',  ( -100.3602033031739609, -289.5514303536575085, -307.4290974135429906 ) ) ;
#59076 = CARTESIAN_POINT ( 'NONE',  ( 60.83289261295102079, -250.0118895884541530, 21.50000000000000000 ) ) ;
#59077 = CIRCLE ( 'NONE', #54519, 2.186979415864515275 ) ;
#59078 = CARTESIAN_POINT ( 'NONE',  ( 29.91959850135221899, -288.0115359480757888, -233.2543962794700292 ) ) ;
#59079 = CARTESIAN_POINT ( 'NONE',  ( 27.33386217378599881, -295.6233781216987495, -239.1787733560258573 ) ) ;
#59080 = CARTESIAN_POINT ( 'NONE',  ( -0.8286853145115329333, -293.6381952032917866, -337.9009148296640319 ) ) ;
#59081 = CARTESIAN_POINT ( 'NONE',  ( 21.24325495529707197, -283.5340859632416937, -319.5658058905803500 ) ) ;
#59082 = VECTOR ( 'NONE', #34287, 1000.000000000000000 ) ;
#59083 = CARTESIAN_POINT ( 'NONE',  ( -110.3092621230438510, -284.4141758594314524, -268.1851352172002976 ) ) ;
#59084 = CARTESIAN_POINT ( 'NONE',  ( 35.86788377100840108, -276.7755592877944650, -263.3572010220200355 ) ) ;
#59085 = CARTESIAN_POINT ( 'NONE',  ( 37.35376758639417005, -291.5778394467686780, -270.7940726316613222 ) ) ;
#59086 = CARTESIAN_POINT ( 'NONE',  ( -76.76464319899919531, -272.3062727201800044, -208.4501975885578702 ) ) ;
#59087 = ORIENTED_EDGE ( 'NONE', *, *, #34052, .F. ) ;
#59088 = CARTESIAN_POINT ( 'NONE',  ( -114.4693872376281121, -273.8646567567205921, -270.3778293100139081 ) ) ;
#59089 = CARTESIAN_POINT ( 'NONE',  ( -53.28901166602894790, -294.9178646318595725, -345.7245277394727054 ) ) ;
#59090 = CARTESIAN_POINT ( 'NONE',  ( -41.42591119986312975, -287.9205116072261603, -196.0204954558087138 ) ) ;
#59091 = CARTESIAN_POINT ( 'NONE',  ( -98.85277881934371180, -298.2436921384124275, -224.5365786145442257 ) ) ;
#59092 = EDGE_CURVE ( 'NONE', #19714, #15987, #63834, .T. ) ;
#59093 = CARTESIAN_POINT ( 'NONE',  ( 17.84770293480332626, -287.5211043880350417, -222.4234244837805647 ) ) ;
#59094 = CARTESIAN_POINT ( 'NONE',  ( -108.4430235737596178, -277.2422597555933521, -299.2993628611334884 ) ) ;
#59095 = CARTESIAN_POINT ( 'NONE',  ( -66.87760821092773256, -296.0805633125021927, -341.3748981024409090 ) ) ;
#59096 = CARTESIAN_POINT ( 'NONE',  ( 23.14161440105112177, -286.3092921343909438, -315.9908686596827465 ) ) ;
#59097 = CARTESIAN_POINT ( 'NONE',  ( 37.40039647763912001, -293.6549142209549927, -251.9393024743903311 ) ) ;
#59098 = CARTESIAN_POINT ( 'NONE',  ( -41.59831225575243963, -292.3304886612406222, -197.4142837545906843 ) ) ;
#59099 = FACE_OUTER_BOUND ( 'NONE', #70562, .T. ) ;
#59100 = DIRECTION ( 'NONE',  ( 1.000000000000000000, 0.000000000000000000, -0.000000000000000000 ) ) ;
#59101 = CARTESIAN_POINT ( 'NONE',  ( 202.9739431815425235, 291.9636489454802017, -68.24819713443925195 ) ) ;
#59102 = CARTESIAN_POINT ( 'NONE',  ( 28.09393383406584377, -288.5545145537709004, -231.0051378809324376 ) ) ;
#59103 = CARTESIAN_POINT ( 'NONE',  ( -72.08107566293803359, -280.9809262143061233, -342.4248175857292154 ) ) ;
#59104 = EDGE_LOOP ( 'NONE', ( #77891, #21960, #75814, #15519 ) ) ;
#59105 = CARTESIAN_POINT ( 'NONE',  ( -111.6303997534848520, -278.1503381933561059, -250.4482305831111546 ) ) ;
#59106 = CARTESIAN_POINT ( 'NONE',  ( 10.42774253480610547, -282.7130705988873274, -212.6905608907666760 ) ) ;
#59107 = CARTESIAN_POINT ( 'NONE',  ( 201.1965474191012504, 286.6890272589430424, -96.92993898827639043 ) ) ;
#59108 = CARTESIAN_POINT ( 'NONE',  ( -69.52797545116446543, -284.2115517108798599, -201.0457095323620251 ) ) ;
#59109 = CARTESIAN_POINT ( 'NONE',  ( 35.09683540725919215, -285.8538167795406935, -287.5067521566995765 ) ) ;
#59110 = CARTESIAN_POINT ( 'NONE',  ( -49.54403497918417543, -275.7587145875591546, -195.5324524860870099 ) ) ;
#59111 = CARTESIAN_POINT ( 'NONE',  ( -36.48879044673999061, -298.5554612201654550, -197.2995053034559021 ) ) ;
#59112 = VERTEX_POINT ( 'NONE', #29932 ) ;
#59113 = CARTESIAN_POINT ( 'NONE',  ( 17.43703797275952638, -292.9333689359762047, -319.3753243287773103 ) ) ;
#59114 = CARTESIAN_POINT ( 'NONE',  ( -106.2503485270460288, -278.7629663289929454, -304.6116875327993512 ) ) ;
#59115 = CARTESIAN_POINT ( 'NONE',  ( 30.27802776076735825, -275.9222054910284783, -298.0014827827318413 ) ) ;
#59116 = CARTESIAN_POINT ( 'NONE',  ( -102.4638420214725301, -274.1638313190111944, -229.8568077856197078 ) ) ;
#59117 = CARTESIAN_POINT ( 'NONE',  ( -73.96139778352669225, -276.4471866244645071, -337.7592209991657910 ) ) ;
#59118 = CARTESIAN_POINT ( 'NONE',  ( -110.5173715819909575, -266.5038384662269095, -306.9164069516367590 ) ) ;
#59119 = CARTESIAN_POINT ( 'NONE',  ( 36.28522939467180919, -273.3677241083664740, -256.0098019135094205 ) ) ;
#59120 = CARTESIAN_POINT ( 'NONE',  ( -97.79705253300559775, -297.3488111491417953, -317.0918002014356603 ) ) ;
#59121 = CARTESIAN_POINT ( 'NONE',  ( 156.9788746593517033, 250.1588552167596333, 16.89623126087882099 ) ) ;
#59122 = CARTESIAN_POINT ( 'NONE',  ( 180.7149167944524493, -12.49482340714361506, 10.00000000000000000 ) ) ;
#59123 = CARTESIAN_POINT ( 'NONE',  ( -98.37199123406922752, -286.1932347336254452, -229.7467160887507021 ) ) ;
#59124 = CARTESIAN_POINT ( 'NONE',  ( -66.17075887807945378, -285.1844665087870112, -340.6805870677355301 ) ) ;
#59125 = CARTESIAN_POINT ( 'NONE',  ( -35.92318276719742443, -285.4189953989413198, -197.2729487824906300 ) ) ;
#59126 = CARTESIAN_POINT ( 'NONE',  ( -102.8567936818223387, -277.4103837043670069, -236.2762466137838544 ) ) ;
#59127 = CARTESIAN_POINT ( 'NONE',  ( -92.56837818269444540, -285.7141611097057421, -319.9874909923241830 ) ) ;
#59128 = CARTESIAN_POINT ( 'NONE',  ( -38.34401603073168019, -278.5192435690294701, -196.6620806762900600 ) ) ;
#59129 = CARTESIAN_POINT ( 'NONE',  ( 11.96573502319869320, -277.4274542991929025, -324.6794638628950338 ) ) ;
#59130 = CARTESIAN_POINT ( 'NONE',  ( 219.8344101925596021, 35.72494958537217968, -7.000000000000000888 ) ) ;
#59131 = CARTESIAN_POINT ( 'NONE',  ( -19.26245373214130296, -274.7833328453204444, -199.5193174185405098 ) ) ;
#59132 = CARTESIAN_POINT ( 'NONE',  ( 28.17268597888741510, -282.8817997075269659, -310.6119905462495012 ) ) ;
#59133 = CARTESIAN_POINT ( 'NONE',  ( -34.47498158608785701, -283.5093668984592910, -347.2461544213545039 ) ) ;
#59134 = VERTEX_POINT ( 'NONE', #51680 ) ;
#59135 = ORIENTED_EDGE ( 'NONE', *, *, #92101, .F. ) ;
#59136 = CARTESIAN_POINT ( 'NONE',  ( 196.8803347170859865, 42.36571313990103249, 12.49999999999999289 ) ) ;
#59137 = CARTESIAN_POINT ( 'NONE',  ( 15.42172952163182842, -288.6488663652718287, -215.9890114335678675 ) ) ;
#59138 = CARTESIAN_POINT ( 'NONE',  ( -98.79839149250919661, -289.8469253770654177, -224.7719379034734004 ) ) ;
#59139 = EDGE_CURVE ( 'NONE', #55081, #26459, #67319, .T. ) ;
#59140 = CARTESIAN_POINT ( 'NONE',  ( -102.6719321324302285, -296.1966716442356642, -237.3156512049067715 ) ) ;
#59141 = CARTESIAN_POINT ( 'NONE',  ( -7.222471578065059461, -291.7855478872908179, -199.5926989929982653 ) ) ;
#59142 = CARTESIAN_POINT ( 'NONE',  ( -5.510310450117462011, -287.1054780762986525, -336.8251713193008072 ) ) ;
#59143 = CARTESIAN_POINT ( 'NONE',  ( -21.01613257656125455, -287.4132519910804717, -342.1166108700935524 ) ) ;
#59144 = CARTESIAN_POINT ( 'NONE',  ( -60.11632823701467032, -286.9553389800802279, -200.5868618510524186 ) ) ;
#59145 = CARTESIAN_POINT ( 'NONE',  ( -110.4464167217849848, -276.7671167876472964, -253.6069822085198382 ) ) ;
#59146 = CARTESIAN_POINT ( 'NONE',  ( 37.57823079558884416, -289.4951776762216582, -265.9110003796409387 ) ) ;
#59147 = CARTESIAN_POINT ( 'NONE',  ( -68.61826181696213212, -287.4620365835401117, -338.7258051652080439 ) ) ;
#59148 = CIRCLE ( 'NONE', #92367, 2.397123461337413719 ) ;
#59149 = CARTESIAN_POINT ( 'NONE',  ( -102.4530433121057627, -285.9476772324411513, -236.8361804557841026 ) ) ;
#59150 = CARTESIAN_POINT ( 'NONE',  ( -112.5355219157387552, -292.5770836622889419, -268.4278995277938975 ) ) ;
#59151 = CARTESIAN_POINT ( 'NONE',  ( 197.0217226327351909, 214.8115906558234371, -12.45424042348861704 ) ) ;
#59152 = CARTESIAN_POINT ( 'NONE',  ( 155.1244896729671439, 20.04296953158265993, -14.86678859756603543 ) ) ;
#59153 = CARTESIAN_POINT ( 'NONE',  ( -77.45902287679265896, -299.4385109443612691, -206.3305423765728221 ) ) ;
#59154 = CARTESIAN_POINT ( 'NONE',  ( 0.4921901685661741466, -279.7671358742132384, -207.6829960213547963 ) ) ;
#59155 = CARTESIAN_POINT ( 'NONE',  ( 25.80085034987899206, -280.0980954989550469, -310.9289899061022879 ) ) ;
#59156 = CARTESIAN_POINT ( 'NONE',  ( -5.873200673730681665, -293.8460328441070146, -340.4602789128251743 ) ) ;
#59157 = CARTESIAN_POINT ( 'NONE',  ( -36.45111023169724973, -296.4633527993654525, -196.5613598044025139 ) ) ;
#59158 = CARTESIAN_POINT ( 'NONE',  ( 14.72132402073479795, -274.3922792783134810, -323.6377286171231162 ) ) ;
#59159 = CARTESIAN_POINT ( 'NONE',  ( -0.4963008571692998361, -295.8669956767841995, -334.0089867835717428 ) ) ;
#59160 = DIRECTION ( 'NONE',  ( -0.000000000000000000, -1.000000000000000000, -0.000000000000000000 ) ) ;
#59161 = CARTESIAN_POINT ( 'NONE',  ( -106.8370676071185841, -295.1908193906509155, -239.5005421950999676 ) ) ;
#59162 = CARTESIAN_POINT ( 'NONE',  ( -7.734722263637749506, -296.0816355774206272, -337.7454367609204837 ) ) ;
#59163 = DIRECTION ( 'NONE',  ( -1.000000000000000000, 0.000000000000000000, -0.000000000000000000 ) ) ;
#59164 = CARTESIAN_POINT ( 'NONE',  ( -66.10723174152366255, -296.2413803868636251, -337.6303228113463888 ) ) ;
#59165 = DIRECTION ( 'NONE',  ( -1.000000000000000000, 0.000000000000000000, -0.000000000000000000 ) ) ;
#59167 = CARTESIAN_POINT ( 'NONE',  ( -110.0503104255924427, -296.6453045863960369, -263.2996556057767066 ) ) ;
#59166 = CARTESIAN_POINT ( 'NONE',  ( -77.62151472661336982, -283.5343936517504631, -206.6748295253652827 ) ) ;
#59168 = CARTESIAN_POINT ( 'NONE',  ( -91.90299058957434397, -285.2994675404841018, -216.0282036195645787 ) ) ;
#59169 = CARTESIAN_POINT ( 'NONE',  ( -1.045274000729234931, -284.4945023242057118, -336.6470681121771804 ) ) ;
#59170 = CARTESIAN_POINT ( 'NONE',  ( -87.73289502608102453, -285.0376039517623212, -212.0971533066257848 ) ) ;
#59171 = CARTESIAN_POINT ( 'NONE',  ( 5.575401975249509867, -290.6342601261230811, -208.9938232435833072 ) ) ;
#59172 = CARTESIAN_POINT ( 'NONE',  ( -111.7309490133388010, -277.6559685721651363, -289.8949852356172414 ) ) ;
#59173 = CARTESIAN_POINT ( 'NONE',  ( -54.42813229853332757, -277.3380690714490129, -195.3538533559490702 ) ) ;
#59174 = CARTESIAN_POINT ( 'NONE',  ( -48.18343439339471956, -275.1886040666647659, -506.6685929469949201 ) ) ;
#59175 = CARTESIAN_POINT ( 'NONE',  ( 20.66384458098975330, -285.7170958360764530, -225.3890456588433153 ) ) ;
#59176 = CARTESIAN_POINT ( 'NONE',  ( -43.17256257768601557, -288.0444856609815361, -346.8300237736628446 ) ) ;
#59177 = LINE ( 'NONE', #51133, #41552 ) ;
#59178 = CARTESIAN_POINT ( 'NONE',  ( -110.0676516180343754, -298.3159795585962115, -257.8161430496942899 ) ) ;
#59179 = CARTESIAN_POINT ( 'NONE',  ( -92.65981265102122677, -280.7042869482132232, -217.5738997647169981 ) ) ;
#59181 = CARTESIAN_POINT ( 'NONE',  ( 35.05432814463167546, -281.0881727064717097, -260.4507349593490630 ) ) ;
#59180 = CARTESIAN_POINT ( 'NONE',  ( -68.86336441560726485, -293.4845996708365305, -338.8207820590514530 ) ) ;
#59182 = CARTESIAN_POINT ( 'NONE',  ( 38.07101924524830849, -293.9133534756608697, -285.9149522766757627 ) ) ;
#59183 = CARTESIAN_POINT ( 'NONE',  ( -30.98025349358860225, -284.2117651929289650, -195.0563311550190519 ) ) ;
#59184 = CARTESIAN_POINT ( 'NONE',  ( -76.47137807786182861, -281.5293517993033561, -206.3176356285933082 ) ) ;
#59185 = CARTESIAN_POINT ( 'NONE',  ( -75.79176179874217212, -294.6375474653270885, -332.7500238143072693 ) ) ;
#59186 = CARTESIAN_POINT ( 'NONE',  ( -36.54089470230270820, -296.0620199789775029, -195.3613822856206639 ) ) ;
#59187 = ORIENTED_EDGE ( 'NONE', *, *, #6569, .F. ) ;
#59188 = LINE ( 'NONE', #87118, #71047 ) ;
#59189 = CARTESIAN_POINT ( 'NONE',  ( 34.92206208694674530, -283.7740998633518075, -289.1149191388742565 ) ) ;
#59190 = CARTESIAN_POINT ( 'NONE',  ( -110.4457867465490892, -296.0453469947829603, -271.4577890013238743 ) ) ;
#59191 = CARTESIAN_POINT ( 'NONE',  ( 154.1407330040854333, 249.5000000000000568, 13.42592592592592915 ) ) ;
#59192 = CARTESIAN_POINT ( 'NONE',  ( -67.68488546085839630, -295.1237833571632336, -207.2794874003663779 ) ) ;
#59193 = CARTESIAN_POINT ( 'NONE',  ( -29.84444656902484638, -273.3419492227055798, -193.8892276605981522 ) ) ;
#59194 = CARTESIAN_POINT ( 'NONE',  ( -105.7098950466958058, -290.7285624476944008, -244.6288303902620953 ) ) ;
#59195 = CARTESIAN_POINT ( 'NONE',  ( -54.67446553266402276, -281.3456057943258770, -198.6824275501904253 ) ) ;
#59196 = CARTESIAN_POINT ( 'NONE',  ( -64.88608884330454885, -275.2864340038062210, -201.8803645821617181 ) ) ;
#59197 = CARTESIAN_POINT ( 'NONE',  ( -58.24749520386723134, -284.9179244132961912, -343.6921444374638668 ) ) ;
#59198 = ADVANCED_FACE ( 'NONE', ( #73487 ), #37929, .T. ) ;
#59199 = CARTESIAN_POINT ( 'NONE',  ( -66.21182856767805447, -278.4605520009587281, -202.8666964932214398 ) ) ;
#59200 = CARTESIAN_POINT ( 'NONE',  ( 6.588326621156112672, -278.4556149077121177, -331.2130385379214772 ) ) ;
#59201 = VERTEX_POINT ( 'NONE', #59279 ) ;
#59202 = CARTESIAN_POINT ( 'NONE',  ( -93.17070340428988118, -273.1103786707471954, -217.3124288204401751 ) ) ;
#59203 = CARTESIAN_POINT ( 'NONE',  ( -104.8727395650716829, -292.8868704139201213, -239.0422273977443695 ) ) ;
#59204 = DIRECTION ( 'NONE',  ( -0.9849620900324524975, 0.000000000000000000, 0.1727706028203382094 ) ) ;
#59205 = ADVANCED_FACE ( 'NONE', ( #16183 ), #92511, .T. ) ;
#59206 = CARTESIAN_POINT ( 'NONE',  ( 198.6884013828325521, 64.61450673763174279, 9.555809373750800972 ) ) ;
#59207 = CARTESIAN_POINT ( 'NONE',  ( -44.69963521150854291, -293.2837783280903636, -345.8203413287523631 ) ) ;
#59208 = CARTESIAN_POINT ( 'NONE',  ( -11.46256119620454506, -273.9060860241622777, -201.9823683891267763 ) ) ;
#59209 = CARTESIAN_POINT ( 'NONE',  ( 196.1963538710216994, 282.2246705312485915, 13.99999999999999112 ) ) ;
#59210 = CARTESIAN_POINT ( 'NONE',  ( -64.16339541989695761, -293.2287500592112224, -198.8680281018717153 ) ) ;
#59211 = CARTESIAN_POINT ( 'NONE',  ( -4.829096099716510437, -276.9805209788416391, -202.7746430608542312 ) ) ;
#59212 = CARTESIAN_POINT ( 'NONE',  ( -11.40998174010726807, -288.3909272590983051, -200.1644342461136148 ) ) ;
#59213 = CARTESIAN_POINT ( 'NONE',  ( -8.043811174191334956, -274.6673593766132626, -339.2347260110625484 ) ) ;
#59214 = CARTESIAN_POINT ( 'NONE',  ( 26.62522777561350296, -277.9855948300413502, -308.4340260761187551 ) ) ;
#59216 = CARTESIAN_POINT ( 'NONE',  ( 32.89067710666319755, -291.9557184457170820, -295.1877136296014896 ) ) ;
#59215 = CIRCLE ( 'NONE', #18379, 26.04691768583017364 ) ;
#59217 = CARTESIAN_POINT ( 'NONE',  ( -110.1568037434600313, -280.6793131326099342, -249.4263104331916168 ) ) ;
#59218 = EDGE_LOOP ( 'NONE', ( #2393, #45917, #81571, #20454 ) ) ;
#59219 = CARTESIAN_POINT ( 'NONE',  ( -73.81103255392446272, -283.2171054920654001, -333.6806976298589689 ) ) ;
#59220 = CARTESIAN_POINT ( 'NONE',  ( -95.67965454365463529, -280.3061380527026927, -220.5596657276281292 ) ) ;
#59221 = CARTESIAN_POINT ( 'NONE',  ( -66.43970661227905339, -282.2197283635438225, -341.2364679255416036 ) ) ;
#59222 = CARTESIAN_POINT ( 'NONE',  ( 8.111420726632259104, -277.3891119227836271, -332.2883473100196738 ) ) ;
#59223 = DIRECTION ( 'NONE',  ( 0.000000000000000000, 0.000000000000000000, 1.000000000000000000 ) ) ;
#59224 = CARTESIAN_POINT ( 'NONE',  ( 36.60848089217793699, -276.8346664066436915, -251.5441447462659710 ) ) ;
#59225 = CARTESIAN_POINT ( 'NONE',  ( -102.0455923789670294, -287.4805209788416391, -239.2376011013261916 ) ) ;
#59226 = ORIENTED_EDGE ( 'NONE', *, *, #23628, .F. ) ;
#59227 = ORIENTED_EDGE ( 'NONE', *, *, #22848, .F. ) ;
#59228 = CARTESIAN_POINT ( 'NONE',  ( -110.8397082590496439, -298.3597315960658420, -285.3596097409123900 ) ) ;
#59229 = CARTESIAN_POINT ( 'NONE',  ( -70.37225221874938086, -292.6857564760307469, -204.9148904125863737 ) ) ;
#59230 = CARTESIAN_POINT ( 'NONE',  ( -74.86134914474827440, -275.5744971127168697, -334.8911322453533899 ) ) ;
#59231 = CARTESIAN_POINT ( 'NONE',  ( -51.47456847335546826, -290.9906497894075983, -345.0219245932429430 ) ) ;
#59232 = CARTESIAN_POINT ( 'NONE',  ( -72.66894332555671099, -290.9201509496366498, -206.3051867135904729 ) ) ;
#59233 = CARTESIAN_POINT ( 'NONE',  ( 14.55756891908503725, -287.8528824296484459, -327.2311315124798057 ) ) ;
#59234 = CARTESIAN_POINT ( 'NONE',  ( 139.6925840978351516, 0.000000000000000000, -21.50000000000000000 ) ) ;
#59235 = CARTESIAN_POINT ( 'NONE',  ( -81.11687103102769925, -282.0575584705125607, -329.8399852014875364 ) ) ;
#59236 = CARTESIAN_POINT ( 'NONE',  ( -91.47756380452071312, -291.6930371038618546, -321.2315699822405008 ) ) ;
#59237 = CARTESIAN_POINT ( 'NONE',  ( -71.48240004584029350, -284.0724622956608414, -205.0532290022398172 ) ) ;
#59238 = CARTESIAN_POINT ( 'NONE',  ( -38.37752109014439128, -281.3540799613490435, -196.8627803948396320 ) ) ;
#59239 = CARTESIAN_POINT ( 'NONE',  ( -112.0309622264713738, -291.2702822745546314, -288.1468021035003630 ) ) ;
#59240 = CARTESIAN_POINT ( 'NONE',  ( -62.33588742353349232, -280.2105521026131214, -201.6543885923783819 ) ) ;
#59241 = CARTESIAN_POINT ( 'NONE',  ( -61.54847960909332016, -290.5395757737460372, -197.6276065480706450 ) ) ;
#59242 = CARTESIAN_POINT ( 'NONE',  ( 38.81386786641555631, -288.2268739638572015, -260.1391669055101374 ) ) ;
#59243 = CARTESIAN_POINT ( 'NONE',  ( 32.81133645269277821, -288.4483560594792380, -301.9534962019183695 ) ) ;
#59244 = CARTESIAN_POINT ( 'NONE',  ( -37.28300403395834905, -286.2195510699564238, -197.3487029993409863 ) ) ;
#59245 = ORIENTED_EDGE ( 'NONE', *, *, #68227, .T. ) ;
#59246 = CARTESIAN_POINT ( 'NONE',  ( 175.2296996224750103, 149.6461846693799487, -24.00000000000001066 ) ) ;
#59247 = CARTESIAN_POINT ( 'NONE',  ( 16.59338243036610905, -294.6691324593296031, -217.0771901050731856 ) ) ;
#59248 = CARTESIAN_POINT ( 'NONE',  ( -112.7209512462045780, -295.0684851726238662, -283.7477506012513686 ) ) ;
#59249 = CARTESIAN_POINT ( 'NONE',  ( 16.69670121250682726, -275.3178931601833028, -319.8091583717057347 ) ) ;
#59250 = CARTESIAN_POINT ( 'NONE',  ( -14.83883542817090806, -297.6755480047640958, -193.4654597526000259 ) ) ;
#59251 = CARTESIAN_POINT ( 'NONE',  ( 36.11400074986045183, -292.1092963467750678, -276.2744723384471399 ) ) ;
#59252 = CARTESIAN_POINT ( 'NONE',  ( -102.0903711785251460, -295.2753630931429711, -234.5060819548803011 ) ) ;
#59253 = CARTESIAN_POINT ( 'NONE',  ( -2.263090077083370399, -293.7323999285008540, -205.8749799484477876 ) ) ;
#59254 = CARTESIAN_POINT ( 'NONE',  ( 27.75474069749391504, -294.1752578669907621, -236.6464406962314797 ) ) ;
#59255 = CARTESIAN_POINT ( 'NONE',  ( -43.46163685640959784, -256.7309459520654968, -442.5444711093502406 ) ) ;
#59256 = CARTESIAN_POINT ( 'NONE',  ( 31.72178143607572309, -291.9406376179620111, -300.1617040198403288 ) ) ;
#59257 = CARTESIAN_POINT ( 'NONE',  ( -110.3348684007941074, -298.3303865942214088, -287.6494786358357487 ) ) ;
#59258 = CARTESIAN_POINT ( 'NONE',  ( -110.4813975845010816, -291.5542706618424518, -265.7326542436144337 ) ) ;
#59259 = ADVANCED_FACE ( 'NONE', ( #66837 ), #2449, .F. ) ;
#59260 = CARTESIAN_POINT ( 'NONE',  ( -92.20375653846130604, -296.1977177104774910, -318.5507668010619113 ) ) ;
#59261 = EDGE_CURVE ( 'NONE', #1315, #78913, #56242, .T. ) ;
#59262 = CARTESIAN_POINT ( 'NONE',  ( -74.50265332788968919, -279.5238568493255116, -335.9162120704741028 ) ) ;
#59263 = CARTESIAN_POINT ( 'NONE',  ( -99.83642463930009114, -277.8247399392926695, -226.2282766793475446 ) ) ;
#59264 = EDGE_LOOP ( 'NONE', ( #17953, #38993 ) ) ;
#59265 = CARTESIAN_POINT ( 'NONE',  ( -60.83207967364867841, -273.1038588933913616, -197.0831979786206603 ) ) ;
#59266 = CARTESIAN_POINT ( 'NONE',  ( -4.207743384126525932, -280.6916773842535804, -337.0203642425162798 ) ) ;
#59267 = CARTESIAN_POINT ( 'NONE',  ( -112.9748177434362333, -276.8294893736833728, -280.0572769153680497 ) ) ;
#59268 = CARTESIAN_POINT ( 'NONE',  ( -98.73648959464510710, -277.1398640988450097, -226.9939846412351585 ) ) ;
#59269 = CARTESIAN_POINT ( 'NONE',  ( -60.65658042419239848, -296.4282212249879080, -200.6103780403647079 ) ) ;
#59270 = CARTESIAN_POINT ( 'NONE',  ( -111.1207100805108894, -274.7289146363895611, -256.6068679754121149 ) ) ;
#59271 = ADVANCED_FACE ( 'NONE', ( #88598 ), #16639, .T. ) ;
#59272 = CARTESIAN_POINT ( 'NONE',  ( 202.9738562182569694, 293.9636489450776367, -54.00000000000000000 ) ) ;
#59273 = AXIS2_PLACEMENT_3D ( 'NONE', #46989, #61699, #73230 ) ;
#59274 = CARTESIAN_POINT ( 'NONE',  ( -98.67728077941929143, -289.1647727934766294, -226.5849446631862065 ) ) ;
#59275 = CARTESIAN_POINT ( 'NONE',  ( -99.02913569081883338, -289.9388116324683438, -316.4661107424431634 ) ) ;
#59276 = CARTESIAN_POINT ( 'NONE',  ( -57.65134353210236640, -275.7908285796809764, -197.9361099450058248 ) ) ;
#59277 = CARTESIAN_POINT ( 'NONE',  ( -70.03608324650180350, -295.6202805425906490, -203.0476294105857278 ) ) ;
#59278 = CARTESIAN_POINT ( 'NONE',  ( -50.07683459419514804, -282.4077383118568605, -346.1907027889089363 ) ) ;
#59279 = CARTESIAN_POINT ( 'NONE',  ( -83.63170945779077670, -298.0521521680024080, -413.1172536214571096 ) ) ;
#59280 = AXIS2_PLACEMENT_3D ( 'NONE', #124, #65482, #15258 ) ;
#59281 = CARTESIAN_POINT ( 'NONE',  ( -61.07922065363230502, -281.3599954497074691, -341.5596076309277009 ) ) ;
#59282 = DIRECTION ( 'NONE',  ( 0.000000000000000000, -1.000000000000000000, 0.000000000000000000 ) ) ;
#59283 = CARTESIAN_POINT ( 'NONE',  ( 31.20467217984041142, -291.9985318348604437, -244.1213514528446353 ) ) ;
#59284 = CARTESIAN_POINT ( 'NONE',  ( -106.7108908541011232, -283.0388164732166274, -243.9266545574677991 ) ) ;
#59285 = CARTESIAN_POINT ( 'NONE',  ( 197.7051530045995094, 41.80213891112349245, 12.00000000000000355 ) ) ;
#59286 = DIRECTION ( 'NONE',  ( 0.9951408606192334583, 0.000000000000000000, -0.09846150276129006507 ) ) ;
#59287 = CARTESIAN_POINT ( 'NONE',  ( 30.55977380720766590, -291.1318313154431507, -238.3889629391739788 ) ) ;
#59288 = CARTESIAN_POINT ( 'NONE',  ( -39.15724095186205744, -278.6754442855039429, -344.1387855290308835 ) ) ;
#59289 = CARTESIAN_POINT ( 'NONE',  ( -74.07203019836173041, -284.7337305507470546, -337.6429991239047013 ) ) ;
#59291 = CARTESIAN_POINT ( 'NONE',  ( -109.4211293791368860, -284.7056479251183418, -258.7253007642735838 ) ) ;
#59290 = CARTESIAN_POINT ( 'NONE',  ( 21.64975101761049103, -272.9873163552364872, -223.1248852418183333 ) ) ;
#59292 = CARTESIAN_POINT ( 'NONE',  ( 32.66427146491945877, -277.2759605079883158, -293.0445669804720410 ) ) ;
#59293 = CARTESIAN_POINT ( 'NONE',  ( 0.9646667953329586265, -277.3299508537898532, -332.7522152491944212 ) ) ;
#59294 = CARTESIAN_POINT ( 'NONE',  ( -95.60224190837091385, -285.9016969008304159, -317.6116841705833167 ) ) ;
#59295 = EDGE_LOOP ( 'NONE', ( #39735, #10312, #25660, #47300 ) ) ;
#59296 = CARTESIAN_POINT ( 'NONE',  ( 222.4306832106270804, -135.2391364535880882, 21.50000000000000000 ) ) ;
#59297 = CARTESIAN_POINT ( 'NONE',  ( -94.65299584153534340, -295.6875769930560978, -321.8046426537650291 ) ) ;
#59298 = CARTESIAN_POINT ( 'NONE',  ( 33.39133284039870375, -289.2222221650000051, -246.5140039186179024 ) ) ;
#59299 = CARTESIAN_POINT ( 'NONE',  ( 195.4709818679464490, 27.30234762113502711, 15.00000000000000000 ) ) ;
#59300 = CARTESIAN_POINT ( 'NONE',  ( -2.659677404128736544, -286.1237833571631768, -342.4524372437778652 ) ) ;
#59301 = CARTESIAN_POINT ( 'NONE',  ( -59.20082964342246612, -278.6959951863848346, -196.8514521837713858 ) ) ;
#59302 = CARTESIAN_POINT ( 'NONE',  ( -33.55848996007854623, -290.4989048911011196, -194.2550884100214716 ) ) ;
#59303 = CARTESIAN_POINT ( 'NONE',  ( -106.8209977280125855, -285.7466650322019746, -295.0758368735749286 ) ) ;
#59304 = CARTESIAN_POINT ( 'NONE',  ( -70.21020943911518941, -281.3731126325400851, -204.0324103728401610 ) ) ;
#59305 = CARTESIAN_POINT ( 'NONE',  ( 39.05056830386127587, -288.9562309325569913, -268.6795665767796208 ) ) ;
#59306 = CARTESIAN_POINT ( 'NONE',  ( 36.29310367044358543, -283.3685413929187007, -256.0487072342228885 ) ) ;
#59307 = CARTESIAN_POINT ( 'NONE',  ( -5.282839820566376687, -276.8084873451835506, -340.3698994339844148 ) ) ;
#59308 = CARTESIAN_POINT ( 'NONE',  ( -34.37347169243706446, -296.1095954194135516, -195.7173170109917351 ) ) ;
#59309 = CARTESIAN_POINT ( 'NONE',  ( -39.58513240509605424, -279.8580645595582723, -193.3807559228765172 ) ) ;
#59310 = CARTESIAN_POINT ( 'NONE',  ( -80.58402723695006387, -299.3808182795068547, -209.7689126954684582 ) ) ;
#59311 = CARTESIAN_POINT ( 'NONE',  ( 156.4851178187871312, 15.24064981607324754, 6.999999999998999023 ) ) ;
#59312 = CARTESIAN_POINT ( 'NONE',  ( -54.42813229853333468, -279.7662352645560304, -345.3683826091709648 ) ) ;
#59313 = CARTESIAN_POINT ( 'NONE',  ( -103.3381623678167216, -271.2889261532651517, -232.5933796212814286 ) ) ;
#59314 = FACE_OUTER_BOUND ( 'NONE', #16691, .T. ) ;
#59315 = CARTESIAN_POINT ( 'NONE',  ( -27.54392032566019566, -279.6874896496641441, -197.9082815646748941 ) ) ;
#59316 = CARTESIAN_POINT ( 'NONE',  ( -8.022344194352687197, -277.8816078899575359, -341.1452680859304678 ) ) ;
#59317 = CARTESIAN_POINT ( 'NONE',  ( -71.64438704873737152, -282.5530624709564336, -339.0353189897990660 ) ) ;
#59318 = CARTESIAN_POINT ( 'NONE',  ( -61.56580197023708223, -291.1313803830333313, -340.2979959691291469 ) ) ;
#59319 = CARTESIAN_POINT ( 'NONE',  ( -54.45863097250634866, -299.3562124186790356, -195.9990414290667218 ) ) ;
#59320 = CARTESIAN_POINT ( 'NONE',  ( 7.683387436728358111, -299.8091520019872291, -193.7491945106231697 ) ) ;
#59321 = CARTESIAN_POINT ( 'NONE',  ( -25.13450700442725605, -294.2081860212998095, -196.4773743154284773 ) ) ;
#59322 = CARTESIAN_POINT ( 'NONE',  ( 35.23983971529512615, -279.3168326724843951, -252.0895293219945756 ) ) ;
#59323 = CARTESIAN_POINT ( 'NONE',  ( -59.35101031626653167, -285.2593207658308074, -341.5272172051828079 ) ) ;
#59324 = CARTESIAN_POINT ( 'NONE',  ( -59.95035027100280445, -271.7779839509131534, -199.1684437841001625 ) ) ;
#59325 = CARTESIAN_POINT ( 'NONE',  ( -113.0274302840048790, -286.2639703026810594, -261.5230941430026519 ) ) ;
#59326 = EDGE_CURVE ( 'NONE', #37103, #24392, #16953, .T. ) ;
#59327 = CARTESIAN_POINT ( 'NONE',  ( -70.12298574114360861, -288.4148760625993191, -335.9464746435422740 ) ) ;
#59328 = CARTESIAN_POINT ( 'NONE',  ( -103.0630025851773865, -256.8465833436261505, -326.7099068919612250 ) ) ;
#59329 = VERTEX_POINT ( 'NONE', #24202 ) ;
#59330 = CARTESIAN_POINT ( 'NONE',  ( 5.213997448806920509, -287.0633906515332683, -333.8246421162912725 ) ) ;
#59331 = CARTESIAN_POINT ( 'NONE',  ( -80.42340096351985324, -289.3206278847395083, -329.3821154119235075 ) ) ;
#59332 = VERTEX_POINT ( 'NONE', #53079 ) ;
#59333 = CARTESIAN_POINT ( 'NONE',  ( -10.11660708030318823, -287.4789080717545176, -198.6087559490982244 ) ) ;
#59334 = CARTESIAN_POINT ( 'NONE',  ( 34.86192568907098632, -275.7406304692809158, -259.3809695100936210 ) ) ;
#59335 = CARTESIAN_POINT ( 'NONE',  ( 35.16489085092543831, -292.1544512647576539, -245.2145508401879113 ) ) ;
#59336 = CARTESIAN_POINT ( 'NONE',  ( 36.38333763275200994, -282.4802768894000451, -292.4060171876651566 ) ) ;
#59337 = CARTESIAN_POINT ( 'NONE',  ( 36.87856427347627175, -283.2965720612031646, -288.1386546930356189 ) ) ;
#59338 = CARTESIAN_POINT ( 'NONE',  ( -61.22108016712463296, -283.6870853797404948, -343.5982009010909337 ) ) ;
#59339 = CARTESIAN_POINT ( 'NONE',  ( 15.27167089700801483, -281.1538305122716110, -219.6537169291917451 ) ) ;
#59340 = CARTESIAN_POINT ( 'NONE',  ( -105.5937364680635966, -293.8380690714490129, -285.9065529553535612 ) ) ;
#59341 = CARTESIAN_POINT ( 'NONE',  ( -63.41909885852727058, -182.9725237402124947, -362.5579290312759895 ) ) ;
#59342 = ORIENTED_EDGE ( 'NONE', *, *, #27631, .T. ) ;
#59343 = AXIS2_PLACEMENT_3D ( 'NONE', #41401, #27701, #70790 ) ;
#59344 = CARTESIAN_POINT ( 'NONE',  ( -88.32644975019017863, -279.7686299980030071, -325.1387021782032321 ) ) ;
#59345 = CARTESIAN_POINT ( 'NONE',  ( 196.7050999029026741, 285.3698064150070195, -111.6815863925781116 ) ) ;
#59346 = AXIS2_PLACEMENT_3D ( 'NONE', #11301, #40154, #69071 ) ;
#59347 = CARTESIAN_POINT ( 'NONE',  ( -109.9067179730154322, -295.7788906872280563, -279.6105235613302398 ) ) ;
#59348 = CARTESIAN_POINT ( 'NONE',  ( 39.16563853981011789, -292.9518892385784739, -261.7390483411336959 ) ) ;
#59349 = CARTESIAN_POINT ( 'NONE',  ( 26.24832809216016116, -24.45034260803730675, -341.6199306126845272 ) ) ;
#59350 = VECTOR ( 'NONE', #30154, 1000.000000000000000 ) ;
#59352 = CARTESIAN_POINT ( 'NONE',  ( -29.10383471639088881, -287.3458804985839379, -343.6999070914222898 ) ) ;
#59351 = CARTESIAN_POINT ( 'NONE',  ( -109.6303901606406157, -271.5548738973836294, -245.3083024605653577 ) ) ;
#59353 = CARTESIAN_POINT ( 'NONE',  ( -108.0384440827360919, -298.1152945166665518, -293.1732387303364931 ) ) ;
#59354 = CARTESIAN_POINT ( 'NONE',  ( -44.08619489208993514, -287.2802689358219368, -197.1780921612973145 ) ) ;
#59355 = VERTEX_POINT ( 'NONE', #43660 ) ;
#59356 = CARTESIAN_POINT ( 'NONE',  ( -74.48198181312594102, -296.4745945953837918, -337.6026333411576275 ) ) ;
#59357 = AXIS2_PLACEMENT_3D ( 'NONE', #50029, #78923, #14072 ) ;
#59358 = CARTESIAN_POINT ( 'NONE',  ( -49.43788583444410989, -286.3862593689379423, -198.2563260900890612 ) ) ;
#59359 = CARTESIAN_POINT ( 'NONE',  ( -106.1498907570397989, -295.7816561999024998, -236.6944932656572576 ) ) ;
#59360 = CARTESIAN_POINT ( 'NONE',  ( 24.67806120022697414, -293.7514493957186232, -224.9991512524795212 ) ) ;
#59361 = CARTESIAN_POINT ( 'NONE',  ( 38.79006878958215765, -293.9009414740083912, -258.8916612788188445 ) ) ;
#59362 = CARTESIAN_POINT ( 'NONE',  ( -102.4105294853175110, -291.1696053634590839, -237.1577128703661401 ) ) ;
#59363 = EDGE_LOOP ( 'NONE', ( #76100, #73071, #50496, #54137 ) ) ;
#59364 = CARTESIAN_POINT ( 'NONE',  ( -47.80257052418233599, -229.5268262511776527, 21.50000000000000000 ) ) ;
#59365 = CARTESIAN_POINT ( 'NONE',  ( -91.16087824626904990, -275.2146166960715732, -217.3251842788459953 ) ) ;
#59366 = CARTESIAN_POINT ( 'NONE',  ( -7.829295294427161878, -273.2251692674003607, -199.6151562959837804 ) ) ;
#59367 = EDGE_LOOP ( 'NONE', ( #76666, #79513, #73108, #31697 ) ) ;
#59368 = CARTESIAN_POINT ( 'NONE',  ( -28.61424944481396082, -276.4520750048379796, -346.8565137576001121 ) ) ;
#59369 = CARTESIAN_POINT ( 'NONE',  ( -101.4021778827159750, -271.4498995545723687, -233.6155905375105135 ) ) ;
#59370 = CARTESIAN_POINT ( 'NONE',  ( -109.4957424123521719, -280.6390270605056685, -252.9066152519873754 ) ) ;
#59371 = CARTESIAN_POINT ( 'NONE',  ( 6.100763367172952201, -274.5956598465853062, -330.6210762945250394 ) ) ;
#59372 = CARTESIAN_POINT ( 'NONE',  ( -79.04215355750585559, -274.5550213912567870, -210.0060134684726734 ) ) ;
#59373 = CARTESIAN_POINT ( 'NONE',  ( -87.50316644905679198, -274.2729004289537897, -216.9321784089285927 ) ) ;
#59374 = CARTESIAN_POINT ( 'NONE',  ( -96.16606327408037203, -274.9668513061713497, -222.2402007114817195 ) ) ;
#59375 = CARTESIAN_POINT ( 'NONE',  ( -89.01620676094657370, -271.3506796356424502, -215.4432606239321046 ) ) ;
#59376 = CARTESIAN_POINT ( 'NONE',  ( -20.81707905155414551, -295.4859505330491061, -341.6230544575838053 ) ) ;
#59377 = CARTESIAN_POINT ( 'NONE',  ( 36.01032612811046363, -292.2041307392824478, -276.2649438748000534 ) ) ;
#59378 = LINE ( 'NONE', #1600, #47206 ) ;
#59379 = CARTESIAN_POINT ( 'NONE',  ( -84.82347076495847205, -278.1790308836919507, -330.9681225577662076 ) ) ;
#59380 = EDGE_CURVE ( 'NONE', #1828, #48224, #47594, .T. ) ;
#59381 = CARTESIAN_POINT ( 'NONE',  ( 9.483454273817326197, -274.8834623247841478, -214.2913085253646273 ) ) ;
#59382 = CARTESIAN_POINT ( 'NONE',  ( -109.7632989416309215, -282.9242008817736860, -295.0270924731030391 ) ) ;
#59383 = CARTESIAN_POINT ( 'NONE',  ( -111.8321738028380139, -298.4185626551264363, -280.8010832467707587 ) ) ;
#59384 = DIRECTION ( 'NONE',  ( 0.000000000000000000, -0.000000000000000000, 1.000000000000000000 ) ) ;
#59385 = CARTESIAN_POINT ( 'NONE',  ( -49.43818209431198341, -285.0912880699073071, -198.1549721843069563 ) ) ;
#59386 = CARTESIAN_POINT ( 'NONE',  ( -75.84130907448532355, -281.5643120534360833, -334.9800432270934039 ) ) ;
#59387 = CARTESIAN_POINT ( 'NONE',  ( -95.25983415955553824, -276.1499783695610972, -316.4624256863126561 ) ) ;
#59388 = CARTESIAN_POINT ( 'NONE',  ( -39.19061369774771464, -275.6505329688265533, -343.9271185348336530 ) ) ;
#59389 = CARTESIAN_POINT ( 'NONE',  ( -74.50844179344917961, -281.5579757296370644, -205.2033703588862750 ) ) ;
#59390 = CARTESIAN_POINT ( 'NONE',  ( 35.75082462417807960, -276.8448686515374106, -277.0404390222568622 ) ) ;
#59391 = CARTESIAN_POINT ( 'NONE',  ( 175.2296996224750103, 160.0000000000000568, 0.000000000000000000 ) ) ;
#59392 = CARTESIAN_POINT ( 'NONE',  ( 23.01182561612909439, -273.3244948249692925, -223.8222162592490747 ) ) ;
#59393 = CARTESIAN_POINT ( 'NONE',  ( 7.433536390348085554, -282.6608750066078528, -209.9208858560567421 ) ) ;
#59394 = CARTESIAN_POINT ( 'NONE',  ( 184.7149167944524493, -12.49482340714361506, -3.999999999999998224 ) ) ;
#59395 = CARTESIAN_POINT ( 'NONE',  ( -21.31371410187765747, -288.1763352625901575, -196.5206286891323657 ) ) ;
#59396 = CARTESIAN_POINT ( 'NONE',  ( 221.4259212729440094, 36.93618551656547311, 10.00000000000000000 ) ) ;
#59397 = CARTESIAN_POINT ( 'NONE',  ( -109.9848977622940822, -288.3117371638712712, -289.0657481500286394 ) ) ;
#59398 = CARTESIAN_POINT ( 'NONE',  ( 104.1717476309105166, -299.5541904835127980, -192.9651424135224715 ) ) ;
#59399 = CARTESIAN_POINT ( 'NONE',  ( -66.96560624799985817, -296.4499545823885001, -203.1941472263000037 ) ) ;
#59400 = CARTESIAN_POINT ( 'NONE',  ( -68.29498457575172665, -289.7807955726265163, -202.8730130505828981 ) ) ;
#59401 = CARTESIAN_POINT ( 'NONE',  ( 181.0595704366054690, 252.2700355933461651, -164.3583243123303532 ) ) ;
#59402 = CARTESIAN_POINT ( 'NONE',  ( 197.1123855246551955, 18.41506350946087522, -10.91506350946096759 ) ) ;
#59403 = CARTESIAN_POINT ( 'NONE',  ( 28.29739534131069334, -286.5436382617302797, -309.2740579564660379 ) ) ;
#59404 = CARTESIAN_POINT ( 'NONE',  ( -56.50723799855340701, -284.9034545936958125, -341.6290811309229412 ) ) ;
#59405 = CARTESIAN_POINT ( 'NONE',  ( -96.77363491790653427, -283.4344158946931316, -223.0132653902421680 ) ) ;
#59406 = CARTESIAN_POINT ( 'NONE',  ( -55.01235538456789698, -291.8185185253624354, -199.5321130283295474 ) ) ;
#59407 = CARTESIAN_POINT ( 'NONE',  ( 21.79171467867494627, -282.3679249526834951, -226.5379279028655901 ) ) ;
#59408 = CARTESIAN_POINT ( 'NONE',  ( 34.22100641308983171, -282.1540124790445248, -255.0902615840891485 ) ) ;
#59409 = CARTESIAN_POINT ( 'NONE',  ( -20.83168193446944017, -290.8212955227522230, -343.9389450386367457 ) ) ;
#59410 = CIRCLE ( 'NONE', #50339, 7.500000000000012434 ) ;
#59411 = CARTESIAN_POINT ( 'NONE',  ( -111.7989246941215242, -273.1324427340867942, -250.6156770818635096 ) ) ;
#59412 = AXIS2_PLACEMENT_3D ( 'NONE', #67857, #46978, #9134 ) ;
#59413 = CARTESIAN_POINT ( 'NONE',  ( -10.10563266378761504, -286.7791811971883362, -340.8416885479788334 ) ) ;
#59414 = CARTESIAN_POINT ( 'NONE',  ( 38.21874907175163116, -275.3668134746865235, -255.5415863867415283 ) ) ;
#59415 = CARTESIAN_POINT ( 'NONE',  ( -63.39798318223426321, -293.6908444651630248, -200.4117297377376588 ) ) ;
#59416 = FACE_OUTER_BOUND ( 'NONE', #76339, .T. ) ;
#59417 = CARTESIAN_POINT ( 'NONE',  ( -114.2704648735229114, -281.0519495502701943, -270.3937649182068981 ) ) ;
#59418 = AXIS2_PLACEMENT_3D ( 'NONE', #29938, #74890, #88605 ) ;
#59420 = VECTOR ( 'NONE', #38695, 1000.000000000000000 ) ;
#59419 = CARTESIAN_POINT ( 'NONE',  ( -95.64882087972777924, -275.8997473816919523, -317.8186939487128484 ) ) ;
#59421 = LINE ( 'NONE', #15865, #23683 ) ;
#59422 = CARTESIAN_POINT ( 'NONE',  ( -37.58444860191104908, -296.4490387548829062, -194.1615018943762152 ) ) ;
#59423 = CARTESIAN_POINT ( 'NONE',  ( 21.56824034799850054, -274.2951488592610190, -227.0770379815169235 ) ) ;
#59424 = CIRCLE ( 'NONE', #60898, 0.5000000000000004441 ) ;
#59425 = CARTESIAN_POINT ( 'NONE',  ( -93.98506786433267735, -292.7349535946738115, -223.2008064314894966 ) ) ;
#59426 = PRODUCT_DEFINITION_SHAPE ( 'NONE', 'NONE',  #74824 ) ;
#59427 = CARTESIAN_POINT ( 'NONE',  ( -103.7747757442157024, -291.9081258858419119, -239.5381571974824624 ) ) ;
#59428 = CARTESIAN_POINT ( 'NONE',  ( -95.06137381201850189, -285.6663020936589987, -316.7106706680724528 ) ) ;
#59429 = CARTESIAN_POINT ( 'NONE',  ( -16.80257704382437822, -293.7376704602239670, -196.7625397737684807 ) ) ;
#59430 = CARTESIAN_POINT ( 'NONE',  ( 21.81721147078295076, -294.2116305041512874, -221.8480119889270270 ) ) ;
#59431 = CARTESIAN_POINT ( 'NONE',  ( 34.83764836775974061, -293.5337975443893583, -281.6050554926152927 ) ) ;
#59432 = CARTESIAN_POINT ( 'NONE',  ( 31.26459995428608352, -289.9507104240859121, -300.7914908447457947 ) ) ;
#59433 = CARTESIAN_POINT ( 'NONE',  ( 39.18252616323609772, -281.6061084499941671, -261.3478582940723527 ) ) ;
#59434 = CARTESIAN_POINT ( 'NONE',  ( -48.72838308939262930, -295.9882174061281717, -195.6113508563573191 ) ) ;
#59435 = CARTESIAN_POINT ( 'NONE',  ( -113.5996787024089940, -284.2473939294193883, -281.4017867208951884 ) ) ;
#59436 = CARTESIAN_POINT ( 'NONE',  ( 26.67372381193292341, -277.0144087605440859, -231.8700111909702457 ) ) ;
#59437 = CARTESIAN_POINT ( 'NONE',  ( -39.97286786938623493, -284.8132791601767622, -197.0112204908242859 ) ) ;
#59438 = CARTESIAN_POINT ( 'NONE',  ( 22.28724812464620442, -284.9291229503145360, -224.8495131303380106 ) ) ;
#59439 = CARTESIAN_POINT ( 'NONE',  ( -111.7781241848990561, -276.8721574554319318, -256.1665410827072265 ) ) ;
#59440 = CARTESIAN_POINT ( 'NONE',  ( 163.5244876965996923, 234.8495348041943487, -191.6304063886470317 ) ) ;
#59441 = CARTESIAN_POINT ( 'NONE',  ( -107.0464464074657229, -283.7698934295147524, -292.2525954982224334 ) ) ;
#59442 = CARTESIAN_POINT ( 'NONE',  ( 33.20626902981570083, -283.1406163705468089, -300.3461481427333410 ) ) ;
#59443 = CARTESIAN_POINT ( 'NONE',  ( -97.98113466564090857, -288.9803757194330842, -317.4321195966422806 ) ) ;
#59444 = CARTESIAN_POINT ( 'NONE',  ( -38.51202282107968955, -278.6667189247613123, -346.5521329573720664 ) ) ;
#59445 = CARTESIAN_POINT ( 'NONE',  ( 3.254116427783104726, -277.8343752899252763, -335.2716025056482749 ) ) ;
#59446 = CARTESIAN_POINT ( 'NONE',  ( -38.35172133784325155, -279.8724661127399713, -197.3557049113782966 ) ) ;
#59447 = CARTESIAN_POINT ( 'NONE',  ( -69.00266535042828764, -275.6136816638878599, -202.7495500415424203 ) ) ;
#59448 = CARTESIAN_POINT ( 'NONE',  ( -113.3907224302259351, -292.2128699707654960, -265.5666815589217435 ) ) ;
#59449 = AXIS2_PLACEMENT_3D ( 'NONE', #91418, #68731, #40739 ) ;
#59450 = CARTESIAN_POINT ( 'NONE',  ( -38.36032238474562917, -293.9855441888782366, -343.6631539932238297 ) ) ;
#59451 = VERTEX_POINT ( 'NONE', #74884 ) ;
#59452 = CARTESIAN_POINT ( 'NONE',  ( -7.983701101779252518, -294.3233663998176439, -337.2342186125437706 ) ) ;
#59453 = CARTESIAN_POINT ( 'NONE',  ( -112.8265981925139698, -291.4607813343548059, -283.9822746103509417 ) ) ;
#59454 = CARTESIAN_POINT ( 'NONE',  ( -24.86714133654969316, -280.8669230423494128, -198.3314154228249606 ) ) ;
#59455 = CARTESIAN_POINT ( 'NONE',  ( -85.65083665714618633, -272.4608488318901891, -210.7033645879270125 ) ) ;
#59456 = CARTESIAN_POINT ( 'NONE',  ( 35.74954845533157766, -287.9006080393311322, -246.2956489235986339 ) ) ;
#59457 = CARTESIAN_POINT ( 'NONE',  ( -9.566999919184999257, -289.0322528267125222, -342.1546435947208238 ) ) ;
#59458 = CARTESIAN_POINT ( 'NONE',  ( -57.40426851425257126, -286.1193949603739952, -200.0975146608287503 ) ) ;
#59459 = CYLINDRICAL_SURFACE ( 'NONE', #38380, 1.895975569037589015 ) ;
#59460 = CARTESIAN_POINT ( 'NONE',  ( -110.3856735362975741, -264.4859968940625095, -306.0548468009229168 ) ) ;
#59461 = CARTESIAN_POINT ( 'NONE',  ( -55.39694311004227956, -169.5609126108696501, -360.5716228430129604 ) ) ;
#59462 = CARTESIAN_POINT ( 'NONE',  ( -54.00061198648864291, -276.4685664602649240, -341.6529881661105605 ) ) ;
#59463 = CARTESIAN_POINT ( 'NONE',  ( -94.70346862234369212, -276.8303379994504780, -316.0304190598139371 ) ) ;
#59464 = CARTESIAN_POINT ( 'NONE',  ( -105.5882314637777171, -272.6796843899326177, -234.6347546966848654 ) ) ;
#59465 = CARTESIAN_POINT ( 'NONE',  ( -37.61793092032886676, -140.8427143539732924, -362.0657075832283454 ) ) ;
#59466 = CARTESIAN_POINT ( 'NONE',  ( -37.14515683742537533, -275.7345374253613386, -346.8806914234819487 ) ) ;
#59467 = CARTESIAN_POINT ( 'NONE',  ( -61.25117269039499490, -297.1184331212925827, -342.5431654630265257 ) ) ;
#59468 = CARTESIAN_POINT ( 'NONE',  ( -77.29404590694403510, -291.9926306616621901, -209.1908759662587727 ) ) ;
#59469 = CARTESIAN_POINT ( 'NONE',  ( -75.70816543095332918, -298.3568837329264625, -203.7254810194878019 ) ) ;
#59470 = CARTESIAN_POINT ( 'NONE',  ( -48.14994351211366563, -287.8772227586073313, -343.1065388092864055 ) ) ;
#59471 = CARTESIAN_POINT ( 'NONE',  ( -81.19906796063573040, -274.1250001016468900, -207.1313751103526215 ) ) ;
#59472 = CARTESIAN_POINT ( 'NONE',  ( -95.29036390310834292, -297.3436202330551055, -225.9453400958412033 ) ) ;
#59473 = VERTEX_POINT ( 'NONE', #90903 ) ;
#59474 = CARTESIAN_POINT ( 'NONE',  ( 164.2231345125756263, 276.0000000000000568, 22.80382896337009058 ) ) ;
#59475 = CARTESIAN_POINT ( 'NONE',  ( -87.98476698147007369, -281.2704282057558771, -214.2844385576136688 ) ) ;
#59476 = EDGE_CURVE ( 'NONE', #20191, #33307, #4302, .T. ) ;
#59477 = B_SPLINE_CURVE_WITH_KNOTS ( 'NONE', 3,
 ( #81712, #82190, #59029, #30146, #44801, #17344, #52377, #87876 ),
 .UNSPECIFIED., .F., .F.,
 ( 4, 2, 2, 4 ),
 ( 0.001027591722192180415, 0.003123856272695763915, 0.005220120823199347199, 0.009412649924206491214 ),
 .UNSPECIFIED. ) ;
#59478 = CARTESIAN_POINT ( 'NONE',  ( -13.44700422291602848, -282.2576332801950230, -343.4950390501155084 ) ) ;
#59479 = AXIS2_PLACEMENT_3D ( 'NONE', #74994, #1157, #30040 ) ;
#59480 = AXIS2_PLACEMENT_3D ( 'NONE', #83799, #83323, #84729 ) ;
#59481 = CARTESIAN_POINT ( 'NONE',  ( -101.0873446707604444, -280.1255602741742905, -234.1572663263705181 ) ) ;
#59482 = CARTESIAN_POINT ( 'NONE',  ( -112.7149554263138782, -280.4394902463442918, -260.3242335047801816 ) ) ;
#59483 = CARTESIAN_POINT ( 'NONE',  ( -57.02838620769510669, -272.2735827212886761, -199.2928208727300614 ) ) ;
#59484 = DIRECTION ( 'NONE',  ( 0.000000000000000000, 0.000000000000000000, 1.000000000000000000 ) ) ;
#59485 = CARTESIAN_POINT ( 'NONE',  ( 205.2296996224750103, 68.12454877777268791, 0.000000000000000000 ) ) ;
#59486 = CARTESIAN_POINT ( 'NONE',  ( -14.31088965566074478, -280.5258175663214502, -201.0358828618031453 ) ) ;
#59487 = VECTOR ( 'NONE', #67913, 1000.000000000000114 ) ;
#59488 = CARTESIAN_POINT ( 'NONE',  ( 39.46917076413583203, -276.3291498178131746, -268.2998240233352476 ) ) ;
#59489 = CARTESIAN_POINT ( 'NONE',  ( 36.74780484157432880, -277.4016548818336787, -258.6275084797254635 ) ) ;
#59490 = CARTESIAN_POINT ( 'NONE',  ( -72.58517864369669326, -276.0841571366627250, -338.1732291633564387 ) ) ;
#59491 = ORIENTED_EDGE ( 'NONE', *, *, #10705, .T. ) ;
#59492 = DIRECTION ( 'NONE',  ( 0.000000000000000000, 0.000000000000000000, -1.000000000000000000 ) ) ;
#59493 = CARTESIAN_POINT ( 'NONE',  ( 36.53804865116615019, -283.7216709875748393, -285.1999025138948696 ) ) ;
#59494 = CIRCLE ( 'NONE', #53463, 25.50000000000000355 ) ;
#59495 = CARTESIAN_POINT ( 'NONE',  ( -17.37873647507503350, -291.5134670732281279, -199.9231682902452576 ) ) ;
#59496 = EDGE_CURVE ( 'NONE', #39706, #83798, #62315, .T. ) ;
#59497 = CARTESIAN_POINT ( 'NONE',  ( 23.78546316888671086, -286.2776520295481077, -223.6835217691885305 ) ) ;
#59498 = CARTESIAN_POINT ( 'NONE',  ( -93.34031160941609073, -282.1117546277640713, -318.7759647947202097 ) ) ;
#59499 = CARTESIAN_POINT ( 'NONE',  ( -66.81207807889211381, -282.0207516297173242, -337.8052960318701707 ) ) ;
#59500 = CARTESIAN_POINT ( 'NONE',  ( 5.140561975330038891, -281.8462486122599557, -210.5080653418146710 ) ) ;
#59501 = CARTESIAN_POINT ( 'NONE',  ( -96.22655637268795203, -271.1898637074183398, -223.9114209064198917 ) ) ;
#59503 = CARTESIAN_POINT ( 'NONE',  ( 22.75923767732920311, -280.5846590842179467, -317.2257417157809414 ) ) ;
#59502 = B_SPLINE_CURVE_WITH_KNOTS ( 'NONE', 3,
 ( #6051, #63837, #34923, #78488, #71389, #6521, #29221, #86030, #336, #50048, #21652, #14095, #79426, #86964, #22117, #12699, #62071, #46438, #10924, #47842, #54485, #90905, #40724, #28323, #12341, #76281, #19446, #62560, #61159, #4304 ),
 .UNSPECIFIED., .F., .F.,
 ( 4, 2, 2, 2, 2, 2, 2, 2, 2, 2, 2, 2, 2, 2, 4 ),
 ( 0.01214138644550194837, 0.01289762902330727004, 0.01365387160111258998, 0.01441011417891791165, 0.01516635675672323331, 0.01667884191233387492, 0.01743508449013913761, 0.01819132706794440030, 0.01970381222355477649, 0.02046005480135993509, 0.02121629737916509023, 0.02197253995697024537, 0.02272878253477540050, 0.02348502511258055564, 0.02424126769038571078 ),
 .UNSPECIFIED. ) ;
#59504 = CARTESIAN_POINT ( 'NONE',  ( 36.39574039698510433, -295.7291575815638680, -284.1343034324547148 ) ) ;
#59505 = VECTOR ( 'NONE', #82669, 1000.000000000000000 ) ;
#59506 = CARTESIAN_POINT ( 'NONE',  ( -93.67929177431585686, -278.5438956382691345, -316.9636477778738026 ) ) ;
#59507 = CARTESIAN_POINT ( 'NONE',  ( -21.39826594332415510, -288.2563288105177435, -196.9047681559327430 ) ) ;
#59508 = DIRECTION ( 'NONE',  ( -0.000000000000000000, -0.000000000000000000, 1.000000000000000000 ) ) ;
#59509 = CARTESIAN_POINT ( 'NONE',  ( -72.78039021578420886, -293.5067239843279481, -203.6125944749465475 ) ) ;
#59510 = CIRCLE ( 'NONE', #71628, 2.500000000000002220 ) ;
#59511 = CARTESIAN_POINT ( 'NONE',  ( 37.37295766519621054, -273.4607588509501284, -263.2559345594654587 ) ) ;
#59512 = CARTESIAN_POINT ( 'NONE',  ( -29.00488113929756651, -288.1463427626158023, -346.7994529033159097 ) ) ;
#59513 = CARTESIAN_POINT ( 'NONE',  ( 34.55015722702925274, -292.1702439063636803, -287.0900927647830940 ) ) ;
#59514 = CARTESIAN_POINT ( 'NONE',  ( -48.18343439306194398, -280.8036219927305410, -430.6712033366062542 ) ) ;
#59515 = CARTESIAN_POINT ( 'NONE',  ( -103.5827141873963200, -276.8077934971782952, -302.3124250561784265 ) ) ;
#59516 = CARTESIAN_POINT ( 'NONE',  ( -108.6391984751745952, -294.9606741339634937, -249.6842659269705393 ) ) ;
#59517 = CARTESIAN_POINT ( 'NONE',  ( -98.51191275177444595, -291.3053432458011116, -311.1203508074016213 ) ) ;
#59518 = CARTESIAN_POINT ( 'NONE',  ( 165.2494399300530290, -11.64849832608277325, -3.999999999999998224 ) ) ;
#59519 = CARTESIAN_POINT ( 'NONE',  ( -23.40286736638519471, -122.5496321078137356, 22.50000000000000000 ) ) ;
#59520 = CARTESIAN_POINT ( 'NONE',  ( 38.96342398434819643, -291.9956997548592881, -267.4822475280382719 ) ) ;
#59521 = CARTESIAN_POINT ( 'NONE',  ( 9.522980761087149304, -288.3094352266235774, -213.3511004577532617 ) ) ;
#59522 = CARTESIAN_POINT ( 'NONE',  ( -113.3764067926420012, -288.7814431443119361, -271.1949678090483076 ) ) ;
#59523 = CARTESIAN_POINT ( 'NONE',  ( 30.49797330927253114, -288.5962818300487811, -241.7133830080311441 ) ) ;
#59524 = FACE_OUTER_BOUND ( 'NONE', #58433, .T. ) ;
#59525 = CARTESIAN_POINT ( 'NONE',  ( 33.86059420307253731, -288.5763625844373337, -287.1788172759117401 ) ) ;
#59526 = CARTESIAN_POINT ( 'NONE',  ( 23.57190624233257736, -296.1338818609468717, -314.7443253490573625 ) ) ;
#59527 = DIRECTION ( 'NONE',  ( 0.000000000000000000, 1.000000000000000000, 0.000000000000000000 ) ) ;
#59528 = CARTESIAN_POINT ( 'NONE',  ( 25.53462351905800531, -289.3394627294273391, -314.2080938520719542 ) ) ;
#59529 = CARTESIAN_POINT ( 'NONE',  ( -12.03741097901147228, -278.3998112347296683, -199.3267510031387246 ) ) ;
#59530 = CARTESIAN_POINT ( 'NONE',  ( -113.0440607827452340, -278.7098822041110111, -284.3940660114665206 ) ) ;
#59531 = CARTESIAN_POINT ( 'NONE',  ( -25.39468663578752228, -279.8671760083025788, -194.3149927685418845 ) ) ;
#59532 = CARTESIAN_POINT ( 'NONE',  ( -63.68298239005284955, -299.6871102796877722, -200.4638615808408986 ) ) ;
#59533 = CARTESIAN_POINT ( 'NONE',  ( -52.46808131195603409, -283.8582324836573889, -196.9023320003765605 ) ) ;
#59534 = CARTESIAN_POINT ( 'NONE',  ( -4.999294894772630116, -278.6221756922370218, -203.5417023324997103 ) ) ;
#59535 = CARTESIAN_POINT ( 'NONE',  ( -65.84050210953581939, -281.4247720128125252, -339.7494210890263844 ) ) ;
#59536 = DIRECTION ( 'NONE',  ( 0.000000000000000000, -1.000000000000000000, 0.000000000000000000 ) ) ;
#59537 = CARTESIAN_POINT ( 'NONE',  ( -4.312632069130462931, -275.1045868853428829, -339.1634802805279492 ) ) ;
#59538 = CARTESIAN_POINT ( 'NONE',  ( -99.03854656822382196, -298.6266176146861540, -229.9672887946356923 ) ) ;
#59539 = CARTESIAN_POINT ( 'NONE',  ( -103.7658233028419943, -283.9740159266211208, -231.9237240757769882 ) ) ;
#59540 = CARTESIAN_POINT ( 'NONE',  ( -110.0365319254666474, -297.3712991017988543, -279.6475332947033507 ) ) ;
#59541 = CARTESIAN_POINT ( 'NONE',  ( -109.5510143678241661, -274.2948784320151958, -245.3726960788743554 ) ) ;
#59542 = CARTESIAN_POINT ( 'NONE',  ( 34.39506666860962270, -275.0390484499698118, -256.7257310647820532 ) ) ;
#59543 = CARTESIAN_POINT ( 'NONE',  ( 34.67764176685086142, -295.8223644810156543, -291.3409195127969724 ) ) ;
#59544 = CARTESIAN_POINT ( 'NONE',  ( -46.02366285445285854, -289.3259079535359319, -346.9232214442576492 ) ) ;
#59545 = CIRCLE ( 'NONE', #71653, 0.4999999999999947820 ) ;
#59546 = CARTESIAN_POINT ( 'NONE',  ( -45.10071797862819665, -278.0346057849507702, -195.1485453294131105 ) ) ;
#59547 = CARTESIAN_POINT ( 'NONE',  ( -112.2631837131080204, -290.1625297421371670, -288.1874955572000658 ) ) ;
#59548 = CARTESIAN_POINT ( 'NONE',  ( -95.14365093139960550, -288.9791361269830077, -315.3518507413093630 ) ) ;
#59549 = CARTESIAN_POINT ( 'NONE',  ( 20.67867814619486921, -290.8968325289162067, -222.8360050655022064 ) ) ;
#59550 = VERTEX_POINT ( 'NONE', #61611 ) ;
#59551 = FACE_BOUND ( 'NONE', #86222, .T. ) ;
#59552 = CIRCLE ( 'NONE', #42906, 11.68950434577434372 ) ;
#59553 = CARTESIAN_POINT ( 'NONE',  ( -90.79993995701471476, -290.7754789528456172, -220.5409652362462509 ) ) ;
#59554 = FACE_OUTER_BOUND ( 'NONE', #49675, .T. ) ;
#59555 = CARTESIAN_POINT ( 'NONE',  ( -70.97399007099811286, -286.5604040062812032, -201.3561233273001676 ) ) ;
#59556 = CARTESIAN_POINT ( 'NONE',  ( -37.30987171927208124, -291.5519495502701375, -340.3611179825599606 ) ) ;
#59557 = CARTESIAN_POINT ( 'NONE',  ( -24.95762099636236542, -293.9567857813126466, -346.1742066921028140 ) ) ;
#59558 = CARTESIAN_POINT ( 'NONE',  ( -4.361154404988054623, -283.9417094352826325, -339.4087101677097849 ) ) ;
#59559 = CARTESIAN_POINT ( 'NONE',  ( -42.67201101160323162, -285.8163836908742041, -197.5433566314246150 ) ) ;
#59560 = CIRCLE ( 'NONE', #79162, 4.999999999999985789 ) ;
#59561 = CARTESIAN_POINT ( 'NONE',  ( 19.57407412826109550, -277.5214164666213037, -316.8765257896781691 ) ) ;
#59562 = CARTESIAN_POINT ( 'NONE',  ( 5.467118782381859887, -290.6545251542821688, -209.1483195387613705 ) ) ;
#59563 = CARTESIAN_POINT ( 'NONE',  ( 29.45374299348132752, -273.9376712199444910, -239.8160946851348854 ) ) ;
#59564 = ORIENTED_EDGE ( 'NONE', *, *, #11999, .F. ) ;
#59565 = CARTESIAN_POINT ( 'NONE',  ( 64.33209501061345748, 48.33985520751024723, -319.1928417150128325 ) ) ;
#59566 = CARTESIAN_POINT ( 'NONE',  ( 38.58472444734961471, -293.3785646829250027, -283.1264778917486638 ) ) ;
#59567 = CARTESIAN_POINT ( 'NONE',  ( 9.926391277329841500, -288.6294093956313418, -212.8542337877264572 ) ) ;
#59568 = AXIS2_PLACEMENT_3D ( 'NONE', #80455, #39674, #46785 ) ;
#59569 = CARTESIAN_POINT ( 'NONE',  ( -111.6656575168238561, -297.3936883340443842, -289.3202284930042083 ) ) ;
#59570 = CARTESIAN_POINT ( 'NONE',  ( -27.83149326644779009, -286.8275296328849890, -197.8804403266230736 ) ) ;
#59571 = CARTESIAN_POINT ( 'NONE',  ( -97.75118954863651766, -276.9757929905859442, -317.7268630104115346 ) ) ;
#59572 = CARTESIAN_POINT ( 'NONE',  ( -37.80275380179691780, -292.6979288421708816, -193.4644326399993872 ) ) ;
#59573 = CARTESIAN_POINT ( 'NONE',  ( 37.86147189221529885, -285.8141243052073719, -279.9900887539664041 ) ) ;
#59574 = CARTESIAN_POINT ( 'NONE',  ( 35.43123181833192348, -293.5671761096620003, -245.1030844619403410 ) ) ;
#59575 = CARTESIAN_POINT ( 'NONE',  ( -92.57527218274242387, -291.5658159659975581, -222.5977428409451875 ) ) ;
#59576 = CARTESIAN_POINT ( 'NONE',  ( 175.2296996224750103, 275.5000000000000568, 0.000000000000000000 ) ) ;
#59577 = CARTESIAN_POINT ( 'NONE',  ( 6.586641810406439035, -59.71310429714220191, -351.1713004201388912 ) ) ;
#59578 = CARTESIAN_POINT ( 'NONE',  ( -52.05869819227491035, -287.3873292957083549, -195.4332025923267793 ) ) ;
#59579 = CARTESIAN_POINT ( 'NONE',  ( 40.64545035920995986, -279.2666405000204009, -288.1938231032136741 ) ) ;
#59580 = ORIENTED_EDGE ( 'NONE', *, *, #16109, .F. ) ;
#59581 = CARTESIAN_POINT ( 'NONE',  ( -32.13742060190021022, -281.9052862106516386, -343.4852695911754381 ) ) ;
#59582 = CARTESIAN_POINT ( 'NONE',  ( -112.4647011951343103, -278.0086935366750822, -287.1622787266808245 ) ) ;
#59583 = CARTESIAN_POINT ( 'NONE',  ( 37.25882013447047569, -283.6362855136566736, -276.8862712139290920 ) ) ;
#59584 = CARTESIAN_POINT ( 'NONE',  ( -104.8949806941793241, -262.6824176341613679, -316.8076958637401503 ) ) ;
#59585 = CARTESIAN_POINT ( 'NONE',  ( 17.39144175509819235, -280.8642827599528005, -323.7554559144114137 ) ) ;
#59586 = CARTESIAN_POINT ( 'NONE',  ( 36.62953843811489207, -285.4382983292776998, -259.9775103678533128 ) ) ;
#59587 = CARTESIAN_POINT ( 'NONE',  ( -13.47441790030156383, -276.2192317023518626, -198.4538282407935128 ) ) ;
#59588 = CONICAL_SURFACE ( 'NONE', #35382, 7.500000000000012434, 0.7853981633974513876 ) ;
#59589 = CARTESIAN_POINT ( 'NONE',  ( -106.7672262728909658, -297.3482445783442927, -247.4392095802336371 ) ) ;
#59590 = CARTESIAN_POINT ( 'NONE',  ( -45.15973353199539986, -293.8379123854019781, -343.4880732176315519 ) ) ;
#59591 = CARTESIAN_POINT ( 'NONE',  ( -96.97008280569878025, -278.5508914317156268, -318.9385967114022833 ) ) ;
#59592 = CARTESIAN_POINT ( 'NONE',  ( -53.95392964931998847, -277.2712698710034260, -341.4979535680965910 ) ) ;
#59593 = CARTESIAN_POINT ( 'NONE',  ( -30.52263579593893184, -299.0768152995971718, -193.5953506817569689 ) ) ;
#59594 = CARTESIAN_POINT ( 'NONE',  ( -93.11866633401946558, -276.7502436622364712, -323.0721407381615222 ) ) ;
#59595 = CARTESIAN_POINT ( 'NONE',  ( 64.47034098748159181, 48.08436262803363093, -318.7852478019347586 ) ) ;
#59596 = CARTESIAN_POINT ( 'NONE',  ( -100.5444961975137090, -276.0073132200173518, -310.8344157179166132 ) ) ;
#59597 = CARTESIAN_POINT ( 'NONE',  ( -69.26508263984791824, -296.8892132442754814, -339.7980859590122122 ) ) ;
#59598 = EDGE_CURVE ( 'NONE', #15079, #36764, #44108, .T. ) ;
#59599 = DIRECTION ( 'NONE',  ( 0.000000000000000000, 1.000000000000000000, 0.000000000000000000 ) ) ;
#59600 = CARTESIAN_POINT ( 'NONE',  ( 202.9738562182569694, 291.4636489450776367, -54.00000000000002132 ) ) ;
#59601 = CARTESIAN_POINT ( 'NONE',  ( -45.66094997524324839, -284.2396056453231381, -343.2478691523747898 ) ) ;
#59602 = CARTESIAN_POINT ( 'NONE',  ( -64.86398251714732055, -285.1668500991312385, -341.2023734020253301 ) ) ;
#59603 = CARTESIAN_POINT ( 'NONE',  ( -33.22463155806325119, -285.4538055576810507, -197.3253230840812478 ) ) ;
#59604 = CARTESIAN_POINT ( 'NONE',  ( -110.4109710795806762, -277.0918160819856553, -259.6475732372405787 ) ) ;
#59605 = CARTESIAN_POINT ( 'NONE',  ( -91.62885509584685906, -285.6964860873844145, -320.9948052486842016 ) ) ;
#59606 = CARTESIAN_POINT ( 'NONE',  ( -103.9886997496694789, -277.4543646077049175, -238.7946984259076828 ) ) ;
#59607 = CARTESIAN_POINT ( 'NONE',  ( -6.132596549257987917, -277.7117928338157640, -336.7090847301910799 ) ) ;
#59608 = CARTESIAN_POINT ( 'NONE',  ( 207.0561972617101674, 35.35788477359428583, 14.50000000000000000 ) ) ;
#59609 = CARTESIAN_POINT ( 'NONE',  ( -83.23410202314381934, -273.8959120811493335, -213.5115279246107605 ) ) ;
#59610 = CARTESIAN_POINT ( 'NONE',  ( 39.47876753147257745, -282.3135376910310583, -267.0541075799198438 ) ) ;
#59611 = CARTESIAN_POINT ( 'NONE',  ( 39.57885165322228715, -282.0031022786512267, -267.0537634741796182 ) ) ;
#59612 = ORIENTED_EDGE ( 'NONE', *, *, #30078, .T. ) ;
#59613 = ORIENTED_EDGE ( 'NONE', *, *, #76301, .F. ) ;
#59614 = CARTESIAN_POINT ( 'NONE',  ( 196.5975808051812237, 18.84406744235292663, -11.77299963048744047 ) ) ;
#59615 = CARTESIAN_POINT ( 'NONE',  ( 37.33530907281996747, -289.2489994240452233, -257.4923651067630885 ) ) ;
#59616 = CARTESIAN_POINT ( 'NONE',  ( -92.86028351398626057, -296.4263118160515660, -222.6943057946793090 ) ) ;
#59617 = ADVANCED_FACE ( 'NONE', ( #90443 ), #54483, .F. ) ;
#59618 = EDGE_CURVE ( 'NONE', #79037, #76858, #9183, .T. ) ;
#59619 = CARTESIAN_POINT ( 'NONE',  ( -5.920985965978887933, -291.8030217340574382, -200.1610121239084776 ) ) ;
#59620 = CARTESIAN_POINT ( 'NONE',  ( 32.96934510270195773, -286.3237795774564347, -292.6003530207044605 ) ) ;
#59622 = CARTESIAN_POINT ( 'NONE',  ( -14.51284509537617495, -290.5920326445378805, -199.9564491749622448 ) ) ;
#59621 = CARTESIAN_POINT ( 'NONE',  ( 12.54199498510939570, -286.9156327562212709, -324.5320253765555094 ) ) ;
#59623 = CARTESIAN_POINT ( 'NONE',  ( -17.07689196913042196, -287.5246230339130307, -199.7639001854538492 ) ) ;
#59624 = CARTESIAN_POINT ( 'NONE',  ( -91.89715655859116339, -275.8299030658744186, -321.9012202697894622 ) ) ;
#59625 = CARTESIAN_POINT ( 'NONE',  ( 25.18347967487245143, -286.5347114446096839, -314.0067314835784487 ) ) ;
#59626 = CIRCLE ( 'NONE', #55076, 204.9779373800640485 ) ;
#59627 = CARTESIAN_POINT ( 'NONE',  ( 4.054003918293396680, -288.6095584404092165, -207.7581160926768007 ) ) ;
#59628 = CARTESIAN_POINT ( 'NONE',  ( -94.09131169823331220, -287.8695570592416857, -319.6511779892436493 ) ) ;
#59629 = CARTESIAN_POINT ( 'NONE',  ( 33.55430200745949776, -282.7356276003422977, -288.7731642554599603 ) ) ;
#59630 = CARTESIAN_POINT ( 'NONE',  ( -108.6987472884038226, -292.8588280642905488, -246.5718007206116908 ) ) ;
#59631 = DIRECTION ( 'NONE',  ( -0.000000000000000000, -0.000000000000000000, -1.000000000000000000 ) ) ;
#59632 = DIRECTION ( 'NONE',  ( 1.000000000000000000, 0.000000000000000000, -0.000000000000000000 ) ) ;
#59633 = CIRCLE ( 'NONE', #68673, 1.000000000000000888 ) ;
#59634 = CARTESIAN_POINT ( 'NONE',  ( -35.88784722562734686, -299.9903649714495941, -194.8006387530634811 ) ) ;
#59635 = CARTESIAN_POINT ( 'NONE',  ( 26.60492476982885179, -280.2644164302735703, -234.8163449392670827 ) ) ;
#59636 = CARTESIAN_POINT ( 'NONE',  ( 20.88917038270630400, -280.2031966276928188, -317.6483226317695880 ) ) ;
#59637 = CARTESIAN_POINT ( 'NONE',  ( -11.12194061459957339, -293.9162530564656208, -342.6441745598965554 ) ) ;
#59638 = CARTESIAN_POINT ( 'NONE',  ( -110.1220644218794860, -270.9706115274059925, -256.6340620640322641 ) ) ;
#59639 = CARTESIAN_POINT ( 'NONE',  ( 30.45590196705300912, -274.0382778421782746, -301.0987064551663934 ) ) ;
#59640 = CARTESIAN_POINT ( 'NONE',  ( -69.92776676529885549, -296.8058422195309731, -336.2351776774651739 ) ) ;
#59641 = SURFACE_STYLE_FILL_AREA ( #32134 ) ;
#59642 = CARTESIAN_POINT ( 'NONE',  ( -92.73242993315990645, -271.8519894405659443, -217.7067427971994675 ) ) ;
#59644 = CARTESIAN_POINT ( 'NONE',  ( -106.2568930367351214, -294.3768824206371164, -302.3715881081471366 ) ) ;
#59643 = AXIS2_PLACEMENT_3D ( 'NONE', #49149, #78045, #65718 ) ;
#59645 = AXIS2_PLACEMENT_3D ( 'NONE', #64516, #13823, #28493 ) ;
#59646 = CARTESIAN_POINT ( 'NONE',  ( -17.28933198909028590, -293.7412133368897571, -199.5036038015535382 ) ) ;
#59647 = CARTESIAN_POINT ( 'NONE',  ( 175.2296996224750103, 250.5000000000000568, 0.000000000000000000 ) ) ;
#59648 = CARTESIAN_POINT ( 'NONE',  ( 25.93744072116606958, -294.8576357937615740, -307.0810316534348772 ) ) ;
#59649 = CARTESIAN_POINT ( 'NONE',  ( 129.4467878515196162, -293.3047352414760667, -195.3611179825600175 ) ) ;
#59651 = CARTESIAN_POINT ( 'NONE',  ( -108.4770382652945813, -296.7684173857288670, -253.9671048038309493 ) ) ;
#59650 = CARTESIAN_POINT ( 'NONE',  ( -59.99100360468393944, -283.7803175849629156, -198.4359083877053820 ) ) ;
#59652 = CIRCLE ( 'NONE', #18808, 7.999999999999998224 ) ;
#59653 = CARTESIAN_POINT ( 'NONE',  ( -113.9038621022054798, -284.4496033952801213, -278.5608346757138065 ) ) ;
#59654 = CARTESIAN_POINT ( 'NONE',  ( 21.73387225690156299, -282.8292874130477230, -223.2301447196631443 ) ) ;
#59655 = CARTESIAN_POINT ( 'NONE',  ( -71.05314149151706715, -285.2860771790552121, -201.1564720917731961 ) ) ;
#59656 = CARTESIAN_POINT ( 'NONE',  ( -105.7333461215181245, -288.1516246447949356, -300.8637023402644104 ) ) ;
#59657 = CARTESIAN_POINT ( 'NONE',  ( -110.4542110544635705, -270.2666405000204009, -253.6410175316879361 ) ) ;
#59658 = AXIS2_PLACEMENT_3D ( 'NONE', #46928, #46012, #75372 ) ;
#59659 = CARTESIAN_POINT ( 'NONE',  ( -5.570392078676166925, -285.1637882725778468, -204.0763753144603925 ) ) ;
#59660 = CARTESIAN_POINT ( 'NONE',  ( -113.5082482855353305, -289.3545551430068485, -279.7527184563340370 ) ) ;
#59661 = LINE ( 'NONE', #73841, #6786 ) ;
#59662 = CARTESIAN_POINT ( 'NONE',  ( -68.84047990809658302, -297.0733918637204169, -337.1152956874589108 ) ) ;
#59663 = CARTESIAN_POINT ( 'NONE',  ( -94.53291741035803852, -280.6692177007316218, -219.6879400736447394 ) ) ;
#59665 = CARTESIAN_POINT ( 'NONE',  ( 26.47937723959200085, -280.7338922373175478, -234.8793258868038265 ) ) ;
#59664 = CARTESIAN_POINT ( 'NONE',  ( 24.35321449964746421, -292.1571913053898584, -313.6519101550778714 ) ) ;
#59666 = CARTESIAN_POINT ( 'NONE',  ( -58.84928545343898065, -295.4894442195571287, -344.3519570706346826 ) ) ;
#59667 = CARTESIAN_POINT ( 'NONE',  ( -82.39725204952947024, -283.5227092671875084, -209.6385595715272814 ) ) ;
#59668 = CARTESIAN_POINT ( 'NONE',  ( -56.08218604468325452, -281.8110800861148846, -197.6866429753504804 ) ) ;
#59669 = CARTESIAN_POINT ( 'NONE',  ( -20.80666647776518019, -293.8935415776381319, -341.7576321749751855 ) ) ;
#59670 = CARTESIAN_POINT ( 'NONE',  ( -15.51135221623666283, -296.3252638725264774, -195.3685521545008896 ) ) ;
#59671 = ORIENTED_EDGE ( 'NONE', *, *, #39759, .F. ) ;
#59672 = DIRECTION ( 'NONE',  ( 0.000000000000000000, 1.000000000000000000, 0.000000000000000000 ) ) ;
#59673 = CARTESIAN_POINT ( 'NONE',  ( 31.52959223255893306, -283.1544049475468796, -241.5758459045207758 ) ) ;
#59674 = CARTESIAN_POINT ( 'NONE',  ( -70.96469589637160880, -295.0159718692639785, -335.2402254005137934 ) ) ;
#59675 = CARTESIAN_POINT ( 'NONE',  ( 164.2231345125756263, 264.6571197653884155, -7.500000000000000000 ) ) ;
#59676 = CARTESIAN_POINT ( 'NONE',  ( -85.33152481854864391, -275.1952119285918457, -330.4860931364850671 ) ) ;
#59677 = CARTESIAN_POINT ( 'NONE',  ( 24.35633267017240300, -274.1391117541636504, -224.5625200809061823 ) ) ;
#59678 = CARTESIAN_POINT ( 'NONE',  ( 39.14665404777217361, -288.8461503707620182, -268.6788733772784781 ) ) ;
#59679 = CARTESIAN_POINT ( 'NONE',  ( -108.9391484479606049, -290.1967658601028575, -284.6660408647016993 ) ) ;
#59680 = CARTESIAN_POINT ( 'NONE',  ( -34.30394467215880638, -281.6111237512004095, -196.7177564679887212 ) ) ;
#59681 = CARTESIAN_POINT ( 'NONE',  ( -87.89599776518949170, -274.9316707205931607, -216.5258683746128554 ) ) ;
#59682 = CARTESIAN_POINT ( 'NONE',  ( -95.91943023011107528, -277.9652002268731508, -226.1160595509714994 ) ) ;
#59683 = CARTESIAN_POINT ( 'NONE',  ( -54.38430306434025852, -279.2711085200696175, -343.4526894459543200 ) ) ;
#59684 = ORIENTED_EDGE ( 'NONE', *, *, #29223, .F. ) ;
#59685 = CARTESIAN_POINT ( 'NONE',  ( -29.83677167309599199, -273.9779991765897762, -193.7277306544036435 ) ) ;
#59686 = CARTESIAN_POINT ( 'NONE',  ( -67.16296899571523227, -293.5782509571520222, -202.1555014740926026 ) ) ;
#59687 = CARTESIAN_POINT ( 'NONE',  ( 208.4306832106271088, 1.000000000000000888, 0.000000000000000000 ) ) ;
#59688 = EDGE_CURVE ( 'NONE', #74706, #46033, #54957, .T. ) ;
#59689 = DIRECTION ( 'NONE',  ( -1.000000000000000000, 0.000000000000000000, 0.000000000000000000 ) ) ;
#59690 = CARTESIAN_POINT ( 'NONE',  ( 5.812442842206622551, -290.7699256440089357, -208.0873239530056651 ) ) ;
#59691 = CARTESIAN_POINT ( 'NONE',  ( -103.2579016783744379, -272.4856301571839481, -238.8485361360083914 ) ) ;
#59692 = DIRECTION ( 'NONE',  ( -1.000000000000000000, -0.000000000000000000, -0.000000000000000000 ) ) ;
#59693 = CARTESIAN_POINT ( 'NONE',  ( 3.751701049364114748, -294.1141798777090912, -206.0019945936297461 ) ) ;
#59694 = CARTESIAN_POINT ( 'NONE',  ( 35.59421657381088266, -301.4082689599840705, -190.3320873922940848 ) ) ;
#59695 = CARTESIAN_POINT ( 'NONE',  ( -22.11098025402440470, -288.2477330025578794, -197.0409362066403389 ) ) ;
#59696 = CARTESIAN_POINT ( 'NONE',  ( -35.08729803370692935, -275.0236121238818328, -345.1604903106862707 ) ) ;
#59697 = CARTESIAN_POINT ( 'NONE',  ( 37.08210012868024563, -277.4522209368880112, -268.8080081081959065 ) ) ;
#59698 = CARTESIAN_POINT ( 'NONE',  ( -63.28002308655479879, -289.7914272431645486, -200.5863546384857727 ) ) ;
#59699 = CARTESIAN_POINT ( 'NONE',  ( -61.67373556538015578, -281.5998601866348849, -198.5544220683409264 ) ) ;
#59700 = ORIENTED_EDGE ( 'NONE', *, *, #25372, .T. ) ;
#59701 = CARTESIAN_POINT ( 'NONE',  ( -45.65929330511178108, -282.5087999961667151, -343.0393846683190304 ) ) ;
#59702 = CARTESIAN_POINT ( 'NONE',  ( -62.29237663306363260, -278.4487675711058614, -342.9358578157461466 ) ) ;
#59703 = CARTESIAN_POINT ( 'NONE',  ( -34.50909818345874669, -281.8122183338728064, -346.9116574040626233 ) ) ;
#59704 = CIRCLE ( 'NONE', #39990, 1.000000000000000888 ) ;
#59705 = CARTESIAN_POINT ( 'NONE',  ( -31.45630831760752599, -277.9209374053632473, -346.9523442054671136 ) ) ;
#59706 = DIRECTION ( 'NONE',  ( 1.000000000000000000, 0.000000000000000000, 0.000000000000000000 ) ) ;
#59707 = CARTESIAN_POINT ( 'NONE',  ( 20.30925315795902364, -277.7540913384030432, -320.3716528631812821 ) ) ;
#59708 = CARTESIAN_POINT ( 'NONE',  ( -82.13390479932378696, -281.9090924074130839, -214.2458315076590907 ) ) ;
#59709 = ORIENTED_EDGE ( 'NONE', *, *, #82280, .F. ) ;
#59710 = CARTESIAN_POINT ( 'NONE',  ( -111.2509992310975235, -298.7159470469808866, -257.6168582356684169 ) ) ;
#59711 = CARTESIAN_POINT ( 'NONE',  ( -18.38034989409230846, -289.8818603630846837, -341.2284281143449789 ) ) ;
#59712 = CARTESIAN_POINT ( 'NONE',  ( -37.84561078348364305, -275.0785680327639966, -345.0169544141380129 ) ) ;
#59713 = CARTESIAN_POINT ( 'NONE',  ( -29.06498055141730674, -290.7089034677928794, -345.9485017376171641 ) ) ;
#59714 = CARTESIAN_POINT ( 'NONE',  ( -2.383402299832444449, -291.8762109097629605, -206.1455775915851802 ) ) ;
#59715 = CARTESIAN_POINT ( 'NONE',  ( 24.08928756656527881, -287.6771396316802907, -316.6834738628915034 ) ) ;
#59716 = DIRECTION ( 'NONE',  ( 0.9452808130703184153, -0.000000000000000000, -0.3262578496237564796 ) ) ;
#59717 = CARTESIAN_POINT ( 'NONE',  ( -89.47368205301026478, -282.2011493925952550, -322.6697982116314165 ) ) ;
#59718 = CARTESIAN_POINT ( 'NONE',  ( -109.5464092174098596, -292.1888584972708713, -287.6048260822874454 ) ) ;
#59719 = CARTESIAN_POINT ( 'NONE',  ( -106.2060208455930876, -283.3790556268481282, -244.1234907382296058 ) ) ;
#59720 = CARTESIAN_POINT ( 'NONE',  ( 17.41916186665769573, -282.1707439834014508, -221.3459012405685655 ) ) ;
#59721 = CARTESIAN_POINT ( 'NONE',  ( 14.45381702192093343, -289.2862508021310646, -327.0904162859282565 ) ) ;
#59722 = CARTESIAN_POINT ( 'NONE',  ( -110.3413688935416701, -279.0048800858978097, -273.3672453267885203 ) ) ;
#59723 = CARTESIAN_POINT ( 'NONE',  ( 21.01795744746100780, -291.6744495375634187, -220.7209254567658263 ) ) ;
#59724 = AXIS2_PLACEMENT_3D ( 'NONE', #48617, #78915, #6022 ) ;
#59725 = CARTESIAN_POINT ( 'NONE',  ( -26.65370208993070733, -286.9875079116935694, -194.2161716983249278 ) ) ;
#59726 = CARTESIAN_POINT ( 'NONE',  ( 25.80479491593573371, -288.6268492442459319, -314.4076601279724628 ) ) ;
#59727 = CARTESIAN_POINT ( 'NONE',  ( -64.05339574406613679, -283.5772309151163881, -338.2984812065489564 ) ) ;
#59728 = ORIENTED_EDGE ( 'NONE', *, *, #63164, .T. ) ;
#59729 = CARTESIAN_POINT ( 'NONE',  ( 184.7149167944524493, 8.542400036368780647, 13.00000000000000178 ) ) ;
#59730 = CARTESIAN_POINT ( 'NONE',  ( -55.90938056640048615, -293.6761043470941672, -196.8526613169327391 ) ) ;
#59731 = CARTESIAN_POINT ( 'NONE',  ( 37.58421457211225913, -292.4317391272521718, -285.8338546751198237 ) ) ;
#59732 = CARTESIAN_POINT ( 'NONE',  ( -68.14727241555689830, -276.5256521572768520, -336.8160517478360134 ) ) ;
#59733 = CARTESIAN_POINT ( 'NONE',  ( -34.75535411046524104, -297.4323273630881204, -193.4633272928202246 ) ) ;
#59734 = CARTESIAN_POINT ( 'NONE',  ( 9.302512522018274055, -291.1860493713606957, -213.2420877315347809 ) ) ;
#59735 = CARTESIAN_POINT ( 'NONE',  ( -86.76047310469942886, -295.5934035755619789, -215.2633967151891454 ) ) ;
#59736 = CARTESIAN_POINT ( 'NONE',  ( -36.21534744610778489, -293.2716266669405059, -196.9601422330328262 ) ) ;
#59737 = CARTESIAN_POINT ( 'NONE',  ( 33.74917465839161679, -294.8670318935711521, -288.2584249475976321 ) ) ;
#59738 = FACE_OUTER_BOUND ( 'NONE', #16552, .T. ) ;
#59739 = CARTESIAN_POINT ( 'NONE',  ( 30.56262401808909601, -291.9765684392257299, -302.7163727456934339 ) ) ;
#59740 = CARTESIAN_POINT ( 'NONE',  ( -90.66203747850281047, -299.2970177042143973, -217.5448304489311226 ) ) ;
#59741 = CARTESIAN_POINT ( 'NONE',  ( 33.61355940060740721, -288.2542460067980414, -252.1788055280051992 ) ) ;
#59742 = CARTESIAN_POINT ( 'NONE',  ( 26.27410627145429345, -278.0740542999984086, -310.8492002204433788 ) ) ;
#59743 = CARTESIAN_POINT ( 'NONE',  ( -48.03319200387923615, -278.6038275693235846, -194.5514960662683279 ) ) ;
#59744 = ADVANCED_FACE ( 'NONE', ( #46436 ), #55442, .T. ) ;
#59745 = CARTESIAN_POINT ( 'NONE',  ( -58.08613152476248587, -273.1396816699996180, -196.2586118664796686 ) ) ;
#59746 = CARTESIAN_POINT ( 'NONE',  ( 22.14621409499660487, -280.2484827093200579, -315.1315004234939465 ) ) ;
#59747 = CARTESIAN_POINT ( 'NONE',  ( -56.33732028574098649, -278.2113705855249464, -196.5123383668334611 ) ) ;
#59748 = EDGE_CURVE ( 'NONE', #33611, #82501, #4861, .T. ) ;
#59749 = CARTESIAN_POINT ( 'NONE',  ( -105.4250072226659256, -294.8687517528945818, -298.0361387046005461 ) ) ;
#59750 = CARTESIAN_POINT ( 'NONE',  ( -36.09237171215955442, -122.5496321078137356, -21.50000000000000000 ) ) ;
#59751 = CARTESIAN_POINT ( 'NONE',  ( 21.55839628155816001, -275.5977646934261998, -227.0636433290985678 ) ) ;
#59752 = CARTESIAN_POINT ( 'NONE',  ( 208.6208076322478746, 32.98517505407394168, 10.00000000000000000 ) ) ;
#59753 = CARTESIAN_POINT ( 'NONE',  ( -110.3936965504984897, -288.8092463544043653, -251.8210390098774667 ) ) ;
#59754 = CARTESIAN_POINT ( 'NONE',  ( -87.38443519962841322, -289.7274506397511118, -328.9522982916945466 ) ) ;
#59755 = CARTESIAN_POINT ( 'NONE',  ( -35.59260432212233383, -276.0741778146834235, -195.2019822268128451 ) ) ;
#59756 = CARTESIAN_POINT ( 'NONE',  ( -111.0780818667128642, -294.7162722516676467, -257.5949738405867038 ) ) ;
#59757 = CARTESIAN_POINT ( 'NONE',  ( 2.002657579084959671, -281.7366859000046020, -336.3624841579058398 ) ) ;
#59758 = DIRECTION ( 'NONE',  ( 0.000000000000000000, 0.000000000000000000, -1.000000000000000000 ) ) ;
#59759 = CARTESIAN_POINT ( 'NONE',  ( 34.57257919619672037, -279.8267546078670875, -291.6975797765239804 ) ) ;
#59760 = CARTESIAN_POINT ( 'NONE',  ( 175.2296996224750103, 134.0000000000000284, 0.000000000000000000 ) ) ;
#59761 = CARTESIAN_POINT ( 'NONE',  ( -105.4873961128336219, -288.9825365149166601, -297.7610262616169621 ) ) ;
#59762 = CARTESIAN_POINT ( 'NONE',  ( -72.00631184373531823, -281.6552263192173200, -336.0058449377789316 ) ) ;
#59763 = CARTESIAN_POINT ( 'NONE',  ( 175.2296996224750103, 249.5000000000000568, 0.000000000000000000 ) ) ;
#59764 = CARTESIAN_POINT ( 'NONE',  ( 221.8344101925596306, 1.000000000000000000, 10.00000000000000000 ) ) ;
#59765 = CARTESIAN_POINT ( 'NONE',  ( 10.13402971821695076, -290.7060881081154662, -212.2329443478662370 ) ) ;
#59766 = CARTESIAN_POINT ( 'NONE',  ( -73.21322283195371483, -279.1362628165799151, -334.8711922747243648 ) ) ;
#59767 = CARTESIAN_POINT ( 'NONE',  ( -78.93120839027876912, -284.8046296929813366, -334.6909051766065772 ) ) ;
#59769 = CARTESIAN_POINT ( 'NONE',  ( -41.32292902932859135, -286.0006676799977186, -197.4572633832124495 ) ) ;
#59768 = CARTESIAN_POINT ( 'NONE',  ( 24.97114220135220464, -273.0570098735959732, -227.6014939173690550 ) ) ;
#59770 = CARTESIAN_POINT ( 'NONE',  ( 10.05731441514111957, -277.8089130592833840, -326.6523991530547733 ) ) ;
#59771 = CARTESIAN_POINT ( 'NONE',  ( 22.60400914789265769, -276.9396298768385236, -312.3898986367362909 ) ) ;
#59772 = CARTESIAN_POINT ( 'NONE',  ( -110.4169716308812070, -286.7690747041713166, -253.4790165613358113 ) ) ;
#59773 = ORIENTED_EDGE ( 'NONE', *, *, #78743, .T. ) ;
#59774 = CARTESIAN_POINT ( 'NONE',  ( 73.43068321062709458, -134.2391364535880598, 0.000000000000000000 ) ) ;
#59775 = CARTESIAN_POINT ( 'NONE',  ( -111.5925811222122945, -296.1300434154398431, -290.7524562445588003 ) ) ;
#59776 = CARTESIAN_POINT ( 'NONE',  ( -7.622748016606969657, -288.4235515614760743, -201.8875413966727024 ) ) ;
#59777 = CARTESIAN_POINT ( 'NONE',  ( 160.5350683151633291, 250.5000000000000568, 25.22542485937379553 ) ) ;
#59778 = CARTESIAN_POINT ( 'NONE',  ( 25.18497378105905682, -285.6952119285918457, -320.2651865833026363 ) ) ;
#59779 = CARTESIAN_POINT ( 'NONE',  ( -90.83267612166100946, -278.2353242451486039, -215.3306785861155390 ) ) ;
#59780 = CARTESIAN_POINT ( 'NONE',  ( -85.98650101412113145, -289.7912209694848116, -211.6400533138141782 ) ) ;
#59781 = CARTESIAN_POINT ( 'NONE',  ( -110.1088070768855403, -286.2255244645986636, -258.6339156118998517 ) ) ;
#59782 = AXIS2_PLACEMENT_3D ( 'NONE', #76115, #82278, #68547 ) ;
#59783 = CARTESIAN_POINT ( 'NONE',  ( -111.1775206948295249, -280.2365831447859250, -276.1805726540234787 ) ) ;
#59784 = CARTESIAN_POINT ( 'NONE',  ( 38.20027581120578475, -288.8315202155641828, -258.7843080269046823 ) ) ;
#59785 = CARTESIAN_POINT ( 'NONE',  ( -20.92632432880489191, -284.8417872597761971, -343.5960877921627912 ) ) ;
#59786 = CARTESIAN_POINT ( 'NONE',  ( 3.503300492076803607, -276.6860664231760438, -335.6978129411951954 ) ) ;
#59787 = CARTESIAN_POINT ( 'NONE',  ( -69.95388855377572668, -295.6405455579798627, -203.2173023830663965 ) ) ;
#59788 = CARTESIAN_POINT ( 'NONE',  ( -79.90901449609418705, -279.3272215037501951, -206.1331212874697769 ) ) ;
#59789 = CARTESIAN_POINT ( 'NONE',  ( -105.0381334677153546, -298.8832036626652098, -239.2771928253048657 ) ) ;
#59790 = CARTESIAN_POINT ( 'NONE',  ( 156.3984609948130071, 15.95758591462568710, 7.138650918358441899 ) ) ;
#59791 = CARTESIAN_POINT ( 'NONE',  ( -69.91165696735023971, -276.1233781216988064, -202.8022627189028810 ) ) ;
#59792 = CARTESIAN_POINT ( 'NONE',  ( -85.15302759674364097, -271.6420913858016206, -211.3013941687038084 ) ) ;
#59793 = DIRECTION ( 'NONE',  ( -0.000000000000000000, 1.000000000000000000, -0.000000000000000000 ) ) ;
#59794 = CARTESIAN_POINT ( 'NONE',  ( -48.62352373873373068, -276.7071936022409773, -342.5977910885592905 ) ) ;
#59795 = CARTESIAN_POINT ( 'NONE',  ( -73.76964031996159576, -274.7849751319397456, -202.9151006532376016 ) ) ;
#59796 = CARTESIAN_POINT ( 'NONE',  ( -8.139531221201190547, -281.7378022744816235, -341.4108144909678799 ) ) ;
#59797 = CARTESIAN_POINT ( 'NONE',  ( 22.79798817802251065, -289.9070913852672788, -313.5026513959310250 ) ) ;
#59798 = CARTESIAN_POINT ( 'NONE',  ( -97.69758570922418528, -298.7014313077266934, -223.6508929627860596 ) ) ;
#59799 = CARTESIAN_POINT ( 'NONE',  ( -51.74110041214319011, -299.0770784330292713, -195.0696592759014436 ) ) ;
#59800 = CARTESIAN_POINT ( 'NONE',  ( -58.18952085651297779, -293.7824356915734825, -198.4362126842878808 ) ) ;
#59801 = CARTESIAN_POINT ( 'NONE',  ( 32.02462957728457837, -279.9187893120579815, -298.4385239749499306 ) ) ;
#59802 = CARTESIAN_POINT ( 'NONE',  ( 27.70551190340293957, -282.9869646775324554, -234.1647866440740415 ) ) ;
#59803 = CARTESIAN_POINT ( 'NONE',  ( -97.59444279829156699, -271.1767109208637407, -226.2133471507214040 ) ) ;
#59804 = CARTESIAN_POINT ( 'NONE',  ( -94.71878262826569994, -285.4669500191061502, -320.5040219714072123 ) ) ;
#59805 = CARTESIAN_POINT ( 'NONE',  ( 14.29138804546174057, -287.2255620141465897, -322.4019700025412476 ) ) ;
#59806 = CARTESIAN_POINT ( 'NONE',  ( 66.25670972154831873, 47.06390698321332167, -318.7317394719314620 ) ) ;
#59807 = VERTEX_POINT ( 'NONE', #76279 ) ;
#59808 = CARTESIAN_POINT ( 'NONE',  ( 7.573381283506060768, -287.0277106130403695, -332.2425486772297063 ) ) ;
#59809 = CARTESIAN_POINT ( 'NONE',  ( 19.52728127439686645, -287.8662783969826364, -316.1651182568014633 ) ) ;
#59810 = ORIENTED_EDGE ( 'NONE', *, *, #75831, .T. ) ;
#59811 = CARTESIAN_POINT ( 'NONE',  ( -101.1542674085729345, -285.0685943038000119, -312.9939953919073332 ) ) ;
#59812 = CARTESIAN_POINT ( 'NONE',  ( -4.098849446580143940, -274.8363442099954455, -205.3316957875819355 ) ) ;
#59813 = CARTESIAN_POINT ( 'NONE',  ( -105.7222414134044612, -289.9226437226115536, -235.5224008523209136 ) ) ;
#59814 = CARTESIAN_POINT ( 'NONE',  ( 37.76776037595595170, -282.4108126385665400, -286.9107941091407952 ) ) ;
#59815 = CARTESIAN_POINT ( 'NONE',  ( 38.92742961939502067, -283.1024758045021485, -272.7543581536374973 ) ) ;
#59816 = CARTESIAN_POINT ( 'NONE',  ( -71.72548637421012074, -283.8273894029236999, -339.2341862678035795 ) ) ;
#59817 = CARTESIAN_POINT ( 'NONE',  ( -85.48418169845588466, -279.3641122505070484, -215.4857913935897500 ) ) ;
#59818 = CARTESIAN_POINT ( 'NONE',  ( -54.42813229853333468, -271.3380690714489560, -195.3538533559490702 ) ) ;
#59819 = CARTESIAN_POINT ( 'NONE',  ( 168.5485566325764069, 232.3890912981213717, -192.7980796144592546 ) ) ;
#59820 = ORIENTED_EDGE ( 'NONE', *, *, #48813, .F. ) ;
#59821 = CARTESIAN_POINT ( 'NONE',  ( 36.42875546167547185, -277.3896077738209556, -257.7174078676169984 ) ) ;
#59822 = CARTESIAN_POINT ( 'NONE',  ( 167.0956850759771157, 232.7156327414166697, -192.3491569821647147 ) ) ;
#59823 = CARTESIAN_POINT ( 'NONE',  ( -35.13557503043015373, -297.4290726340713036, -197.2594361228370872 ) ) ;
#59824 = CARTESIAN_POINT ( 'NONE',  ( 23.06366043742156791, -292.4217407343726336, -222.6879977926365370 ) ) ;
#59825 = CARTESIAN_POINT ( 'NONE',  ( 197.1939414079961068, 281.6276418469664122, -110.3312364695952255 ) ) ;
#59827 = CARTESIAN_POINT ( 'NONE',  ( -15.63559332744059560, -287.1665590860283714, -340.9502193199492126 ) ) ;
#59826 = CARTESIAN_POINT ( 'NONE',  ( -110.5602435304467832, -271.5193695338213047, -247.9913494692551978 ) ) ;
#59828 = CARTESIAN_POINT ( 'NONE',  ( -20.54606043807000759, -296.6947587259135162, -342.7243565857409635 ) ) ;
#59829 = CARTESIAN_POINT ( 'NONE',  ( -62.74897468898124941, -287.0297092932822238, -201.3451565021675549 ) ) ;
#59830 = ORIENTED_EDGE ( 'NONE', *, *, #69090, .F. ) ;
#59831 = CARTESIAN_POINT ( 'NONE',  ( -32.01682861958862247, -295.9277974261654549, -346.9541332634416904 ) ) ;
#59832 = CARTESIAN_POINT ( 'NONE',  ( -103.5438792155005814, -285.4629318991974287, -239.3338853962637529 ) ) ;
#59833 = CARTESIAN_POINT ( 'NONE',  ( 53.02061087099094294, -297.9547193582686191, -193.7761767739849859 ) ) ;
#59834 = CARTESIAN_POINT ( 'NONE',  ( -44.89137728774763758, -292.7618475729618126, -193.8415738790481555 ) ) ;
#59835 = CARTESIAN_POINT ( 'NONE',  ( 35.43025780430517813, -294.3613555150514003, -295.4997882179580984 ) ) ;
#59836 = CARTESIAN_POINT ( 'NONE',  ( -69.01952119185894219, -291.7903132264139003, -204.5786621262338940 ) ) ;
#59837 = ORIENTED_EDGE ( 'NONE', *, *, #38620, .F. ) ;
#59838 = CARTESIAN_POINT ( 'NONE',  ( 0.000000000000000000, 0.000000000000000000, -40.00000000000000711 ) ) ;
#59839 = CARTESIAN_POINT ( 'NONE',  ( -112.4343469585250119, -274.5792469029044582, -261.9701353890976634 ) ) ;
#59840 = CARTESIAN_POINT ( 'NONE',  ( 11.54415370207408564, -273.5076165051057160, -211.3160649113189038 ) ) ;
#59841 = ORIENTED_EDGE ( 'NONE', *, *, #80919, .F. ) ;
#59842 = VERTEX_POINT ( 'NONE', #61157 ) ;
#59843 = CARTESIAN_POINT ( 'NONE',  ( 23.46555241426075611, -275.6899676316126033, -317.5206302212818059 ) ) ;
#59844 = CARTESIAN_POINT ( 'NONE',  ( -98.49479361424627655, -271.5211272808954277, -228.9572805244135623 ) ) ;
#59845 = CARTESIAN_POINT ( 'NONE',  ( -94.04883340816303416, -281.0822238220499116, -222.4336601087031511 ) ) ;
#59846 = CARTESIAN_POINT ( 'NONE',  ( -4.541289912399062878, -274.7549574148200122, -336.9710266119130324 ) ) ;
#59847 = CARTESIAN_POINT ( 'NONE',  ( -106.1835776299343905, -298.0965403650738494, -244.7600371908943657 ) ) ;
#59848 = CARTESIAN_POINT ( 'NONE',  ( -78.99872674225353819, -274.4166242656008308, -210.0657947924567281 ) ) ;
#59849 = CARTESIAN_POINT ( 'NONE',  ( -92.45286756839716702, -275.0368891145354837, -218.0283277660527119 ) ) ;
#59850 = CARTESIAN_POINT ( 'NONE',  ( -60.34452159860159526, -271.7755938740722854, -198.5482201839979552 ) ) ;
#59851 = CARTESIAN_POINT ( 'NONE',  ( 17.16209751502314518, -294.8996385466196557, -319.0957885185661667 ) ) ;
#59852 = CARTESIAN_POINT ( 'NONE',  ( -69.25685667554330394, -290.1986187309854586, -204.0388515191822592 ) ) ;
#59853 = CYLINDRICAL_SURFACE ( 'NONE', #35205, 1.895975569037589015 ) ;
#59854 = CARTESIAN_POINT ( 'NONE',  ( -14.60189432618421179, -277.2575962254414321, -343.9181122100008565 ) ) ;
#59855 = CARTESIAN_POINT ( 'NONE',  ( -35.39245437488732904, -274.2439415676043950, -197.3746416265469463 ) ) ;
#59856 = AXIS2_PLACEMENT_3D ( 'NONE', #66573, #74125, #7404 ) ;
#59857 = CARTESIAN_POINT ( 'NONE',  ( -106.5665948135525980, -282.8170347997694876, -302.9373704866046069 ) ) ;
#59858 = CARTESIAN_POINT ( 'NONE',  ( -30.72631281538588510, -296.9688542096346282, -345.2361143240630099 ) ) ;
#59859 = CARTESIAN_POINT ( 'NONE',  ( 154.1415209985679269, 20.37991841447901820, -11.45812909362559040 ) ) ;
#59860 = CARTESIAN_POINT ( 'NONE',  ( 9.140943131670363542, -285.9068609658804689, -213.8636348349867262 ) ) ;
#59861 = CARTESIAN_POINT ( 'NONE',  ( -30.40993362373118103, -280.9644985858088262, -345.2074875628674135 ) ) ;
#59862 = CARTESIAN_POINT ( 'NONE',  ( -43.31085443167592786, -275.3684220568890737, -344.1333567353430567 ) ) ;
#59863 = CARTESIAN_POINT ( 'NONE',  ( 30.81697159432768274, -274.4971626236555835, -298.2413610292055637 ) ) ;
#59864 = CARTESIAN_POINT ( 'NONE',  ( 36.02782401972909554, -283.3518243804489316, -254.7468375708408814 ) ) ;
#59865 = CARTESIAN_POINT ( 'NONE',  ( 24.11765056412005848, -276.2042337513098573, -230.2378240344406493 ) ) ;
#59866 = CARTESIAN_POINT ( 'NONE',  ( 197.2116943569230045, 215.0000000000000568, -12.92446933126075592 ) ) ;
#59867 = B_SPLINE_CURVE_WITH_KNOTS ( 'NONE', 3,
 ( #25449, #39169, #32090, #68081, #61467, #83202, #31177, #45816 ),
 .UNSPECIFIED., .F., .F.,
 ( 4, 2, 2, 4 ),
 ( -8.944277078438763205E-06, 0.001321608365870415719, 0.001986884687344899272, 0.002652161008819382826 ),
 .UNSPECIFIED. ) ;
#59868 = CARTESIAN_POINT ( 'NONE',  ( -18.72548618634065321, -272.6877316019501336, -196.4156757316058020 ) ) ;
#59869 = CARTESIAN_POINT ( 'NONE',  ( -31.24839846841152280, -282.1289783530559134, -195.3903910776010662 ) ) ;
#59870 = CARTESIAN_POINT ( 'NONE',  ( 157.4851178187871312, 17.34719063663031946, -6.999999999999998224 ) ) ;
#59871 = CARTESIAN_POINT ( 'NONE',  ( -2.901492816105845751, -288.4237949380349164, -203.0920053168421475 ) ) ;
#59872 = CARTESIAN_POINT ( 'NONE',  ( 156.0793278192200830, 19.12150670425148036, -12.12861874973244269 ) ) ;
#59873 = CARTESIAN_POINT ( 'NONE',  ( -62.51885965831366576, -287.3794356077967791, -341.0632713737886093 ) ) ;
#59874 = CARTESIAN_POINT ( 'NONE',  ( 82.12341071034305173, -301.5530703083973094, -195.5810619036753621 ) ) ;
#59875 = CARTESIAN_POINT ( 'NONE',  ( -110.8342274447078353, -271.2731220238221681, -267.6021512995649800 ) ) ;
#59876 = CARTESIAN_POINT ( 'NONE',  ( -96.07740985483196994, -289.3203087400980280, -224.9630796293529613 ) ) ;
#59877 = CARTESIAN_POINT ( 'NONE',  ( -112.8394912670188432, -266.8193566212495966, -283.2716462811306428 ) ) ;
#59878 = DIRECTION ( 'NONE',  ( -0.8660254037844404840, 0.000000000000000000, -0.4999999999999968359 ) ) ;
#59879 = CARTESIAN_POINT ( 'NONE',  ( 23.57690612498094040, -286.6495310681497131, -316.3136061280771401 ) ) ;
#59880 = CARTESIAN_POINT ( 'NONE',  ( -4.452535808313517585, -284.2113900780484528, -336.4273218072285090 ) ) ;
#59881 = CARTESIAN_POINT ( 'NONE',  ( -107.3030483509968604, -282.4079987788808808, -300.1502239984573066 ) ) ;
#59882 = CARTESIAN_POINT ( 'NONE',  ( -70.22071680094495605, -291.6062597767686952, -205.1846631646922390 ) ) ;
#59883 = CARTESIAN_POINT ( 'NONE',  ( 20.65648588179590917, -283.6107212219213238, -315.6555474253764260 ) ) ;
#59884 = CARTESIAN_POINT ( 'NONE',  ( -7.177580718275951455, -283.4488846991008018, -337.0286522395519455 ) ) ;
#59885 = CARTESIAN_POINT ( 'NONE',  ( -54.11052887803349165, -291.2461902545247199, -343.8803853110682667 ) ) ;
#59886 = CARTESIAN_POINT ( 'NONE',  ( -96.92240829427498738, -273.5402224874503077, -221.5975117940554640 ) ) ;
#59887 = CARTESIAN_POINT ( 'NONE',  ( -3.723798878786034994, -286.6919988280857865, -338.0448949012799744 ) ) ;
#59888 = CARTESIAN_POINT ( 'NONE',  ( 36.06263233575805316, -275.8444448026766622, -293.6163104250691163 ) ) ;
#59889 = CARTESIAN_POINT ( 'NONE',  ( -87.04257176165499743, -293.3364210459879473, -214.5988856252446340 ) ) ;
#59890 = DIRECTION ( 'NONE',  ( -0.000000000000000000, 1.000000000000000000, -0.000000000000000000 ) ) ;
#59891 = CARTESIAN_POINT ( 'NONE',  ( 35.77081079830085031, -277.8376638359845288, -253.6410175316879361 ) ) ;
#59892 = CARTESIAN_POINT ( 'NONE',  ( -48.25363108850776683, -275.1904010751892429, -344.7841434390111317 ) ) ;
#59893 = DIRECTION ( 'NONE',  ( -0.000000000000000000, -1.000000000000000000, -0.000000000000000000 ) ) ;
#59894 = CARTESIAN_POINT ( 'NONE',  ( -98.43866940082922667, -295.5643255791685533, -224.8025413472602168 ) ) ;
#59895 = CARTESIAN_POINT ( 'NONE',  ( -55.22572924904498137, -293.4183893965025050, -198.7608252775363837 ) ) ;
#59896 = CARTESIAN_POINT ( 'NONE',  ( -85.37089824739111066, -272.7164044348450034, -215.1838689634349748 ) ) ;
#59897 = CARTESIAN_POINT ( 'NONE',  ( -111.0618844352059540, -292.0970852283807631, -268.4630347558305061 ) ) ;
#59898 = CARTESIAN_POINT ( 'NONE',  ( -22.70528133408100757, -293.1853659735446058, -198.6033052213029180 ) ) ;
#59899 = CARTESIAN_POINT ( 'NONE',  ( -101.8858418863424617, -286.8023473990782577, -234.0341057589306502 ) ) ;
#59900 = CARTESIAN_POINT ( 'NONE',  ( 27.54234683659478478, -294.4442714519171886, -229.9044345564421121 ) ) ;
#59901 = CARTESIAN_POINT ( 'NONE',  ( 24.49762168190883571, -295.4692711078989191, -315.4297960445541094 ) ) ;
#59902 = CARTESIAN_POINT ( 'NONE',  ( -13.01024369078865384, -294.5604493792727112, -339.2400989432494498 ) ) ;
#59903 = CARTESIAN_POINT ( 'NONE',  ( 14.50420669101167093, -288.7812082875682904, -216.0953726551335023 ) ) ;
#59904 = CARTESIAN_POINT ( 'NONE',  ( 0.8702025466675872289, -282.7237271127066833, -337.2258118303606125 ) ) ;
#59905 = CARTESIAN_POINT ( 'NONE',  ( 73.76994744378262681, -297.5125299601920119, -194.8371112144576216 ) ) ;
#59906 = CARTESIAN_POINT ( 'NONE',  ( -46.50339244953634221, -285.7722435388460553, -193.9081036645936820 ) ) ;
#59907 = CARTESIAN_POINT ( 'NONE',  ( 26.80156856705642809, -278.0453233320057507, -308.5381776122274573 ) ) ;
#59908 = CARTESIAN_POINT ( 'NONE',  ( -96.88802799567245927, -283.9441705592350900, -227.4285498773733707 ) ) ;
#59909 = CARTESIAN_POINT ( 'NONE',  ( 35.77570596229903543, -285.3369260600396728, -253.6053634102506464 ) ) ;
#59910 = CARTESIAN_POINT ( 'NONE',  ( -28.34773591233913592, -278.3045522671701519, -195.0792745551300129 ) ) ;
#59911 = DIRECTION ( 'NONE',  ( 0.000000000000000000, 1.000000000000000000, 0.000000000000000000 ) ) ;
#59912 = CARTESIAN_POINT ( 'NONE',  ( -66.58996174927615641, -282.9535259265710465, -337.3263824336396510 ) ) ;
#59913 = CARTESIAN_POINT ( 'NONE',  ( -77.29856545092492581, -280.7343952382271368, -204.9433145908795950 ) ) ;
#59914 = CARTESIAN_POINT ( 'NONE',  ( 29.93115793733951335, -286.1293350021964557, -233.2753574517882100 ) ) ;
#59915 = CARTESIAN_POINT ( 'NONE',  ( 25.29665154043909325, -295.8505621639567380, -309.8834532017362449 ) ) ;
#59916 = CARTESIAN_POINT ( 'NONE',  ( -77.37706367951381026, -279.1793560791526261, -335.2576795012071784 ) ) ;
#59917 = EDGE_CURVE ( 'NONE', #75628, #89903, #11870, .T. ) ;
#59918 = CARTESIAN_POINT ( 'NONE',  ( -12.01354245582624714, -278.0445835991639001, -342.6093692790500427 ) ) ;
#59920 = EDGE_CURVE ( 'NONE', #70318, #81225, #69878, .T. ) ;
#59919 = CARTESIAN_POINT ( 'NONE',  ( -109.2864456931788055, -278.2213494960535058, -282.8024568442604618 ) ) ;
#59921 = CARTESIAN_POINT ( 'NONE',  ( -95.90150665561472465, -299.1941044623279709, -223.7695147596665493 ) ) ;
#59922 = CARTESIAN_POINT ( 'NONE',  ( 37.38498537389749288, -285.4893312287964022, -265.4921790455068162 ) ) ;
#59923 = COLOUR_RGB ( '',0.7921568627450980005, 0.8196078431372548767, 0.9333333333333333481 ) ;
#59924 = CARTESIAN_POINT ( 'NONE',  ( -99.20870705545418389, -291.5561715330583183, -314.8684501775746867 ) ) ;
#59925 = CARTESIAN_POINT ( 'NONE',  ( -47.85088403527714007, -294.1091254032806432, -342.9645502403151340 ) ) ;
#59926 = ORIENTED_EDGE ( 'NONE', *, *, #5542, .T. ) ;
#59927 = CARTESIAN_POINT ( 'NONE',  ( 14.32824189675854853, -293.9681046555747344, -322.0297335270641952 ) ) ;
#59928 = VERTEX_POINT ( 'NONE', #62557 ) ;
#59929 = CARTESIAN_POINT ( 'NONE',  ( -113.8802116867503145, -291.6924967883056752, -265.5290627889569350 ) ) ;
#59930 = CARTESIAN_POINT ( 'NONE',  ( -41.06466110886249510, -280.6554759195682891, -197.3540482569941048 ) ) ;
#59931 = CARTESIAN_POINT ( 'NONE',  ( -70.02067741567400105, -272.6909438608519736, -200.8852158456117820 ) ) ;
#59932 = CARTESIAN_POINT ( 'NONE',  ( 36.59091332883427583, -287.9359521538286799, -249.0230873958698794 ) ) ;
#59933 = CARTESIAN_POINT ( 'NONE',  ( 27.42930485019983067, -288.4324054879674577, -312.0582237548915714 ) ) ;
#59934 = CARTESIAN_POINT ( 'NONE',  ( -110.2496245091570728, -284.9499649275306297, -265.4680148169834411 ) ) ;
#59935 = LINE ( 'NONE', #58068, #17317 ) ;
#59936 = CARTESIAN_POINT ( 'NONE',  ( -100.6316193246363895, -246.5931397093643795, -333.0237302267296400 ) ) ;
#59937 = CARTESIAN_POINT ( 'NONE',  ( -39.45748113467511331, -139.8532795829076463, -360.8829801073189856 ) ) ;
#59938 = CARTESIAN_POINT ( 'NONE',  ( -8.684830022753116552, -275.8644938294555118, -337.6902561242339402 ) ) ;
#59939 = CARTESIAN_POINT ( 'NONE',  ( -93.85306733370345000, -276.8130911310531701, -317.0786652712330920 ) ) ;
#59940 = CARTESIAN_POINT ( 'NONE',  ( -34.75570499637699129, -297.5913720358046248, -193.4228652938332687 ) ) ;
#59941 = CARTESIAN_POINT ( 'NONE',  ( -104.5598740624659513, -261.7493365748397878, -316.1504158153062463 ) ) ;
#59942 = CARTESIAN_POINT ( 'NONE',  ( -98.15842529236812197, -290.4826491639692563, -310.8723386717459789 ) ) ;
#59943 = CARTESIAN_POINT ( 'NONE',  ( 19.23069837402722371, -299.5463773817224364, -193.5150897415832105 ) ) ;
#59944 = CARTESIAN_POINT ( 'NONE',  ( -95.01552854323075792, -273.8931649452441093, -219.4981422270397502 ) ) ;
#59945 = CARTESIAN_POINT ( 'NONE',  ( -107.8362130380808281, -296.9698491233963296, -251.3518349678664947 ) ) ;
#59946 = ORIENTED_EDGE ( 'NONE', *, *, #65700, .T. ) ;
#59947 = CARTESIAN_POINT ( 'NONE',  ( 196.8936505956917244, 70.76315252099192321, -10.57021625195834424 ) ) ;
#59948 = CARTESIAN_POINT ( 'NONE',  ( -102.3541008922031921, -279.9599116326868966, -308.9695364781742342 ) ) ;
#59949 = CARTESIAN_POINT ( 'NONE',  ( -31.64710392622223267, -282.4897672494021208, -347.1018050768863077 ) ) ;
#59950 = ADVANCED_FACE ( 'NONE', ( #75339 ), #82889, .T. ) ;
#59951 = CARTESIAN_POINT ( 'NONE',  ( -91.18557997915989688, -278.9196045203940457, -320.1849426367939486 ) ) ;
#59952 = CARTESIAN_POINT ( 'NONE',  ( -98.81658237866699324, -279.7115242311438124, -315.0465626485628263 ) ) ;
#59953 = CARTESIAN_POINT ( 'NONE',  ( -70.71870656527912047, -296.1777577622423223, -204.7624146363433226 ) ) ;
#59954 = FACE_OUTER_BOUND ( 'NONE', #68254, .T. ) ;
#59955 = CARTESIAN_POINT ( 'NONE',  ( 208.4306832106271088, -74.55766379199613425, 7.500000000000013323 ) ) ;
#59956 = CARTESIAN_POINT ( 'NONE',  ( -9.249308301015997102, -280.5966293190467695, -202.9829499609261063 ) ) ;
#59957 = CARTESIAN_POINT ( 'NONE',  ( 19.76405880992443187, -277.0544565268701831, -321.7918136389699839 ) ) ;
#59958 = CARTESIAN_POINT ( 'NONE',  ( 28.18736872967216556, -277.0655372054245049, -233.7723145199266241 ) ) ;
#59959 = CARTESIAN_POINT ( 'NONE',  ( -3.006269638561347879, -275.1822099983924659, -338.6375640229837245 ) ) ;
#59960 = ORIENTED_EDGE ( 'NONE', *, *, #1142, .T. ) ;
#59961 = CARTESIAN_POINT ( 'NONE',  ( 197.2116943569230330, 275.0000000000000568, -12.92446933126074882 ) ) ;
#59962 = CARTESIAN_POINT ( 'NONE',  ( -25.37262622998626327, -291.4056441699275410, -198.1337458989947606 ) ) ;
#59963 = CARTESIAN_POINT ( 'NONE',  ( 16.23412307829809365, -286.1374419462657102, -215.1982323242311566 ) ) ;
#59964 = CARTESIAN_POINT ( 'NONE',  ( -37.56579216964176027, -281.2948887900610089, -344.3867177952171232 ) ) ;
#59966 = CARTESIAN_POINT ( 'NONE',  ( 20.65215831188271878, -284.9847601820686691, -223.6715820239177503 ) ) ;
#59965 = CARTESIAN_POINT ( 'NONE',  ( -56.48956269030360033, -281.8785408671863593, -341.4155638312459473 ) ) ;
#59967 = CARTESIAN_POINT ( 'NONE',  ( 23.65080172314155149, -290.1469955183363254, -314.0927358630821686 ) ) ;
#59968 = CARTESIAN_POINT ( 'NONE',  ( 19.97653418451871232, -282.1130215345847319, -224.5162652557175136 ) ) ;
#59969 = CARTESIAN_POINT ( 'NONE',  ( -102.4795565685557790, -271.0489455320371803, -233.0808819269815046 ) ) ;
#59970 = CARTESIAN_POINT ( 'NONE',  ( -3.269032450612306739, -281.0096783425094031, -338.5334763367176834 ) ) ;
#59971 = CARTESIAN_POINT ( 'NONE',  ( 9.957276081149519342, -296.4011405635624783, -328.6329376264565099 ) ) ;
#59972 = CARTESIAN_POINT ( 'NONE',  ( -40.93771608963155018, -278.2473815861245043, -194.4465631866245587 ) ) ;
#59973 = CARTESIAN_POINT ( 'NONE',  ( -108.8627853391299709, -279.0043819126972267, -285.4815359254573650 ) ) ;
#59974 = CARTESIAN_POINT ( 'NONE',  ( -112.4947376363317915, -286.5925953426739738, -267.2171151802833720 ) ) ;
#59975 = CARTESIAN_POINT ( 'NONE',  ( 123.4306832106270946, -134.2641364535880939, 4.999999999999990230 ) ) ;
#59976 = CARTESIAN_POINT ( 'NONE',  ( -91.79169301609626075, -293.2037747349238543, -217.8985594117043547 ) ) ;
#59977 = CARTESIAN_POINT ( 'NONE',  ( -6.713583523252705021, -274.6499094297258239, -338.8221954292720284 ) ) ;
#59978 = CARTESIAN_POINT ( 'NONE',  ( 33.88878854897261306, -287.1175407733646807, -299.3190446538386595 ) ) ;
#59979 = CARTESIAN_POINT ( 'NONE',  ( -3.248766159620207539, -290.9101817495467799, -204.9079876501931494 ) ) ;
#59980 = DIRECTION ( 'NONE',  ( 0.000000000000000000, 0.000000000000000000, -1.000000000000000000 ) ) ;
#59981 = CARTESIAN_POINT ( 'NONE',  ( -54.08243044369199026, -275.9563074602513666, -341.9747163648090691 ) ) ;
#59982 = CARTESIAN_POINT ( 'NONE',  ( -96.60448239626387590, -294.0739507885874104, -315.0898748861079071 ) ) ;
#59983 = CARTESIAN_POINT ( 'NONE',  ( -108.9115299702456667, -292.0869143084013899, -253.6028031454002871 ) ) ;
#59984 = CARTESIAN_POINT ( 'NONE',  ( 165.2494399300530290, -11.64849832608277325, 10.00000000000000000 ) ) ;
#59985 = CARTESIAN_POINT ( 'NONE',  ( -7.443854635798750508, -290.9169794872181001, -200.1413211783660131 ) ) ;
#59986 = CARTESIAN_POINT ( 'NONE',  ( 35.78604678410714968, -289.0177414312382780, -260.0501408862831454 ) ) ;
#59987 = CARTESIAN_POINT ( 'NONE',  ( -112.1701820300762762, -288.9595082875632670, -257.1447527013571062 ) ) ;
#59988 = CARTESIAN_POINT ( 'NONE',  ( 7.269833936686640463, -288.0986812405787987, -211.7716587364999157 ) ) ;
#59989 = FACE_OUTER_BOUND ( 'NONE', #35841, .T. ) ;
#59990 = CARTESIAN_POINT ( 'NONE',  ( 33.18220331233044362, -288.0983141563156664, -250.8936895230266089 ) ) ;
#59991 = CARTESIAN_POINT ( 'NONE',  ( -1.466534964591752699, -296.5588674342830018, -336.6431706760815814 ) ) ;
#59992 = CARTESIAN_POINT ( 'NONE',  ( 82.64890176555634582, -299.5541904835138780, -197.7570935515976203 ) ) ;
#59993 = CARTESIAN_POINT ( 'NONE',  ( 36.76420277686428051, -289.0013069038577669, -289.7601868853059841 ) ) ;
#59994 = CARTESIAN_POINT ( 'NONE',  ( -72.96533557734936437, -277.6026813209381316, -203.9434512651407658 ) ) ;
#59995 = CARTESIAN_POINT ( 'NONE',  ( -38.54037258048894898, -277.4000767044311715, -347.3306410159770508 ) ) ;
#59996 = CARTESIAN_POINT ( 'NONE',  ( -8.864986838942877867, -280.0813804991981328, -198.8431405798105800 ) ) ;
#59997 = CARTESIAN_POINT ( 'NONE',  ( -44.75701922743524364, -299.9378694268813774, -196.0340335865562054 ) ) ;
#59998 = CARTESIAN_POINT ( 'NONE',  ( -49.72740002051758523, -283.8941529133288668, -196.3379803099534229 ) ) ;
#59999 = CARTESIAN_POINT ( 'NONE',  ( -48.18343439339133738, -279.1747503396557590, -502.4506777725324014 ) ) ;
#60000 = CARTESIAN_POINT ( 'NONE',  ( -34.23837009260996922, -278.2311321860943281, -196.1780528109326838 ) ) ;
#60001 = CARTESIAN_POINT ( 'NONE',  ( -52.53794309811355134, -281.2465061557251715, -343.8585641416272551 ) ) ;
#60002 = DIRECTION ( 'NONE',  ( 0.000000000000000000, 0.000000000000000000, 1.000000000000000000 ) ) ;
#60003 = CARTESIAN_POINT ( 'NONE',  ( -77.46693802465658507, -276.0596087175227922, -335.3276371634951261 ) ) ;
#60004 = CARTESIAN_POINT ( 'NONE',  ( -80.54575753980547859, -297.1701315814090663, -330.0613455692244429 ) ) ;
#60005 = CARTESIAN_POINT ( 'NONE',  ( 37.24451121664420583, -280.6971994382673756, -288.2605650847006586 ) ) ;
#60006 = CARTESIAN_POINT ( 'NONE',  ( -110.3326625622826782, -297.4069985505269642, -276.9326452309686033 ) ) ;
#60007 = CARTESIAN_POINT ( 'NONE',  ( -112.9638697334090125, -274.1199723198372453, -259.0500456937389231 ) ) ;
#60008 = CARTESIAN_POINT ( 'NONE',  ( -0.5319458963451971778, -274.2225929373191775, -207.2820357615500768 ) ) ;
#60009 = CARTESIAN_POINT ( 'NONE',  ( 30.20663376833570979, -295.9829947566333317, -303.0727378157774297 ) ) ;
#60010 = CARTESIAN_POINT ( 'NONE',  ( 9.809080576523538042, -286.8480423831206849, -209.4858037457485409 ) ) ;
#60011 = CARTESIAN_POINT ( 'NONE',  ( -92.01459899129939402, -277.3594001382181773, -218.1309640287522882 ) ) ;
#60012 = CARTESIAN_POINT ( 'NONE',  ( -89.49304150174650374, -289.5965242215511353, -327.0112512340981539 ) ) ;
#60013 = EDGE_CURVE ( 'NONE', #2870, #83522, #45751, .T. ) ;
#60014 = CARTESIAN_POINT ( 'NONE',  ( -66.43349028916553323, -288.5013157416526042, -337.6245103654333661 ) ) ;
#60015 = CARTESIAN_POINT ( 'NONE',  ( 22.39803500793282609, -290.9314232945565664, -224.9950232031948474 ) ) ;
#60016 = EDGE_LOOP ( 'NONE', ( #87484, #23495, #49536, #4706 ) ) ;
#60017 = CARTESIAN_POINT ( 'NONE',  ( 196.8803347170859865, 73.40565171261611965, 12.50000000000000533 ) ) ;
#60018 = CARTESIAN_POINT ( 'NONE',  ( -78.21402997820378289, -289.1256732226037798, -330.9814285970900301 ) ) ;
#60019 = DIRECTION ( 'NONE',  ( -0.000000000000000000, -0.9681751575201845705, 0.2502735790305593011 ) ) ;
#60020 = CARTESIAN_POINT ( 'NONE',  ( -49.31987434615352583, -286.8444318614805866, -194.4831196181479527 ) ) ;
#60021 = CARTESIAN_POINT ( 'NONE',  ( 17.36665895637874613, -295.4090924074130839, -226.6919474004047572 ) ) ;
#60022 = CARTESIAN_POINT ( 'NONE',  ( 31.97866207542431738, -292.1855170949002627, -237.2601640534593912 ) ) ;
#60023 = EDGE_CURVE ( 'NONE', #46969, #57853, #55465, .T. ) ;
#60024 = CARTESIAN_POINT ( 'NONE',  ( -58.33524340190015067, -284.6330159097171304, -343.9864239888361794 ) ) ;
#60025 = CARTESIAN_POINT ( 'NONE',  ( -58.95015643619222345, -283.1728226824019430, -340.1428384657923516 ) ) ;
#60026 = CARTESIAN_POINT ( 'NONE',  ( -91.63552747125348219, -297.3041668406910958, -215.7609319716147809 ) ) ;
#60027 = CARTESIAN_POINT ( 'NONE',  ( 34.85483683740542915, -276.6872371516304838, -256.6168999520595548 ) ) ;
#60028 = CARTESIAN_POINT ( 'NONE',  ( -36.15525363930201053, -290.0871741326099027, -195.7129860930606355 ) ) ;
#60029 = CARTESIAN_POINT ( 'NONE',  ( 32.44411336585147865, -274.0450347767934431, -247.4583256500109485 ) ) ;
#60030 = ORIENTED_EDGE ( 'NONE', *, *, #31052, .F. ) ;
#60031 = CARTESIAN_POINT ( 'NONE',  ( -71.74250447947856912, -195.9422791308210492, -360.7315132586310824 ) ) ;
#60032 = CARTESIAN_POINT ( 'NONE',  ( -74.29123523874994817, -287.4770865509159989, -205.7239995025852579 ) ) ;
#60033 = CARTESIAN_POINT ( 'NONE',  ( -93.44604478154516869, -298.3481232988896750, -217.9979353451291786 ) ) ;
#60034 = CARTESIAN_POINT ( 'NONE',  ( -93.33852299750604686, -285.8699476186229163, -223.3691133751094640 ) ) ;
#60035 = CARTESIAN_POINT ( 'NONE',  ( -73.99508255952055436, -276.5855836735034359, -337.8249430197521974 ) ) ;
#60036 = CARTESIAN_POINT ( 'NONE',  ( 11.04819745993944480, -293.3530312216186644, -210.5286586992511104 ) ) ;
#60037 = CARTESIAN_POINT ( 'NONE',  ( 35.51019780483819943, -285.4245286084055238, -249.3682159514878549 ) ) ;
#60038 = CARTESIAN_POINT ( 'NONE',  ( 26.49658173305608599, -294.4523386142902837, -313.3776038982574619 ) ) ;
#60039 = CARTESIAN_POINT ( 'NONE',  ( -91.69173430259594682, -291.5833271266084807, -221.5760195433436195 ) ) ;
#60040 = FACE_OUTER_BOUND ( 'NONE', #42669, .T. ) ;
#60041 = CARTESIAN_POINT ( 'NONE',  ( 154.0370857100322723, 19.38211809614433534, -11.97004389447338291 ) ) ;
#60042 = CARTESIAN_POINT ( 'NONE',  ( -46.80064229259274811, -155.6065870647230440, -361.5538532369098448 ) ) ;
#60043 = CARTESIAN_POINT ( 'NONE',  ( -100.4342404296290283, -286.6444321592520055, -227.3487617070399267 ) ) ;
#60044 = CARTESIAN_POINT ( 'NONE',  ( -54.42813229853333468, -295.3380690714489560, -195.3538533559490702 ) ) ;
#60045 = ORIENTED_EDGE ( 'NONE', *, *, #35632, .T. ) ;
#60046 = CARTESIAN_POINT ( 'NONE',  ( -65.44686644367027384, -282.3487444171194625, -338.0824241412300353 ) ) ;
#60047 = CARTESIAN_POINT ( 'NONE',  ( -103.5897598217109845, -277.7068393319694337, -309.6694710042850716 ) ) ;
#60048 = CARTESIAN_POINT ( 'NONE',  ( 36.29390644308807623, -283.7248411236676020, -283.7681907213568024 ) ) ;
#60049 = CARTESIAN_POINT ( 'NONE',  ( 198.8865589563561969, 282.5583194059946663, -111.0619671203250221 ) ) ;
#60050 = CARTESIAN_POINT ( 'NONE',  ( -34.51904984752484040, -281.5920573642800377, -346.7197385799287872 ) ) ;
#60051 = CARTESIAN_POINT ( 'NONE',  ( -7.576410142704281370, -284.4644072194051887, -201.9076716328407031 ) ) ;
#60052 = CARTESIAN_POINT ( 'NONE',  ( -75.82606838877276800, -275.4049506015747966, -205.0374892216299827 ) ) ;
#60053 = CARTESIAN_POINT ( 'NONE',  ( -65.60230355358891075, -298.1646704465148332, -202.9865921156171851 ) ) ;
#60054 = CARTESIAN_POINT ( 'NONE',  ( 29.19204912661200524, -291.8167075531522983, -239.0239114305246630 ) ) ;
#60055 = CARTESIAN_POINT ( 'NONE',  ( -111.7267238633212685, -278.9585843775696503, -289.9110675159396919 ) ) ;
#60056 = CARTESIAN_POINT ( 'NONE',  ( -11.25404169307784308, -276.7024905025317025, -338.5405435989334251 ) ) ;
#60057 = CARTESIAN_POINT ( 'NONE',  ( -85.62432355126473738, -274.4814469709464788, -210.7768853010366286 ) ) ;
#60058 = CARTESIAN_POINT ( 'NONE',  ( -94.98756247507560602, -276.7852675716887347, -320.9422119264992261 ) ) ;
#60059 = CARTESIAN_POINT ( 'NONE',  ( -110.4262895430651383, -266.6388475384649155, -306.9518243255700440 ) ) ;
#60060 = CARTESIAN_POINT ( 'NONE',  ( 32.88961892668422138, -273.8954262008013529, -296.8235451646469869 ) ) ;
#60061 = CARTESIAN_POINT ( 'NONE',  ( -3.473499367217985245, -296.0391763085331718, -338.8705111685437146 ) ) ;
#60062 = CARTESIAN_POINT ( 'NONE',  ( 151.7489156927949807, 20.88249531811356974, 8.613363710899784920 ) ) ;
#60063 = CARTESIAN_POINT ( 'NONE',  ( 165.2494399300530290, 8.542400036368780647, 10.00000000000000000 ) ) ;
#60064 = CARTESIAN_POINT ( 'NONE',  ( -91.88587535834876974, -284.9335426534595399, -319.3612137084307960 ) ) ;
#60065 = CARTESIAN_POINT ( 'NONE',  ( -37.29210996487410057, -284.8116373413867564, -346.3606654925657722 ) ) ;
#60066 = CARTESIAN_POINT ( 'NONE',  ( -62.59030357095917196, -285.0634391555424827, -201.7039252361940669 ) ) ;
#60067 = EDGE_CURVE ( 'NONE', #68073, #30213, #52514, .T. ) ;
#60068 = CARTESIAN_POINT ( 'NONE',  ( -111.1506026067404775, -276.9846385056405893, -267.8610541376225456 ) ) ;
#60069 = CARTESIAN_POINT ( 'NONE',  ( 18.55020681192583254, -284.0980071081172582, -319.2176448815467893 ) ) ;
#60070 = CARTESIAN_POINT ( 'NONE',  ( -24.73896594693563245, -278.6957374422057683, -197.7534128682572430 ) ) ;
#60071 = CARTESIAN_POINT ( 'NONE',  ( 5.588889963951293005, -277.5352739910390483, -329.8476334836412320 ) ) ;
#60072 = CARTESIAN_POINT ( 'NONE',  ( 175.2296996224750103, 249.5000000000000568, 0.000000000000000000 ) ) ;
#60073 = CARTESIAN_POINT ( 'NONE',  ( -21.92715326418548472, -274.7474043191746773, -198.9441719092578751 ) ) ;
#60074 = CARTESIAN_POINT ( 'NONE',  ( 37.71001984078320390, -282.5622074971882398, -286.8960834947649801 ) ) ;
#60075 = CARTESIAN_POINT ( 'NONE',  ( -56.54735872776912231, -280.3035094294096439, -195.8033444586691019 ) ) ;
#60076 = EDGE_LOOP ( 'NONE', ( #78289, #91587, #25569 ) ) ;
#60077 = ORIENTED_EDGE ( 'NONE', *, *, #81073, .T. ) ;
#60078 = CARTESIAN_POINT ( 'NONE',  ( 200.1633050441426747, 15.87263057655165532, -10.05743975622730524 ) ) ;
#60079 = CARTESIAN_POINT ( 'NONE',  ( -10.45482138025249874, -288.2595266745221352, -199.4716193110464246 ) ) ;
#60080 = CARTESIAN_POINT ( 'NONE',  ( -104.9074321217238293, -296.1248053154967579, -242.2991582027503625 ) ) ;
#60081 = CARTESIAN_POINT ( 'NONE',  ( -40.61976135454321479, -291.3605619703167235, -193.5197871089743842 ) ) ;
#60082 = CARTESIAN_POINT ( 'NONE',  ( 33.34041857083791172, -285.7581998457193322, -249.4660021938422005 ) ) ;
#60083 = CARTESIAN_POINT ( 'NONE',  ( 3.930180888038329545, -287.0593590692782868, -331.3487941644067973 ) ) ;
#60084 = CARTESIAN_POINT ( 'NONE',  ( -97.69112625662680216, -286.3363273289169797, -228.5647736578165166 ) ) ;
#60085 = CARTESIAN_POINT ( 'NONE',  ( -111.7299583593154750, -276.6797949464423709, -260.4073693525061799 ) ) ;
#60086 = CARTESIAN_POINT ( 'NONE',  ( -4.694487754694855575, -287.0291665085744057, -339.2274596313182542 ) ) ;
#60087 = CARTESIAN_POINT ( 'NONE',  ( 23.89696215297717785, -288.9637462005171642, -227.0397144218443941 ) ) ;
#60088 = CARTESIAN_POINT ( 'NONE',  ( -34.75601702405487003, -287.0195713830769932, -345.4833029360109435 ) ) ;
#60089 = CARTESIAN_POINT ( 'NONE',  ( -16.05269163242585151, -283.7112393347064199, -340.4338413838113979 ) ) ;
#60090 = CARTESIAN_POINT ( 'NONE',  ( -103.0207213337438645, -293.0377465651410489, -233.8057545256713468 ) ) ;
#60091 = CARTESIAN_POINT ( 'NONE',  ( 82.14284478241719967, -300.0267218569679244, -193.4142195599097533 ) ) ;
#60092 = CARTESIAN_POINT ( 'NONE',  ( 155.7140808774800007, 19.99999999999999645, -15.62500000000000178 ) ) ;
#60093 = CARTESIAN_POINT ( 'NONE',  ( -45.98979296249717663, -299.8634439075888167, -195.2976469253153766 ) ) ;
#60094 = CARTESIAN_POINT ( 'NONE',  ( 17.18998019359640850, -280.0530794719977621, -221.5871744418945184 ) ) ;
#60095 = CARTESIAN_POINT ( 'NONE',  ( 35.05055846913502648, -279.2993518184894128, -250.7067791094480640 ) ) ;
#60096 = CARTESIAN_POINT ( 'NONE',  ( 33.26414128774135293, -293.1377728287725972, -300.8100319795473183 ) ) ;
#60097 = CARTESIAN_POINT ( 'NONE',  ( -109.5181740824437213, -271.0052213271757182, -253.9742139346364240 ) ) ;
#60098 = CARTESIAN_POINT ( 'NONE',  ( 37.02697664948645695, -273.5766100585297522, -266.0800591831813904 ) ) ;
#60099 = CARTESIAN_POINT ( 'NONE',  ( -61.15724257057043900, -296.6829725821341412, -339.9424789945534826 ) ) ;
#60100 =( LENGTH_UNIT ( ) NAMED_UNIT ( * ) SI_UNIT ( .MILLI., .METRE. ) );
#60101 = CARTESIAN_POINT ( 'NONE',  ( -103.7086846919696512, -271.6237411656142058, -232.3863919452905122 ) ) ;
#60102 = CARTESIAN_POINT ( 'NONE',  ( -113.2233437110134133, -294.7300343687853683, -275.2515210284833529 ) ) ;
#60103 = CARTESIAN_POINT ( 'NONE',  ( 20.63599331096736478, -294.3434659884822509, -225.0200663288813132 ) ) ;
#60104 = CARTESIAN_POINT ( 'NONE',  ( 205.7381008070598227, 1.000000000000000888, 7.000000000000000000 ) ) ;
#60105 = CARTESIAN_POINT ( 'NONE',  ( 35.86962783226373119, -294.3601164790650841, -270.7506019270845741 ) ) ;
#60106 = CARTESIAN_POINT ( 'NONE',  ( 175.2296996224750103, 214.5000000000000568, 0.000000000000000000 ) ) ;
#60108 = CARTESIAN_POINT ( 'NONE',  ( 31.54005341148707942, -293.8755630787714495, -294.6848561595447791 ) ) ;
#60107 = CARTESIAN_POINT ( 'NONE',  ( -69.07667481921521357, -283.6570217192106043, -202.0001651731305685 ) ) ;
#60109 = CARTESIAN_POINT ( 'NONE',  ( 13.68078880008794229, -282.3606358612337317, -328.1010212976989351 ) ) ;
#60110 = CARTESIAN_POINT ( 'NONE',  ( -8.116955713747312728, -282.3520635717634377, -200.6676147848299081 ) ) ;
#60111 = CARTESIAN_POINT ( 'NONE',  ( -106.6582305779312350, -284.6485668294866969, -236.8803339739678506 ) ) ;
#60112 = CARTESIAN_POINT ( 'NONE',  ( -101.2647559451360451, -289.0747590808985024, -231.4526181405437910 ) ) ;
#60113 = B_SPLINE_CURVE_WITH_KNOTS ( 'NONE', 3,
 ( #79913, #7932, #54281, #52878, #39579, #61869, #53829, #33437, #88856, #89788 ),
 .UNSPECIFIED., .F., .F.,
 ( 4, 2, 2, 2, 4 ),
 ( -1.751965293301170726E-05, 0.002261625431216393936, 0.004540770515365799044, 0.006819915599515204152, 0.009099060683664610127 ),
 .UNSPECIFIED. ) ;
#60114 = CARTESIAN_POINT ( 'NONE',  ( 34.94597919716335355, -280.3445120974340625, -294.9628594690515229 ) ) ;
#60115 = CARTESIAN_POINT ( 'NONE',  ( -74.95823404620226427, -284.2245612456954404, -207.2244420008466079 ) ) ;
#60116 = CARTESIAN_POINT ( 'NONE',  ( 28.63080754990374999, -286.9840178760042591, -309.4650914356356566 ) ) ;
#60117 = CARTESIAN_POINT ( 'NONE',  ( 206.9189553108847122, 30.70889394204684208, 15.00000000000001776 ) ) ;
#60118 = CARTESIAN_POINT ( 'NONE',  ( -63.83738493670087877, -297.0034800188745407, -339.2949996874035605 ) ) ;
#60119 = CARTESIAN_POINT ( 'NONE',  ( -99.16227662721641423, -279.3767094134034323, -315.2924080061521863 ) ) ;
#60121 = CARTESIAN_POINT ( 'NONE',  ( -32.95750494528525110, -279.7756245676312687, -197.4717064098965977 ) ) ;
#60120 = CARTESIAN_POINT ( 'NONE',  ( 34.78778412533412023, -291.8540587322781903, -292.3492427028863290 ) ) ;
#60122 = CARTESIAN_POINT ( 'NONE',  ( -44.89915883971343646, -292.1257976000697454, -193.6799708958425583 ) ) ;
#60123 = CARTESIAN_POINT ( 'NONE',  ( -112.7725404520761145, -282.5653148040115639, -275.5932424697898000 ) ) ;
#60124 = CARTESIAN_POINT ( 'NONE',  ( -26.04539553192085677, -278.9084648984074875, -344.5055321279956502 ) ) ;
#60125 = ADVANCED_FACE ( 'NONE', ( #16538 ), #45392, .T. ) ;
#60126 = CARTESIAN_POINT ( 'NONE',  ( -12.94111007456871931, -293.7860022681561531, -339.4653921907678296 ) ) ;
#60127 = CARTESIAN_POINT ( 'NONE',  ( -26.54324336545797181, -296.1871694351947326, -195.3647908593901263 ) ) ;
#60128 = EDGE_LOOP ( 'NONE', ( #33147, #60737, #25194, #41807 ) ) ;
#60129 = FACE_OUTER_BOUND ( 'NONE', #92526, .T. ) ;
#60130 = CARTESIAN_POINT ( 'NONE',  ( 32.60289517677492199, -283.1902606646293634, -244.1438174813643798 ) ) ;
#60131 = CARTESIAN_POINT ( 'NONE',  ( -108.9462885836776849, -295.8676270808834943, -284.9414145441156734 ) ) ;
#60132 = DIRECTION ( 'NONE',  ( 0.000000000000000000, 1.000000000000000000, 0.000000000000000000 ) ) ;
#60133 = CARTESIAN_POINT ( 'NONE',  ( 10.64812456238590777, -272.1952119285918457, -210.2361428286349110 ) ) ;
#60134 = CARTESIAN_POINT ( 'NONE',  ( 23.51123663286032084, -274.1216616260454089, -223.4240406178885792 ) ) ;
#60135 = CARTESIAN_POINT ( 'NONE',  ( 39.08401493050234876, -288.8103014648780231, -265.8307958653457490 ) ) ;
#60136 = CARTESIAN_POINT ( 'NONE',  ( -96.55985825834288505, -289.7884929461734487, -313.0484668365041330 ) ) ;
#60137 = CARTESIAN_POINT ( 'NONE',  ( -92.74234073507324183, -280.7594970890079367, -221.7468872238774225 ) ) ;
#60138 = CARTESIAN_POINT ( 'NONE',  ( -106.1696470976915379, -274.5059144561298581, -243.5901003498948114 ) ) ;
#60139 = CARTESIAN_POINT ( 'NONE',  ( -95.09382783052089394, -277.9825165329937136, -225.0438502526426987 ) ) ;
#60140 = ORIENTED_EDGE ( 'NONE', *, *, #11778, .T. ) ;
#60141 = CARTESIAN_POINT ( 'NONE',  ( -18.54791832922530759, -274.1209492767274583, -195.6348497170022540 ) ) ;
#60142 = CARTESIAN_POINT ( 'NONE',  ( -86.90569370446500841, -293.2766925370726199, -214.7514189129017836 ) ) ;
#60143 = CARTESIAN_POINT ( 'NONE',  ( 160.5350683151633291, 249.5000000000000568, 20.22542485937379908 ) ) ;
#60144 = ADVANCED_FACE ( 'NONE', ( #10352 ), #81951, .T. ) ;
#60145 = CARTESIAN_POINT ( 'NONE',  ( -105.2045835335101742, -290.8387265926386931, -297.6726918875684191 ) ) ;
#60146 = DIRECTION ( 'NONE',  ( -1.000000000000000000, -0.000000000000000000, -0.000000000000000000 ) ) ;
#60147 = CARTESIAN_POINT ( 'NONE',  ( -50.33091995366235949, -290.0276058009588382, -195.7180630717236625 ) ) ;
#60148 = CARTESIAN_POINT ( 'NONE',  ( -84.08511472884470095, -297.0558748295205760, -214.1957211572884603 ) ) ;
#60149 = DIRECTION ( 'NONE',  ( 0.000000000000000000, 0.000000000000000000, 1.000000000000000000 ) ) ;
#60150 = CARTESIAN_POINT ( 'NONE',  ( -105.8821533741155889, -291.6362835345876761, -304.0209006586660507 ) ) ;
#60151 = CARTESIAN_POINT ( 'NONE',  ( -88.47809603358389552, -292.1948066931273615, -334.5364918783848793 ) ) ;
#60152 = CARTESIAN_POINT ( 'NONE',  ( -30.38561211151381514, -288.1403637805460107, -195.7997077712545604 ) ) ;
#60153 = CARTESIAN_POINT ( 'NONE',  ( -40.61072232799127590, -275.0931724856184815, -345.1357966490565445 ) ) ;
#60154 = CARTESIAN_POINT ( 'NONE',  ( -4.698228753427344806, -276.4056702911311731, -203.4462169109697243 ) ) ;
#60155 = CARTESIAN_POINT ( 'NONE',  ( -33.40836774472629855, -290.1818665307650349, -196.0123647669730076 ) ) ;
#60156 = CARTESIAN_POINT ( 'NONE',  ( -38.18038781605122978, -281.9021564278876326, -194.6009563713172383 ) ) ;
#60157 = ORIENTED_EDGE ( 'NONE', *, *, #45253, .F. ) ;
#60158 = CARTESIAN_POINT ( 'NONE',  ( 30.42592407771797269, -281.2673194061783306, -297.7735563531068124 ) ) ;
#60159 = CARTESIAN_POINT ( 'NONE',  ( -68.87565776265314810, -278.5367690266302247, -340.2832742911587616 ) ) ;
#60160 = CARTESIAN_POINT ( 'NONE',  ( -76.56782556689915964, -282.3592685663999760, -336.2201920078268813 ) ) ;
#60161 = CARTESIAN_POINT ( 'NONE',  ( -91.15551542514162975, -278.7352955428076484, -325.1794351223465469 ) ) ;
#60162 =( NAMED_UNIT ( * ) SI_UNIT ( $, .STERADIAN. ) SOLID_ANGLE_UNIT ( ) );
#60163 = CARTESIAN_POINT ( 'NONE',  ( 15.53255164632434315, -276.3039156527190698, -215.3427460433160832 ) ) ;
#60164 = CARTESIAN_POINT ( 'NONE',  ( -102.0172624299486870, -280.6233781216988064, -301.5434626090942061 ) ) ;
#60165 = ORIENTED_EDGE ( 'NONE', *, *, #40970, .T. ) ;
#60166 = VERTEX_POINT ( 'NONE', #46335 ) ;
#60167 = CARTESIAN_POINT ( 'NONE',  ( -107.6904353227772901, -298.8914970349131295, -244.2101000726262612 ) ) ;
#60168 = CARTESIAN_POINT ( 'NONE',  ( -26.41529573755634885, -289.9896548858116603, -342.9026579866572320 ) ) ;
#60169 = CARTESIAN_POINT ( 'NONE',  ( -6.858512891713676396, -274.6701744502375959, -338.4979076164985372 ) ) ;
#60170 = CARTESIAN_POINT ( 'NONE',  ( -7.299652639978720714, -290.4236878280474343, -340.1709421014539316 ) ) ;
#60171 = CARTESIAN_POINT ( 'NONE',  ( -60.28309630248881490, -291.0954291505530591, -200.8991811606387898 ) ) ;
#60172 = CARTESIAN_POINT ( 'NONE',  ( 10.18500508836902796, -287.9245591271960620, -330.9329336872447129 ) ) ;
#60173 = CARTESIAN_POINT ( 'NONE',  ( 152.0128028882535034, 20.82798718771465829, -9.301361753755829298 ) ) ;
#60174 = CARTESIAN_POINT ( 'NONE',  ( -111.1083650188672465, -282.9809582191699633, -268.1431089663556691 ) ) ;
#60175 = CARTESIAN_POINT ( 'NONE',  ( -83.29259632869344898, -291.5499034077038232, -328.6653255132981144 ) ) ;
#60176 = CARTESIAN_POINT ( 'NONE',  ( -81.88239411230510711, -283.9124467166165005, -211.6513715178007544 ) ) ;
#60177 = CARTESIAN_POINT ( 'NONE',  ( 20.89651535950630290, -282.2404050807076601, -225.5126246587260823 ) ) ;
#60178 = CARTESIAN_POINT ( 'NONE',  ( 38.44464974120310785, -288.6507145488807851, -282.9013639530062960 ) ) ;
#60179 = CARTESIAN_POINT ( 'NONE',  ( -109.1937588055996144, -279.2189980024490410, -257.1221563315460799 ) ) ;
#60180 = CARTESIAN_POINT ( 'NONE',  ( -3.482959689871361952, -291.2840846420069170, -201.6327945492602396 ) ) ;
#60181 = CARTESIAN_POINT ( 'NONE',  ( 14.13111054126479793, -287.5558469833566733, -213.2396894451537435 ) ) ;
#60182 = CARTESIAN_POINT ( 'NONE',  ( 22.03867827054667927, -287.3866424217281406, -221.4377333414403211 ) ) ;
#60183 = CARTESIAN_POINT ( 'NONE',  ( -109.8724925711547087, -284.6040743325395965, -279.0604625725920869 ) ) ;
#60184 = ORIENTED_EDGE ( 'NONE', *, *, #44915, .T. ) ;
#60185 = CARTESIAN_POINT ( 'NONE',  ( 208.4306832106271088, 0.04196010845015910040, -7.500000000000013323 ) ) ;
#60186 = CARTESIAN_POINT ( 'NONE',  ( -7.695715735095363108, -294.2969712121603720, -200.6231364379452771 ) ) ;
#60187 = CARTESIAN_POINT ( 'NONE',  ( 23.62578397985801715, -292.8567483778737710, -316.5808557125232028 ) ) ;
#60188 = CARTESIAN_POINT ( 'NONE',  ( 28.23587354593491838, -275.0529397128208302, -303.0789345688033904 ) ) ;
#60189 = CARTESIAN_POINT ( 'NONE',  ( -82.90349917195925400, -296.7959896746002642, -208.3479271522658109 ) ) ;
#60190 = CARTESIAN_POINT ( 'NONE',  ( 29.01046979033746354, -292.4632787213426468, -302.5426920484623565 ) ) ;
#60191 = CARTESIAN_POINT ( 'NONE',  ( -80.29821245380310302, -295.7011154739013818, -210.0891339426439970 ) ) ;
#60192 = CARTESIAN_POINT ( 'NONE',  ( -33.50293255450065288, -293.3065915030982183, -197.0519386510420361 ) ) ;
#60193 = CARTESIAN_POINT ( 'NONE',  ( 33.60389554548378044, -294.3890767478114299, -251.8963263797545551 ) ) ;
#60194 = FACE_OUTER_BOUND ( 'NONE', #82034, .T. ) ;
#60195 = CARTESIAN_POINT ( 'NONE',  ( -63.64898561860923820, -293.3941268106640905, -340.7738665185340210 ) ) ;
#60196 = CARTESIAN_POINT ( 'NONE',  ( -110.4115052554880521, -298.7700237323742272, -253.3996235229373326 ) ) ;
#60197 = CARTESIAN_POINT ( 'NONE',  ( 34.24321491439282283, -288.6974187575096948, -285.8798756206513758 ) ) ;
#60198 = CARTESIAN_POINT ( 'NONE',  ( 17.71898388876078201, -278.2489727771535399, -321.8074772184902486 ) ) ;
#60199 = CARTESIAN_POINT ( 'NONE',  ( 5.635761406164304432, -275.2788306918330932, -333.7720517227579080 ) ) ;
#60200 = CARTESIAN_POINT ( 'NONE',  ( -32.68048206436853320, -273.4580076966628326, -193.5913184391545201 ) ) ;
#60201 = CARTESIAN_POINT ( 'NONE',  ( 35.63767361693135882, -279.8226556343589664, -285.0991268998797068 ) ) ;
#60202 = CARTESIAN_POINT ( 'NONE',  ( -107.9231706006774516, -276.5834894489800604, -299.0786464215859155 ) ) ;
#60203 = EDGE_CURVE ( 'NONE', #92631, #59201, #71454, .T. ) ;
#60204 = CARTESIAN_POINT ( 'NONE',  ( -99.15710950568829674, -294.6894605470060355, -310.2048317315768031 ) ) ;
#60205 = CARTESIAN_POINT ( 'NONE',  ( -112.3426406673569460, -274.5876385001751032, -267.6101980901121919 ) ) ;
#60206 = CARTESIAN_POINT ( 'NONE',  ( -110.4436330666481183, -273.2034605540640086, -270.3693926218427919 ) ) ;
#60207 = FACE_OUTER_BOUND ( 'NONE', #35504, .T. ) ;
#60209 = CARTESIAN_POINT ( 'NONE',  ( -36.73393744560132745, -273.8933171697080979, -197.3512329030607759 ) ) ;
#60208 = CARTESIAN_POINT ( 'NONE',  ( -71.40569764138540165, -289.6247439370711731, -203.1303845220607514 ) ) ;
#60210 = CARTESIAN_POINT ( 'NONE',  ( -20.49640521205113686, -288.8417219096920689, -345.5505711178771548 ) ) ;
#60211 = CARTESIAN_POINT ( 'NONE',  ( -110.6607944582050607, -274.7645059448481675, -253.7979408056417867 ) ) ;
#60212 = CARTESIAN_POINT ( 'NONE',  ( -108.6232173118451385, -294.2553407670069987, -293.3100488120630871 ) ) ;
#60213 = CARTESIAN_POINT ( 'NONE',  ( 13.56614023886991482, -281.5579325093266903, -327.9866943903553533 ) ) ;
#60214 = DIRECTION ( 'NONE',  ( -1.000000000000000000, 0.000000000000000000, 0.000000000000000000 ) ) ;
#60215 = CARTESIAN_POINT ( 'NONE',  ( 36.03842940642930159, -279.3521498507132605, -254.7967583021844007 ) ) ;
#60216 = CARTESIAN_POINT ( 'NONE',  ( 199.8263553767660312, 25.49203953695227653, 10.63455718553152352 ) ) ;
#60217 = CARTESIAN_POINT ( 'NONE',  ( -106.4113925128306732, -289.0181810814100913, -295.1906990955588981 ) ) ;
#60218 = CARTESIAN_POINT ( 'NONE',  ( -110.7229842665056054, -282.5418030374244154, -281.9189072579788444 ) ) ;
#60219 = CARTESIAN_POINT ( 'NONE',  ( 165.2494399300530290, 8.542400036368780647, 10.00000000000000000 ) ) ;
#60220 = DIRECTION ( 'NONE',  ( -0.000000000000000000, -1.000000000000000000, -0.000000000000000000 ) ) ;
#60221 = CARTESIAN_POINT ( 'NONE',  ( -112.1188241497729052, -288.4696180742941465, -276.7763032269879773 ) ) ;
#60222 = CARTESIAN_POINT ( 'NONE',  ( -72.25311772611807726, -275.1019721937089457, -205.4050948290368979 ) ) ;
#60223 = CARTESIAN_POINT ( 'NONE',  ( -37.29898738808524428, -284.2566617434163732, -346.9770331353863639 ) ) ;
#60225 = CARTESIAN_POINT ( 'NONE',  ( -109.6122248940153412, -284.6879502116936465, -260.0668841569407164 ) ) ;
#60224 = CARTESIAN_POINT ( 'NONE',  ( -43.89306941923850758, -272.0499383651509788, -195.0333546889487764 ) ) ;
#60226 = CARTESIAN_POINT ( 'NONE',  ( -1.164857568720132130, -277.9877671385102644, -334.5016323174721151 ) ) ;
#60227 = CARTESIAN_POINT ( 'NONE',  ( -13.72362006023690739, -277.5405924947315270, -339.6587842107962274 ) ) ;
#60228 = CARTESIAN_POINT ( 'NONE',  ( -78.05218136899647163, -285.5995863308420439, -333.3504612427573761 ) ) ;
#60229 = EDGE_CURVE ( 'NONE', #93421, #40890, #10819, .T. ) ;
#60230 = VECTOR ( 'NONE', #86666, 1000.000000000000000 ) ;
#60231 = ORIENTED_EDGE ( 'NONE', *, *, #35872, .T. ) ;
#60232 = CARTESIAN_POINT ( 'NONE',  ( -110.7796250023127413, -271.2951657040497935, -270.3451135339026905 ) ) ;
#60233 = CARTESIAN_POINT ( 'NONE',  ( -79.47873886606210192, -295.4378054795741377, -334.8085381860692564 ) ) ;
#60234 = CARTESIAN_POINT ( 'NONE',  ( -11.47513166114145555, -288.3706622350141515, -200.3413533579721957 ) ) ;
#60235 = CARTESIAN_POINT ( 'NONE',  ( 195.4776723108872716, 27.11938025175527045, 14.98434631268485084 ) ) ;
#60236 = CARTESIAN_POINT ( 'NONE',  ( -117.3417001280813707, -275.0519495502701943, -270.3929463913696054 ) ) ;
#60237 = CARTESIAN_POINT ( 'NONE',  ( -111.1467946632371167, -277.2102500921432124, -291.2009963621537167 ) ) ;
#60238 = CARTESIAN_POINT ( 'NONE',  ( -106.5254538032993707, -289.3663254432653389, -238.2972757114068258 ) ) ;
#60239 = CARTESIAN_POINT ( 'NONE',  ( -88.18673389239081928, -286.8445716099072911, -217.0179807214520906 ) ) ;
#60240 = CARTESIAN_POINT ( 'NONE',  ( -103.0659069813546580, -280.7701125916995011, -236.2156670393682987 ) ) ;
#60241 = CARTESIAN_POINT ( 'NONE',  ( -66.97741093497941733, -287.0965170357496845, -199.9315010687141410 ) ) ;
#60242 = CARTESIAN_POINT ( 'NONE',  ( -7.680462126197816097, -284.6635433944708780, -339.2466143603145383 ) ) ;
#60243 = CARTESIAN_POINT ( 'NONE',  ( -41.38232289034768030, -277.2683565401914620, -347.2682366834074514 ) ) ;
#60244 = CARTESIAN_POINT ( 'NONE',  ( -35.74699414900050698, -296.0923198386323065, -195.7168507407495781 ) ) ;
#60245 = CARTESIAN_POINT ( 'NONE',  ( -64.74034322147507226, -279.5375379301183330, -198.3443836432581406 ) ) ;
#60246 = CARTESIAN_POINT ( 'NONE',  ( -102.4863371415567599, -298.9550658739826190, -234.3404230450854868 ) ) ;
#60247 = DIRECTION ( 'NONE',  ( 0.000000000000000000, 0.000000000000000000, 1.000000000000000000 ) ) ;
#60248 = EDGE_CURVE ( 'NONE', #35701, #54214, #50274, .T. ) ;
#60249 = CARTESIAN_POINT ( 'NONE',  ( -106.6662871844225293, -275.4805209788417528, -237.0123917617630980 ) ) ;
#60250 = CARTESIAN_POINT ( 'NONE',  ( 74.14484272234649609, -297.5732043206075446, -194.6311733944271793 ) ) ;
#60251 = DIRECTION ( 'NONE',  ( 0.000000000000000000, 0.000000000000000000, 1.000000000000000000 ) ) ;
#60252 = CARTESIAN_POINT ( 'NONE',  ( -36.47172746892963602, -276.5486457846513417, -343.4299548495921499 ) ) ;
#60253 = CARTESIAN_POINT ( 'NONE',  ( -44.02349718850356908, -275.1746640943948137, -193.9971262066018483 ) ) ;
#60254 = CARTESIAN_POINT ( 'NONE',  ( 34.10982527358357430, -280.2524243061703260, -242.1535515154855602 ) ) ;
#60255 = CARTESIAN_POINT ( 'NONE',  ( -53.60974514382409239, -291.0238988515947085, -342.5644747067432831 ) ) ;
#60256 = CARTESIAN_POINT ( 'NONE',  ( -113.0888950202087671, -298.1886702332307095, -261.1377662027001634 ) ) ;
#60257 = CARTESIAN_POINT ( 'NONE',  ( -61.45195794554442159, -296.5634570477599254, -343.1262905628850604 ) ) ;
#60258 = CARTESIAN_POINT ( 'NONE',  ( 5.533705379969268812, -294.6339370999251628, -208.9646833250910731 ) ) ;
#60259 = CARTESIAN_POINT ( 'NONE',  ( 36.13918433175174272, -279.3688671727073256, -256.1305820727551463 ) ) ;
#60260 = CARTESIAN_POINT ( 'NONE',  ( -38.39838872102135525, -281.9589619749160079, -195.9159684115177242 ) ) ;
#60261 = CARTESIAN_POINT ( 'NONE',  ( -97.24484975780916329, -295.2396601323035839, -226.1476748521939442 ) ) ;
#60262 = CARTESIAN_POINT ( 'NONE',  ( -112.8041653303977228, -286.0139173228913023, -281.3093389377768858 ) ) ;
#60263 = CARTESIAN_POINT ( 'NONE',  ( -96.02399003453884063, -288.8580964210298134, -314.3208354987219764 ) ) ;
#60264 = CARTESIAN_POINT ( 'NONE',  ( -82.33048564276411696, -220.3546857680660196, -352.1821843074090452 ) ) ;
#60265 = ORIENTED_EDGE ( 'NONE', *, *, #53277, .F. ) ;
#60266 = CARTESIAN_POINT ( 'NONE',  ( -36.11464794040890780, -287.6118182440138753, -346.7750486394689347 ) ) ;
#60267 = CARTESIAN_POINT ( 'NONE',  ( 34.98072400148332406, -287.3529688752091147, -280.5295414112006824 ) ) ;
#60268 = ORIENTED_EDGE ( 'NONE', *, *, #80317, .F. ) ;
#60269 = CARTESIAN_POINT ( 'NONE',  ( -71.58831737021651520, -284.5736588485382299, -338.9808069832134834 ) ) ;
#60270 = CARTESIAN_POINT ( 'NONE',  ( -14.06271774850366540, -274.6959185158779064, -201.1500172392267132 ) ) ;
#60271 = ADVANCED_FACE ( 'NONE', ( #25959 ), #61512, .F. ) ;
#60272 = CARTESIAN_POINT ( 'NONE',  ( -34.95619835613400994, -291.0017558241210622, -193.6942414667640833 ) ) ;
#60273 = CARTESIAN_POINT ( 'NONE',  ( 38.56855941326944048, -282.3584503686267340, -282.7294047206377172 ) ) ;
#60274 = CARTESIAN_POINT ( 'NONE',  ( -9.135554972707513599, -281.9344844748413266, -199.4589238809577978 ) ) ;
#60275 = CARTESIAN_POINT ( 'NONE',  ( -6.242801423961558349, -280.7829446263093587, -199.9295028669648104 ) ) ;
#60276 = CARTESIAN_POINT ( 'NONE',  ( -68.52329096929361185, -279.6305960739908301, -204.3557515900368458 ) ) ;
#60277 = CARTESIAN_POINT ( 'NONE',  ( 7.399455738971487229, -291.9094976428775681, -326.5171145203363494 ) ) ;
#60278 = CARTESIAN_POINT ( 'NONE',  ( -95.01368496865339353, -240.5153381641504495, -341.9424385301951475 ) ) ;
#60279 = VERTEX_POINT ( 'NONE', #83253 ) ;
#60280 = CARTESIAN_POINT ( 'NONE',  ( 31.98586378361875759, -277.9220439906721936, -298.6721042649011224 ) ) ;
#60281 = CARTESIAN_POINT ( 'NONE',  ( 188.9470303086956164, 271.4955109107032172, -139.4255392735582006 ) ) ;
#60282 = CARTESIAN_POINT ( 'NONE',  ( 22.66595197881656176, -278.9633109306001870, -225.9444556358551779 ) ) ;
#60283 = CARTESIAN_POINT ( 'NONE',  ( -37.14101340303343335, -297.4033232792091894, -197.2563542109352284 ) ) ;
#60284 = CARTESIAN_POINT ( 'NONE',  ( 39.54515796689923235, -293.0950701058832237, -273.1785557095368517 ) ) ;
#60285 = CARTESIAN_POINT ( 'NONE',  ( 154.0301839824525985, 204.4104515755834086, -214.4894503002514341 ) ) ;
#60287 = CARTESIAN_POINT ( 'NONE',  ( -71.56161040001792628, -287.9119001957585056, -335.7622317474711622 ) ) ;
#60286 = CARTESIAN_POINT ( 'NONE',  ( -89.19502213159468340, -295.9146647860602570, -214.1660304428902180 ) ) ;
#60288 = CARTESIAN_POINT ( 'NONE',  ( -66.51713264913252033, -297.2987928475288868, -338.6228174872716181 ) ) ;
#60289 = CARTESIAN_POINT ( 'NONE',  ( -38.65037451406145408, -287.3506136791974086, -196.8670521539149263 ) ) ;
#60290 = VERTEX_POINT ( 'NONE', #54840 ) ;
#60291 = CARTESIAN_POINT ( 'NONE',  ( 34.23906574697407734, -294.1393536794490728, -242.4831755626318284 ) ) ;
#60292 = CARTESIAN_POINT ( 'NONE',  ( -95.96737624409604450, -284.4334301758705692, -313.9617893278019096 ) ) ;
#60293 = CARTESIAN_POINT ( 'NONE',  ( -43.24377113548126772, -296.7742550785668527, -193.9329620962970750 ) ) ;
#60294 = CARTESIAN_POINT ( 'NONE',  ( 22.07787360660950782, -293.6993719801215548, -221.6428146621456960 ) ) ;
#60295 = CARTESIAN_POINT ( 'NONE',  ( 35.39237964450586560, -293.7262164888749112, -245.1144232785966324 ) ) ;
#60296 = CARTESIAN_POINT ( 'NONE',  ( -63.81891468975411641, -289.5737869967754818, -338.4443925058523632 ) ) ;
#60297 = ORIENTED_EDGE ( 'NONE', *, *, #74314, .T. ) ;
#60298 = CARTESIAN_POINT ( 'NONE',  ( 159.0442047513580235, 16.98551211945798656, 9.330684800570141491 ) ) ;
#60299 = CARTESIAN_POINT ( 'NONE',  ( -92.77545552695330855, -299.1287418647900722, -218.6376460912532593 ) ) ;
#60300 = CARTESIAN_POINT ( 'NONE',  ( -78.61463545351449511, -272.3043817426019473, -205.8277659264548163 ) ) ;
#60301 = CARTESIAN_POINT ( 'NONE',  ( 35.37191193793383093, -280.7310580270817582, -279.4994516254529913 ) ) ;
#60302 = ORIENTED_EDGE ( 'NONE', *, *, #30492, .T. ) ;
#60303 = ORIENTED_EDGE ( 'NONE', *, *, #2955, .T. ) ;
#60304 = CARTESIAN_POINT ( 'NONE',  ( -4.027173323994664322, -276.1321952319327693, -339.7273831865137481 ) ) ;
#60305 = AXIS2_PLACEMENT_3D ( 'NONE', #40023, #62793, #40475 ) ;
#60306 = CARTESIAN_POINT ( 'NONE',  ( -90.76177888933847271, -271.6785891852978807, -219.4237229612803617 ) ) ;
#60307 = CARTESIAN_POINT ( 'NONE',  ( -110.8482623037358366, -280.5518020876081096, -259.6281508827213997 ) ) ;
#60308 = CARTESIAN_POINT ( 'NONE',  ( 3.799293095429488787, -274.6313957641800698, -332.1533841260673512 ) ) ;
#60309 = CARTESIAN_POINT ( 'NONE',  ( -92.15157593434433636, -298.4514762476190413, -221.5450548524433430 ) ) ;
#60310 = CARTESIAN_POINT ( 'NONE',  ( -100.9279926597968284, -273.9908707611533032, -233.9246674225685467 ) ) ;
#60311 = CARTESIAN_POINT ( 'NONE',  ( -111.1882564979777186, -297.9140611442166460, -289.2053987739818126 ) ) ;
#60312 = CARTESIAN_POINT ( 'NONE',  ( 29.79652972768992925, -273.1219726962755203, -236.1432148959524397 ) ) ;
#60313 = CARTESIAN_POINT ( 'NONE',  ( 10.36430436560265989, -295.0243135278672071, -325.7509167103522714 ) ) ;
#60314 = CARTESIAN_POINT ( 'NONE',  ( -22.60503324030578298, -290.8192225406309035, -198.2625357183725043 ) ) ;
#60315 = CARTESIAN_POINT ( 'NONE',  ( 194.7510731661265595, -164.3527196417747405, -21.50000000000000000 ) ) ;
#60316 = CARTESIAN_POINT ( 'NONE',  ( -67.67856717981702275, -277.9320459888386949, -341.0661489269728577 ) ) ;
#60317 = CARTESIAN_POINT ( 'NONE',  ( -85.31176140418813247, -273.5343660305431399, -215.2676291830930779 ) ) ;
#60318 = CARTESIAN_POINT ( 'NONE',  ( -41.55881333526495780, -281.7889124891074744, -346.8036464413556814 ) ) ;
#60319 = CARTESIAN_POINT ( 'NONE',  ( 12.20692942455942642, -296.3652147582964176, -326.9541434600171783 ) ) ;
#60320 = DIRECTION ( 'NONE',  ( 0.000000000000000000, 1.000000000000000000, 0.000000000000000000 ) ) ;
#60321 = CARTESIAN_POINT ( 'NONE',  ( -110.4806728384389771, -283.7062194877621550, -273.6351884539421349 ) ) ;
#60322 = CARTESIAN_POINT ( 'NONE',  ( -64.61140155105918836, -281.4071551656447241, -340.4206266324717376 ) ) ;
#60323 = ADVANCED_FACE ( 'NONE', ( #47256 ), #76169, .T. ) ;
#60324 = CARTESIAN_POINT ( 'NONE',  ( 35.28571244093176773, -274.2860847551515917, -282.5274744170075678 ) ) ;
#60325 = CARTESIAN_POINT ( 'NONE',  ( 28.35337820628796379, -283.0699347400537249, -234.0724968215549211 ) ) ;
#60326 = DIRECTION ( 'NONE',  ( -1.000000000000000000, 0.000000000000000000, 0.000000000000000000 ) ) ;
#60327 = CARTESIAN_POINT ( 'NONE',  ( -112.3417001280813849, -275.0519495502701943, -270.3929463913730729 ) ) ;
#60328 = CARTESIAN_POINT ( 'NONE',  ( -31.30293086102659572, -272.5270667090164238, -194.3876317211995399 ) ) ;
#60329 = CARTESIAN_POINT ( 'NONE',  ( -90.02545959419016697, -279.7940334233845761, -324.0478788431071280 ) ) ;
#60330 = LINE ( 'NONE', #44224, #10521 ) ;
#60331 = CARTESIAN_POINT ( 'NONE',  ( -69.20824167837935192, -287.5564359016947265, -201.8354313154490001 ) ) ;
#60332 = CARTESIAN_POINT ( 'NONE',  ( -110.1095955710663645, -288.7858685791759399, -252.1481033439261239 ) ) ;
#60333 = CARTESIAN_POINT ( 'NONE',  ( 209.2599468862078140, 293.9636489450776367, -59.00000000000003553 ) ) ;
#60334 = CARTESIAN_POINT ( 'NONE',  ( -93.39552501683924390, -294.6771571863573627, -317.7630714065162465 ) ) ;
#60335 = CARTESIAN_POINT ( 'NONE',  ( -66.84130882736201329, -287.5823003259767461, -338.5382902689954108 ) ) ;
#60336 = CARTESIAN_POINT ( 'NONE',  ( 122.2132510144744231, 146.9671518294229884, -260.0597590233358574 ) ) ;
#60337 = CARTESIAN_POINT ( 'NONE',  ( -66.32264754545623475, -295.6725654130979706, -201.1866621677464195 ) ) ;
#60338 = CARTESIAN_POINT ( 'NONE',  ( 34.41381725791989510, -286.3646009679407030, -296.4734274704601376 ) ) ;
#60339 = CARTESIAN_POINT ( 'NONE',  ( 36.50357674861623991, -283.1645900003296674, -271.3038625489959941 ) ) ;
#60340 = CARTESIAN_POINT ( 'NONE',  ( -60.93856772378150310, -281.5940001801135963, -342.6459994047218629 ) ) ;
#60341 = CARTESIAN_POINT ( 'NONE',  ( -110.1226431689860163, -290.4694564193342217, -276.6299076501842933 ) ) ;
#60342 = CARTESIAN_POINT ( 'NONE',  ( 36.01798336709773452, -283.0614899264870132, -276.7846554825192698 ) ) ;
#60343 = CARTESIAN_POINT ( 'NONE',  ( 18.62447054245579636, -283.0230564430576692, -317.5015775549690602 ) ) ;
#60344 = CARTESIAN_POINT ( 'NONE',  ( -18.11904906768154433, -290.7854634704876275, -343.2232925734124933 ) ) ;
#60345 = CARTESIAN_POINT ( 'NONE',  ( -114.3205561439199016, -272.8853797068901486, -270.3653521014397825 ) ) ;
#60346 = VERTEX_POINT ( 'NONE', #4199 ) ;
#60347 = CARTESIAN_POINT ( 'NONE',  ( -36.13483442274355895, -287.1170165586009375, -345.9243486391231386 ) ) ;
#60348 = CARTESIAN_POINT ( 'NONE',  ( 39.13758532672542145, -275.6695467902663950, -279.7478967641140457 ) ) ;
#60349 = CARTESIAN_POINT ( 'NONE',  ( 22.29299383757311404, -294.9154489403833281, -225.4662398637358649 ) ) ;
#60350 = FACE_OUTER_BOUND ( 'NONE', #87608, .T. ) ;
#60351 = CARTESIAN_POINT ( 'NONE',  ( -106.6379572354042296, -286.6233781216988064, -303.7686719486574702 ) ) ;
#60352 = CARTESIAN_POINT ( 'NONE',  ( 19.41871461515636454, -274.2343777766545259, -319.6582094377096155 ) ) ;
#60353 = CARTESIAN_POINT ( 'NONE',  ( 151.3768371069326690, 130.9657748190496704, -11.49999999999999645 ) ) ;
#60354 = CARTESIAN_POINT ( 'NONE',  ( -112.0998145659246603, -295.1393257513942672, -255.5406399483490816 ) ) ;
#60355 = CARTESIAN_POINT ( 'NONE',  ( -110.9184965776258025, -292.0693271024657633, -276.7188878244583066 ) ) ;
#60356 = CARTESIAN_POINT ( 'NONE',  ( -54.22704220152846943, -273.1780817950580058, -199.2360317549228910 ) ) ;
#60357 = CARTESIAN_POINT ( 'NONE',  ( -95.48576876399165769, -291.4401111558981370, -315.6581479910167900 ) ) ;
#60358 = CARTESIAN_POINT ( 'NONE',  ( -36.21449393256687443, -293.0078456164562795, -197.1219812885336466 ) ) ;
#60359 = CARTESIAN_POINT ( 'NONE',  ( -94.04569903959664146, -286.9784963019735073, -222.7940019961555436 ) ) ;
#60360 = CARTESIAN_POINT ( 'NONE',  ( -70.65732792718868893, -293.0466318752395978, -201.5957543171193151 ) ) ;
#60361 = CARTESIAN_POINT ( 'NONE',  ( -2.296752405834777910, -293.8212157918388243, -202.3379816396223134 ) ) ;
#60362 = CARTESIAN_POINT ( 'NONE',  ( -10.49197628768942359, -294.5251384784609741, -338.2440490787099634 ) ) ;
#60363 = CARTESIAN_POINT ( 'NONE',  ( 21.05686653724457358, -288.9044396604714393, -223.2811554807071843 ) ) ;
#60364 = CARTESIAN_POINT ( 'NONE',  ( 31.07811630528027180, -282.1741526931518251, -305.6843217402886239 ) ) ;
#60365 = CARTESIAN_POINT ( 'NONE',  ( -92.59277407053893683, -295.3487818320621727, -218.7422906775180138 ) ) ;
#60366 = CARTESIAN_POINT ( 'NONE',  ( -102.5173452166442303, -284.9223813039850484, -229.3594681159061111 ) ) ;
#60367 = CARTESIAN_POINT ( 'NONE',  ( 37.24682703375449222, -277.5838526821655705, -274.3765271141187441 ) ) ;
#60368 = CARTESIAN_POINT ( 'NONE',  ( -66.73259335456813801, -282.2409125996175590, -337.6302913085501700 ) ) ;
#60369 = CARTESIAN_POINT ( 'NONE',  ( 32.01976943006615528, -285.1782093018072715, -241.6948677089157798 ) ) ;
#60370 = CARTESIAN_POINT ( 'NONE',  ( -28.76478048777695662, -275.0842267364463964, -345.6915977970836025 ) ) ;
#60371 = FACE_OUTER_BOUND ( 'NONE', #68899, .T. ) ;
#60372 = CARTESIAN_POINT ( 'NONE',  ( -99.08639726049293017, -283.5193809196402412, -309.5145271514999195 ) ) ;
#60373 = CARTESIAN_POINT ( 'NONE',  ( -111.3513979208076279, -280.0065270791583885, -250.5475088318775363 ) ) ;
#60374 = CARTESIAN_POINT ( 'NONE',  ( 16.14386378315460746, -285.8476498692041332, -215.2964771897490266 ) ) ;
#60375 = CARTESIAN_POINT ( 'NONE',  ( 33.32084354231822942, -295.6000628705302802, -292.3788139522815186 ) ) ;
#60376 = CARTESIAN_POINT ( 'NONE',  ( 12.20010765938192598, -277.9761194971094938, -328.2580064537045814 ) ) ;
#60377 = CARTESIAN_POINT ( 'NONE',  ( 23.23206548785715242, -276.2393255405116861, -223.6052599135365426 ) ) ;
#60378 = CARTESIAN_POINT ( 'NONE',  ( -29.71553516543211160, -276.7863686243386496, -343.0125858697768422 ) ) ;
#60379 = CARTESIAN_POINT ( 'NONE',  ( -101.4809558736667867, -299.0709051326151098, -231.7092294700630930 ) ) ;
#60380 = CARTESIAN_POINT ( 'NONE',  ( 31.09153117124195731, -285.9510332009285776, -300.7702923337593006 ) ) ;
#60381 = CARTESIAN_POINT ( 'NONE',  ( -84.65186673030201803, -291.2913822761420306, -330.1627423075444199 ) ) ;
#60382 = CARTESIAN_POINT ( 'NONE',  ( 16.37632526507976038, -293.1865005834794147, -320.2469859380777848 ) ) ;
#60383 = VERTEX_POINT ( 'NONE', #33074 ) ;
#60384 = CARTESIAN_POINT ( 'NONE',  ( -52.36997697598155810, -291.5212123210685604, -198.8512544192556390 ) ) ;
#60385 = ORIENTED_EDGE ( 'NONE', *, *, #49429, .T. ) ;
#60386 = CARTESIAN_POINT ( 'NONE',  ( -93.35757527685545654, -290.9139143489872481, -322.8181126954419256 ) ) ;
#60387 = CARTESIAN_POINT ( 'NONE',  ( -100.9045231218293139, -279.6973710432708913, -234.2548830501746693 ) ) ;
#60388 = EDGE_CURVE ( 'NONE', #28948, #10184, #65176, .T. ) ;
#60389 = CARTESIAN_POINT ( 'NONE',  ( -103.5758760150832245, -295.9787427896730492, -231.5973881383107198 ) ) ;
#60390 = CARTESIAN_POINT ( 'NONE',  ( 32.77533583169434195, -288.6073964738947097, -301.9350638001409379 ) ) ;
#60391 = CARTESIAN_POINT ( 'NONE',  ( -14.95434048996155596, -289.1032855208179058, -344.0684021427582593 ) ) ;
#60392 = CARTESIAN_POINT ( 'NONE',  ( -110.0159010472469276, -284.9857822643265877, -262.7520650954139114 ) ) ;
#60393 = CARTESIAN_POINT ( 'NONE',  ( 160.9517679153581753, 220.5049154629363102, -205.2241752943726283 ) ) ;
#60394 = CARTESIAN_POINT ( 'NONE',  ( 83.03165031430961562, 83.43481754666375139, -300.8253819011565042 ) ) ;
#60395 = CARTESIAN_POINT ( 'NONE',  ( -31.26167726347551223, -124.5763668223686835, -360.4898096339886706 ) ) ;
#60396 = CARTESIAN_POINT ( 'NONE',  ( 17.54962551842718099, -275.4386829101774197, -318.7488484137036266 ) ) ;
#60397 = CARTESIAN_POINT ( 'NONE',  ( -104.7207959087122333, -277.8588643062657866, -241.4771514175159552 ) ) ;
#60398 = CARTESIAN_POINT ( 'NONE',  ( -83.56400558663789013, -273.1045818380775927, -208.7375805075950836 ) ) ;
#60399 = CARTESIAN_POINT ( 'NONE',  ( -61.42094543554144792, -183.6680788050960302, -359.7854877795325592 ) ) ;
#60400 = CARTESIAN_POINT ( 'NONE',  ( -62.26129571335676616, -276.0543080632585884, -342.7517924108050238 ) ) ;
#60401 = EDGE_LOOP ( 'NONE', ( #14078, #48006, #88344, #74016 ) ) ;
#60402 = CARTESIAN_POINT ( 'NONE',  ( -88.69987556725860145, -290.2895612397065292, -322.3257815257055654 ) ) ;
#60403 = CARTESIAN_POINT ( 'NONE',  ( -91.52891105552558315, -298.1068700209668236, -215.8826360640291568 ) ) ;
#60404 = CARTESIAN_POINT ( 'NONE',  ( 35.48715543661081995, -286.1029092815344370, -260.1297113658219473 ) ) ;
#60405 = CARTESIAN_POINT ( 'NONE',  ( -76.38812534817202504, -274.1961429040649136, -204.0524023061860532 ) ) ;
#60406 = CARTESIAN_POINT ( 'NONE',  ( -13.00624196479073191, -294.8937557311120941, -339.2386854501556854 ) ) ;
#60407 = VERTEX_POINT ( 'NONE', #63397 ) ;
#60408 = CARTESIAN_POINT ( 'NONE',  ( -34.32366762088548739, -278.9346321755835447, -345.8608244721069696 ) ) ;
#60409 = CARTESIAN_POINT ( 'NONE',  ( 37.48705065781805246, -281.2844285935266839, -288.3110075054955814 ) ) ;
#60410 = CARTESIAN_POINT ( 'NONE',  ( -79.24275955927753046, -280.5513155769745595, -210.2069220239609990 ) ) ;
#60411 = CARTESIAN_POINT ( 'NONE',  ( -104.0748209470628751, -279.8357202494831881, -306.7020673000677675 ) ) ;
#60412 = CARTESIAN_POINT ( 'NONE',  ( -107.8543212321808369, -271.3150099633287482, -248.7697013048455688 ) ) ;
#60413 = CARTESIAN_POINT ( 'NONE',  ( 151.0528680457204018, 20.99319481056665992, -6.529293081333598536 ) ) ;
#60414 = CARTESIAN_POINT ( 'NONE',  ( -81.28957079212877090, -279.6026526462124480, -212.0088393225276207 ) ) ;
#60415 = CARTESIAN_POINT ( 'NONE',  ( -99.44260204667226333, -273.9578133151052270, -225.0220549198278945 ) ) ;
#60416 = CARTESIAN_POINT ( 'NONE',  ( -101.0343693207089757, -275.0841720468228573, -230.7600505899964958 ) ) ;
#60417 = CARTESIAN_POINT ( 'NONE',  ( 16.52685502746049906, -274.8796504516705568, -324.6270949286655991 ) ) ;
#60418 = CARTESIAN_POINT ( 'NONE',  ( 200.6103193995254230, 275.5000000000000568, -2.464576988612312114 ) ) ;
#60419 = CARTESIAN_POINT ( 'NONE',  ( -110.1325230367951633, -289.8461273554763125, -263.0059954806920928 ) ) ;
#60420 = CARTESIAN_POINT ( 'NONE',  ( -113.4996134851687373, -283.7627389567925320, -281.3810550041005172 ) ) ;
#60421 = CARTESIAN_POINT ( 'NONE',  ( 27.35534310518245604, -279.3072619147211526, -234.4130080426462825 ) ) ;
#60423 = CARTESIAN_POINT ( 'NONE',  ( -109.7608409365407169, -282.8555170516749513, -253.0789295292640304 ) ) ;
#60422 = CARTESIAN_POINT ( 'NONE',  ( 36.29217619228348468, -280.1396761020107533, -271.3395607405268493 ) ) ;
#60425 = CARTESIAN_POINT ( 'NONE',  ( -73.73857301142604115, -291.5354534251313225, -335.9520805877830867 ) ) ;
#60424 = AXIS2_PLACEMENT_3D ( 'NONE', #88601, #38412, #23749 ) ;
#60426 = CARTESIAN_POINT ( 'NONE',  ( 34.72118241597770094, -282.5735851738255633, -256.3640232395841849 ) ) ;
#60427 = CARTESIAN_POINT ( 'NONE',  ( -49.16145522619329711, -155.7821930437820299, -366.3065075751858330 ) ) ;
#60428 = CARTESIAN_POINT ( 'NONE',  ( 8.708969109741483194, -280.8325290187318615, -331.0717124137480596 ) ) ;
#60429 = CARTESIAN_POINT ( 'NONE',  ( 24.86744961748311766, -296.1189489540585100, -312.2541047099462048 ) ) ;
#60430 = CARTESIAN_POINT ( 'NONE',  ( -112.7090258089518642, -276.9197754974242685, -260.2797850532599568 ) ) ;
#60431 = CIRCLE ( 'NONE', #33240, 2.999999999999997780 ) ;
#60432 = CARTESIAN_POINT ( 'NONE',  ( -96.17010578136677168, -278.5959504278434338, -313.7769278729720668 ) ) ;
#60433 = CARTESIAN_POINT ( 'NONE',  ( -99.87933577908189875, -285.9889349030044627, -312.1566534656125214 ) ) ;
#60434 = EDGE_CURVE ( 'NONE', #85445, #64930, #48199, .T. ) ;
#60435 = EDGE_CURVE ( 'NONE', #9799, #31408, #56758, .T. ) ;
#60436 = CARTESIAN_POINT ( 'NONE',  ( 222.4306832106270804, -141.7221692137691775, -21.50000000000000000 ) ) ;
#60437 = CARTESIAN_POINT ( 'NONE',  ( -19.74628914275245251, -294.1966729846561748, -196.8245676715132220 ) ) ;
#60438 = CARTESIAN_POINT ( 'NONE',  ( 30.96558841734766787, -273.9582843052109524, -301.3306994664233684 ) ) ;
#60439 = CARTESIAN_POINT ( 'NONE',  ( -18.21232186337783077, -285.4896455832965216, -195.8868729565939191 ) ) ;
#60440 = CARTESIAN_POINT ( 'NONE',  ( -98.95633730131135053, -289.5104028974135986, -229.6471909792298050 ) ) ;
#60441 = CARTESIAN_POINT ( 'NONE',  ( -48.18343439343216517, -260.0909709188723014, -439.4475977827055999 ) ) ;
#60442 = CARTESIAN_POINT ( 'NONE',  ( 17.79418301199583397, -274.9264242473320792, -318.9730797678557224 ) ) ;
#60443 = CARTESIAN_POINT ( 'NONE',  ( -69.06636681671103872, -293.6134082483695238, -337.4899922149833742 ) ) ;
#60444 = CARTESIAN_POINT ( 'NONE',  ( -106.4909477400585587, -291.5380246971271845, -295.2533865042721573 ) ) ;
#60445 = DIRECTION ( 'NONE',  ( 0.000000000000000000, 1.000000000000000000, 0.000000000000000000 ) ) ;
#60446 = FACE_OUTER_BOUND ( 'NONE', #48586, .T. ) ;
#60447 = CARTESIAN_POINT ( 'NONE',  ( 36.75339312711324169, -291.8018109438058900, -252.1231106745921977 ) ) ;
#60448 = CARTESIAN_POINT ( 'NONE',  ( 34.15862023356043409, -288.9130158438732678, -252.0305447312458114 ) ) ;
#60449 = CARTESIAN_POINT ( 'NONE',  ( -18.00412063822193787, -287.0460320457614216, -343.8460282081819628 ) ) ;
#60450 = CARTESIAN_POINT ( 'NONE',  ( 11.51178007031639616, -288.1705333175712553, -215.2589294679796126 ) ) ;
#60451 = CARTESIAN_POINT ( 'NONE',  ( 208.6208076322478746, 32.98517505407394168, 10.00000000000000000 ) ) ;
#60452 = CARTESIAN_POINT ( 'NONE',  ( 27.79726307608590119, -287.9020858653212258, -236.9400331837324529 ) ) ;
#60453 = CARTESIAN_POINT ( 'NONE',  ( -66.26921147229691655, -297.4088277195949104, -339.9566630169336463 ) ) ;
#60454 = CARTESIAN_POINT ( 'NONE',  ( 200.3186454232214828, 249.5000000000000568, -3.421094783296257713 ) ) ;
#60455 = CARTESIAN_POINT ( 'NONE',  ( -7.511988127940834481, -287.6395739469902537, -199.7484213841595704 ) ) ;
#60456 = CARTESIAN_POINT ( 'NONE',  ( -59.27089505442766892, -275.4136943288603447, -342.6689640691782301 ) ) ;
#60457 = CARTESIAN_POINT ( 'NONE',  ( -54.12250354081604087, -277.5950956193195225, -345.5432937424280340 ) ) ;
#60458 = CARTESIAN_POINT ( 'NONE',  ( -69.94955670522723779, -279.3010920102036039, -200.6153053965879280 ) ) ;
#60459 = CARTESIAN_POINT ( 'NONE',  ( -40.61477191305175438, -299.9907085589559870, -195.7752767430148140 ) ) ;
#60460 = CARTESIAN_POINT ( 'NONE',  ( -99.75775605391878287, -283.1138997041495031, -228.7770271374152458 ) ) ;
#60461 = CARTESIAN_POINT ( 'NONE',  ( -48.18343439339134449, -281.1255779508778119, -502.6442049081570644 ) ) ;
#60462 = CARTESIAN_POINT ( 'NONE',  ( -70.26716429366889827, -277.7531422142660062, -203.8129948819625383 ) ) ;
#60463 = CARTESIAN_POINT ( 'NONE',  ( -99.76894582009430223, -281.9892592119396113, -312.0216398064575856 ) ) ;
#60464 = CYLINDRICAL_SURFACE ( 'NONE', #54791, 1.000000000000000888 ) ;
#60465 = CARTESIAN_POINT ( 'NONE',  ( 5.466182630333113579, -274.9638351995419043, -333.5290918702791600 ) ) ;
#60466 = CARTESIAN_POINT ( 'NONE',  ( -53.28065189791139744, -296.7802625684204259, -342.3625864068833948 ) ) ;
#60467 = CARTESIAN_POINT ( 'NONE',  ( 17.59520904227672844, -281.2098279357848583, -323.9479973300236111 ) ) ;
#60468 = CARTESIAN_POINT ( 'NONE',  ( -95.48315923168142660, -298.1180668606017434, -225.8100260978594065 ) ) ;
#60469 = CARTESIAN_POINT ( 'NONE',  ( -93.31347934851625325, -298.5835879158189528, -218.1258116344050393 ) ) ;
#60470 = CARTESIAN_POINT ( 'NONE',  ( -74.28041603919683666, -273.2135572696998338, -207.3135097928088726 ) ) ;
#60471 = CARTESIAN_POINT ( 'NONE',  ( 34.26366238025857314, -295.8400433992657668, -292.6696972553274918 ) ) ;
#60472 = CARTESIAN_POINT ( 'NONE',  ( 33.85861635838831774, -287.3447010272027455, -240.9043486338368041 ) ) ;
#60473 = CARTESIAN_POINT ( 'NONE',  ( -109.1729696449280027, -276.9344563478626355, -246.7520387146150256 ) ) ;
#60474 = CARTESIAN_POINT ( 'NONE',  ( -113.8138157160755810, -290.2673993167886124, -279.8021662227334900 ) ) ;
#60475 = CARTESIAN_POINT ( 'NONE',  ( -18.42424667314170961, -287.8612621802606100, -341.1637006831845156 ) ) ;
#60476 = CARTESIAN_POINT ( 'NONE',  ( 3.085500285982334834, -290.5944646524255859, -207.1280172241680191 ) ) ;
#60477 = ORIENTED_EDGE ( 'NONE', *, *, #46440, .F. ) ;
#60478 = CARTESIAN_POINT ( 'NONE',  ( -32.04911714649202992, -124.5213432794980974, -365.6788127701597659 ) ) ;
#60479 = CARTESIAN_POINT ( 'NONE',  ( 34.06949131471166936, -287.2640519193242881, -285.8609546571488522 ) ) ;
#60480 = LINE ( 'NONE', #43913, #2121 ) ;
#60481 = CARTESIAN_POINT ( 'NONE',  ( -79.02188655731423239, -284.5408484617651084, -334.8249238877208427 ) ) ;
#60482 = CARTESIAN_POINT ( 'NONE',  ( -30.70562566366761814, -291.1927188127653494, -193.8311861543629391 ) ) ;
#60483 = CARTESIAN_POINT ( 'NONE',  ( 30.64661842002393399, -283.3224618116423130, -305.4451145117475335 ) ) ;
#60484 = CARTESIAN_POINT ( 'NONE',  ( -65.31765963758300586, -283.2615883188624366, -337.8013115896732756 ) ) ;
#60485 = CARTESIAN_POINT ( 'NONE',  ( -114.2338118077027218, -296.4898922198067908, -275.3393729434181978 ) ) ;
#60486 = CARTESIAN_POINT ( 'NONE',  ( 32.52544030834806676, -276.5648781178616105, -247.3978271721397846 ) ) ;
#60487 = CARTESIAN_POINT ( 'NONE',  ( 35.25317974580958236, -291.3474700368367394, -252.9331715136766547 ) ) ;
#60488 = CARTESIAN_POINT ( 'NONE',  ( 30.54791512914200524, -273.9736478377423623, -242.3326003459168874 ) ) ;
#60489 = VERTEX_POINT ( 'NONE', #4661 ) ;
#60490 = DIRECTION ( 'NONE',  ( 0.6056179655966478226, -0.7957555401921982963, -0.000000000000000000 ) ) ;
#60491 = CARTESIAN_POINT ( 'NONE',  ( 3.211412914798389640, -288.5218311975210099, -207.9370904057302596 ) ) ;
#60492 = CARTESIAN_POINT ( 'NONE',  ( -27.77271544623243571, -296.0131518667982391, -346.5057671648525002 ) ) ;
#60493 = CARTESIAN_POINT ( 'NONE',  ( -101.8572910434111805, -284.7344842269143896, -304.8436945102615141 ) ) ;
#60494 = CARTESIAN_POINT ( 'NONE',  ( 30.32996426721521033, -275.0820113036388079, -306.7137162957004648 ) ) ;
#60495 = CARTESIAN_POINT ( 'NONE',  ( 39.33879950311789031, -294.1311753769712141, -264.5806541041093851 ) ) ;
#60496 = CARTESIAN_POINT ( 'NONE',  ( 36.29816829439095471, -285.9188744056791620, -288.2336879446320381 ) ) ;
#60497 = AXIS2_PLACEMENT_3D ( 'NONE', #21337, #49743, #63989 ) ;
#60498 = CARTESIAN_POINT ( 'NONE',  ( 1.762351128586354454, -294.8772926592548060, -336.6681120844520478 ) ) ;
#60499 = CARTESIAN_POINT ( 'NONE',  ( -86.74056144057361450, -290.0948930024592300, -324.2055395784946654 ) ) ;
#60500 = CARTESIAN_POINT ( 'NONE',  ( 196.0143093133015384, 73.40565171261609123, 11.99999999999998757 ) ) ;
#60501 = LINE ( 'NONE', #89817, #58435 ) ;
#60502 = CARTESIAN_POINT ( 'NONE',  ( -88.12805157378475940, -229.8124237020200837, -344.5111176630173304 ) ) ;
#60503 = VECTOR ( 'NONE', #7522, 1000.000000000000000 ) ;
#60504 = CARTESIAN_POINT ( 'NONE',  ( -66.93817202083411644, -287.1913513824442248, -200.0279351660444718 ) ) ;
#60505 = CARTESIAN_POINT ( 'NONE',  ( 40.65961533371913106, -278.8380690714489560, -252.5904736702033802 ) ) ;
#60506 = EDGE_LOOP ( 'NONE', ( #8650, #19852, #86083, #58627 ) ) ;
#60507 = CARTESIAN_POINT ( 'NONE',  ( -42.97031193815468697, -282.0450455850189542, -343.5041302086287374 ) ) ;
#60508 = CARTESIAN_POINT ( 'NONE',  ( -87.08476619684397235, -277.3894779953670309, -329.1792417500458328 ) ) ;
#60509 = CARTESIAN_POINT ( 'NONE',  ( 37.53760656589423661, -283.5645577198256433, -271.3122625095609237 ) ) ;
#60510 = CARTESIAN_POINT ( 'NONE',  ( -20.05301036732419462, -109.6085418338271325, -361.2089085121472181 ) ) ;
#60511 = CARTESIAN_POINT ( 'NONE',  ( -65.05553085888470832, -281.9819505822722476, -341.5830082621079669 ) ) ;
#60512 = CARTESIAN_POINT ( 'NONE',  ( 37.32636870389302430, -285.5455533740810097, -268.2914573979493866 ) ) ;
#60513 = CARTESIAN_POINT ( 'NONE',  ( -67.07311219661875157, -275.5269561293563925, -200.6736110778851128 ) ) ;
#60514 = CARTESIAN_POINT ( 'NONE',  ( -63.58524729297759848, -295.8958775393900851, -338.6002356537047149 ) ) ;
#60515 = CARTESIAN_POINT ( 'NONE',  ( 33.78970379422997183, -291.9946186084454212, -251.8795905768408829 ) ) ;
#60516 = CARTESIAN_POINT ( 'NONE',  ( -108.4216000602299061, -279.5769834915836896, -241.0189876586613593 ) ) ;
#60517 = CARTESIAN_POINT ( 'NONE',  ( -24.32960295472098267, -276.8815240205642567, -342.2435184127699586 ) ) ;
#60518 = CARTESIAN_POINT ( 'NONE',  ( 37.28786742031591217, -274.6949080942545720, -288.0789004629479564 ) ) ;
#60519 = CARTESIAN_POINT ( 'NONE',  ( -113.5000000000000568, -218.8335761803644743, -447.4016117689005796 ) ) ;
#60520 = CARTESIAN_POINT ( 'NONE',  ( 23.05401909177898645, -272.9452268401891502, -225.8724155096909101 ) ) ;
#60521 = CARTESIAN_POINT ( 'NONE',  ( 33.90865761725102345, -295.3298246709218802, -297.9653352845036807 ) ) ;
#60522 = LINE ( 'NONE', #89358, #74773 ) ;
#60523 = DIRECTION ( 'NONE',  ( -0.000000000000000000, -1.000000000000000000, -0.000000000000000000 ) ) ;
#60524 = CARTESIAN_POINT ( 'NONE',  ( -110.3034882577515106, -285.7320522267272622, -262.7314890404674088 ) ) ;
#60525 = CARTESIAN_POINT ( 'NONE',  ( -31.68900807216368065, -284.7418921529511522, -346.1503361395804177 ) ) ;
#60526 = CARTESIAN_POINT ( 'NONE',  ( -42.67329689383888081, -285.3317287527656845, -197.4412272059102236 ) ) ;
#60527 = CARTESIAN_POINT ( 'NONE',  ( -73.24887588890946688, -275.9365228485140165, -334.8513535008983126 ) ) ;
#60528 = CARTESIAN_POINT ( 'NONE',  ( 16.74174465225318897, -284.1330837846441568, -321.2865270618526665 ) ) ;
#60529 = CARTESIAN_POINT ( 'NONE',  ( -104.9148116344691317, -276.6388864316090803, -299.8928449021976803 ) ) ;
#60530 = CARTESIAN_POINT ( 'NONE',  ( 1.044953632588694781, -277.6067450453736569, -332.8762833897277460 ) ) ;
#60531 = CARTESIAN_POINT ( 'NONE',  ( 207.7761861081325776, 35.69891260691533574, 14.41714557868295188 ) ) ;
#60532 = CARTESIAN_POINT ( 'NONE',  ( -103.2782961899313108, -279.8716610418654795, -230.8048308979910246 ) ) ;
#60533 = CARTESIAN_POINT ( 'NONE',  ( 33.11407624544944639, -281.6499648306585186, -239.4497854544152915 ) ) ;
#60534 = EDGE_LOOP ( 'NONE', ( #47220, #69587, #21164, #8202 ) ) ;
#60535 = EDGE_LOOP ( 'NONE', ( #81816, #28271, #34642 ) ) ;
#60536 = CARTESIAN_POINT ( 'NONE',  ( 199.3270723581584321, 16.88338937786638994, -10.34008960743408245 ) ) ;
#60537 = CARTESIAN_POINT ( 'NONE',  ( 37.45942772654314723, -289.5697300886031940, -282.7263006920437647 ) ) ;
#60538 = CARTESIAN_POINT ( 'NONE',  ( -96.22421295610264735, -296.3568010194084081, -226.9181863685478220 ) ) ;
#60539 = CARTESIAN_POINT ( 'NONE',  ( -70.60250078612546076, -288.8277924496885021, -339.7083474993643222 ) ) ;
#60540 = CARTESIAN_POINT ( 'NONE',  ( 33.64818717020367700, -285.5182193394552428, -249.3781218782071392 ) ) ;
#60542 = CARTESIAN_POINT ( 'NONE',  ( -110.4232096375316701, -288.6386401632899492, -282.1485428781422797 ) ) ;
#60541 = CARTESIAN_POINT ( 'NONE',  ( 36.03794416984193560, -286.2078452335103975, -276.5488024868615753 ) ) ;
#60543 = CARTESIAN_POINT ( 'NONE',  ( -54.86593816862129813, -287.0270325313683770, -199.0341927750866375 ) ) ;
#60544 = CARTESIAN_POINT ( 'NONE',  ( -56.43998825413677167, -275.2979696075724405, -342.9423686592047034 ) ) ;
#60545 = CARTESIAN_POINT ( 'NONE',  ( -2.188096729433388177, -286.9945401694358225, -337.9678083718283688 ) ) ;
#60546 = CARTESIAN_POINT ( 'NONE',  ( -5.643018050268392649, -288.4691924920522865, -202.3891075114036084 ) ) ;
#60547 = CARTESIAN_POINT ( 'NONE',  ( -45.84430722351293497, -287.1594166389476186, -345.0972097400667167 ) ) ;
#60548 = CARTESIAN_POINT ( 'NONE',  ( -36.17780863960586402, -283.9784588265530942, -343.5871639324492435 ) ) ;
#60549 = CARTESIAN_POINT ( 'NONE',  ( -104.8553635282622025, -292.1162448210491220, -303.5237687887135962 ) ) ;
#60550 = CYLINDRICAL_SURFACE ( 'NONE', #79111, 5.568361562975243650 ) ;
#60551 = EDGE_CURVE ( 'NONE', #57747, #69256, #32093, .T. ) ;
#60552 = CARTESIAN_POINT ( 'NONE',  ( 155.0589890788380387, 20.95955078618535694, -14.77888609070628334 ) ) ;
#60553 = CARTESIAN_POINT ( 'NONE',  ( -99.57872012755365176, -299.0489784469172037, -227.4913452869886612 ) ) ;
#60554 = CARTESIAN_POINT ( 'NONE',  ( -46.46648324612441883, -279.1306978598997262, -197.7196833028347953 ) ) ;
#60555 = CARTESIAN_POINT ( 'NONE',  ( 36.30282800205460347, -279.3688671705141928, -256.0988322388138272 ) ) ;
#60556 = CARTESIAN_POINT ( 'NONE',  ( 39.55003942692350449, -292.7488089563902918, -270.3202706118128731 ) ) ;
#60557 = CARTESIAN_POINT ( 'NONE',  ( -92.76226730721126046, -271.4833460967124097, -221.3046734687274864 ) ) ;
#60558 = CARTESIAN_POINT ( 'NONE',  ( 24.53666851091549361, -280.7829715364869116, -310.1070178101709303 ) ) ;
#60559 = CARTESIAN_POINT ( 'NONE',  ( -37.84353444839104696, -275.1382964924279690, -344.8121285912944245 ) ) ;
#60560 = CARTESIAN_POINT ( 'NONE',  ( -88.83551304192404530, -297.1087385594521493, -322.8695417592547301 ) ) ;
#60561 = CYLINDRICAL_SURFACE ( 'NONE', #33646, 204.9779373800640485 ) ;
#60562 = CARTESIAN_POINT ( 'NONE',  ( -15.04264616131752064, -296.8064226372752046, -194.0600888125450467 ) ) ;
#60563 = CARTESIAN_POINT ( 'NONE',  ( -44.71984174023356218, -293.3840368724249288, -346.0414434558113044 ) ) ;
#60564 = CARTESIAN_POINT ( 'NONE',  ( 26.73879230165602650, -294.4848933392556773, -234.0761079441385277 ) ) ;
#60565 = DIRECTION ( 'NONE',  ( 0.9693563597868444237, 0.2456588035076248955, 1.780678744869133453E-16 ) ) ;
#60566 = CARTESIAN_POINT ( 'NONE',  ( 35.58620969732011474, -294.4318767629111449, -276.2024958275785593 ) ) ;
#60568 = ADVANCED_FACE ( 'NONE', ( #42503 ), #92696, .T. ) ;
#60567 = CIRCLE ( 'NONE', #1537, 4.000000000000003553 ) ;
#60569 = CARTESIAN_POINT ( 'NONE',  ( 152.4536156746142410, 250.5000000000000568, 12.49999999999999289 ) ) ;
#60571 = CARTESIAN_POINT ( 'NONE',  ( 17.08056822218696880, -294.2483305425531626, -319.0340156440103669 ) ) ;
#60570 = CARTESIAN_POINT ( 'NONE',  ( -63.36810191647938950, -281.4097083275216278, -341.0791016373691491 ) ) ;
#60572 = CARTESIAN_POINT ( 'NONE',  ( 2.094138187946521512, -282.5393889787492299, -336.4959397961259242 ) ) ;
#60573 = CARTESIAN_POINT ( 'NONE',  ( 36.57086068559772940, -283.2715198885970267, -254.6070352888611978 ) ) ;
#60574 = AXIS2_PLACEMENT_3D ( 'NONE', #69882, #92573, #13537 ) ;
#60575 = CARTESIAN_POINT ( 'NONE',  ( -40.81126966245135179, -285.6764845111841851, -193.4083124510580092 ) ) ;
#60576 = CARTESIAN_POINT ( 'NONE',  ( -80.56948442246236652, -289.4648332325664910, -209.2125360946509716 ) ) ;
#60577 = CARTESIAN_POINT ( 'NONE',  ( 26.13429704387030483, -280.5945619526020778, -312.7109176932845571 ) ) ;
#60578 = CARTESIAN_POINT ( 'NONE',  ( 0.4364395159697663229, -285.2513440326130763, -207.2616693030522868 ) ) ;
#60579 = CARTESIAN_POINT ( 'NONE',  ( -9.687671272622218055, -287.6195282366902575, -341.8925600049396394 ) ) ;
#60580 = CARTESIAN_POINT ( 'NONE',  ( 180.7287904564219332, 275.5000000000000568, -24.90000000000003411 ) ) ;
#60581 = CARTESIAN_POINT ( 'NONE',  ( -35.61165264579608447, -296.6302519773774407, -344.1534726132274500 ) ) ;
#60582 = CARTESIAN_POINT ( 'NONE',  ( -9.410176537001710528, -278.1194006394584335, -341.4838027099662554 ) ) ;
#60584 = CARTESIAN_POINT ( 'NONE',  ( -83.44780380070754688, -279.0667575865829235, -213.6713462875808602 ) ) ;
#60583 = CARTESIAN_POINT ( 'NONE',  ( -32.15151727363704737, -293.0071247618849384, -345.5503410003860267 ) ) ;
#60585 = CARTESIAN_POINT ( 'NONE',  ( 17.48811442845540043, -292.9756695827549038, -216.2241180179798050 ) ) ;
#60586 = CARTESIAN_POINT ( 'NONE',  ( -96.43857024671335409, -283.2744289753583757, -223.2774249978915861 ) ) ;
#60587 = CARTESIAN_POINT ( 'NONE',  ( -17.85241623260458610, -278.8009893531771013, -342.7846532393796224 ) ) ;
#60588 = CARTESIAN_POINT ( 'NONE',  ( -7.904696112840743361, -293.7154938753760121, -337.4334528087462672 ) ) ;
#60589 = CARTESIAN_POINT ( 'NONE',  ( -90.84577750382673855, -271.2949341975801758, -217.5658328722028898 ) ) ;
#60590 = ORIENTED_EDGE ( 'NONE', *, *, #76146, .T. ) ;
#60591 = CARTESIAN_POINT ( 'NONE',  ( 200.2349812190172713, 66.43136063442170780, -7.741079165001072404 ) ) ;
#60592 = CARTESIAN_POINT ( 'NONE',  ( -3.626719288247383322, -282.4791681233259624, -203.7500174577812118 ) ) ;
#60593 = CARTESIAN_POINT ( 'NONE',  ( -15.58047257130720276, -294.2705986754926926, -340.1598514669502720 ) ) ;
#60594 = CYLINDRICAL_SURFACE ( 'NONE', #47366, 7.500000000000007105 ) ;
#60595 = CARTESIAN_POINT ( 'NONE',  ( -106.6379572354042296, -270.4809262143061233, -236.9535640164627353 ) ) ;
#60596 = CARTESIAN_POINT ( 'NONE',  ( -54.53078975202447509, -296.8952345963784865, -195.5456422427284906 ) ) ;
#60597 = CARTESIAN_POINT ( 'NONE',  ( 5.296460762930212951, -289.8033955440743625, -333.8850151207809063 ) ) ;
#60598 = CARTESIAN_POINT ( 'NONE',  ( -23.78725754470517018, -288.7075739331700674, -342.1434033988199985 ) ) ;
#60599 = CARTESIAN_POINT ( 'NONE',  ( -24.77703228413670189, -281.7354919470448067, -197.7468158597859826 ) ) ;
#60600 = CARTESIAN_POINT ( 'NONE',  ( -80.33463390192298448, -299.2208312046917058, -210.1151085145808679 ) ) ;
#60601 = CARTESIAN_POINT ( 'NONE',  ( -16.79594119653510376, -279.1184445013944924, -199.8983455861094001 ) ) ;
#60602 = VERTEX_POINT ( 'NONE', #26912 ) ;
#60603 = CARTESIAN_POINT ( 'NONE',  ( -57.38012185026543932, -297.4672460197297141, -195.9808532764782001 ) ) ;
#60604 = CARTESIAN_POINT ( 'NONE',  ( -91.82957718802086333, -293.1875909031014658, -219.6235749595483355 ) ) ;
#60605 = DIRECTION ( 'NONE',  ( 0.000000000000000000, 1.000000000000000000, 0.000000000000000000 ) ) ;
#60606 = CARTESIAN_POINT ( 'NONE',  ( -99.80300282278302859, -291.7259055380560540, -232.3811451849066430 ) ) ;
#60607 = LINE ( 'NONE', #30316, #28535 ) ;
#60608 = CARTESIAN_POINT ( 'NONE',  ( 20.38496360662549733, -291.0192152930006841, -221.2705473242575067 ) ) ;
#60609 = CARTESIAN_POINT ( 'NONE',  ( -106.3624677003556229, -272.3781973416595292, -246.4002731446144026 ) ) ;
#60610 = DIRECTION ( 'NONE',  ( 0.000000000000000000, -0.7071067811865364705, -0.7071067811865584529 ) ) ;
#60611 = CARTESIAN_POINT ( 'NONE',  ( 195.5045040238821059, 26.76854409577648397, 14.93905022940502469 ) ) ;
#60612 = CARTESIAN_POINT ( 'NONE',  ( -113.6961392413176952, -292.0611784968479014, -271.2402657328650548 ) ) ;
#60613 = CARTESIAN_POINT ( 'NONE',  ( -72.08107566293803359, -288.1233781216987495, -198.2974183793908196 ) ) ;
#60614 = CARTESIAN_POINT ( 'NONE',  ( 10.17546534086699417, -288.7094029349109405, -212.5498093207402803 ) ) ;
#60615 = CARTESIAN_POINT ( 'NONE',  ( 12.79320847787570692, -272.7529408060775040, -214.7348697397721935 ) ) ;
#60616 = CARTESIAN_POINT ( 'NONE',  ( 27.88677906717059329, -276.9905502895525728, -234.3851046867563070 ) ) ;
#60617 = CARTESIAN_POINT ( 'NONE',  ( 15.92264603349519092, -290.8935415500233717, -218.2851128831837855 ) ) ;
#60618 = CARTESIAN_POINT ( 'NONE',  ( -50.74476704198991683, -281.7431036626027208, -195.7912629784086391 ) ) ;
#60619 = ORIENTED_EDGE ( 'NONE', *, *, #47636, .T. ) ;
#60620 = CARTESIAN_POINT ( 'NONE',  ( 15.89440995821195912, -281.6216598381349741, -320.5321354122337993 ) ) ;
#60621 = CARTESIAN_POINT ( 'NONE',  ( -64.97082253458765422, -278.4842878120849150, -341.9582392192971270 ) ) ;
#60622 = CARTESIAN_POINT ( 'NONE',  ( 36.22271522649956665, -280.0772904032810402, -248.9532191077369419 ) ) ;
#60623 = CARTESIAN_POINT ( 'NONE',  ( -84.15502384080009790, -218.1365120809277869, -349.3283341728729852 ) ) ;
#60624 = CARTESIAN_POINT ( 'NONE',  ( 36.27125077342100212, -276.7678838039670950, -292.1779974731985021 ) ) ;
#60625 = DIRECTION ( 'NONE',  ( -1.000000000000000000, 0.000000000000000000, 0.000000000000000000 ) ) ;
#60626 = CARTESIAN_POINT ( 'NONE',  ( -5.422082409212579890, -275.9846430709311562, -201.0513368564109840 ) ) ;
#60627 = CARTESIAN_POINT ( 'NONE',  ( -107.3417001280813565, -275.0519495502701943, -270.3929463913696054 ) ) ;
#60628 = EDGE_LOOP ( 'NONE', ( #67269, #54080, #40528, #11678 ) ) ;
#60629 = ORIENTED_EDGE ( 'NONE', *, *, #92477, .F. ) ;
#60630 = AXIS2_PLACEMENT_3D ( 'NONE', #89550, #12257, #62951 ) ;
#60631 = CARTESIAN_POINT ( 'NONE',  ( -63.92019387127945151, -290.4866310520984598, -338.7368989656019949 ) ) ;
#60632 = CARTESIAN_POINT ( 'NONE',  ( -79.95356955140357513, -291.3797356019202880, -333.3389183249099119 ) ) ;
#60633 = CARTESIAN_POINT ( 'NONE',  ( -5.990401590645244134, -291.8240484974339211, -204.3095332323871673 ) ) ;
#60634 = CARTESIAN_POINT ( 'NONE',  ( 0.2591966413363832600, -286.0466692120098742, -203.2215746124874443 ) ) ;
#60635 = CARTESIAN_POINT ( 'NONE',  ( 200.3691939013025092, 25.16710152838963666, 9.000000000000000000 ) ) ;
#60636 = CARTESIAN_POINT ( 'NONE',  ( -34.83960815200947536, -281.4201037312869289, -344.1312666608919244 ) ) ;
#60637 = CARTESIAN_POINT ( 'NONE',  ( 30.56438278280192122, -289.8109883746771516, -300.4825694039474797 ) ) ;
#60638 = CARTESIAN_POINT ( 'NONE',  ( -15.94955111743373166, -281.2502617265599838, -340.8812123653286790 ) ) ;
#60639 = CARTESIAN_POINT ( 'NONE',  ( 13.66539583930616608, -282.0998886256161882, -217.3797276448290461 ) ) ;
#60640 = CARTESIAN_POINT ( 'NONE',  ( 35.62163048327094828, -288.1904000803211829, -246.3338642848808888 ) ) ;
#60641 = CARTESIAN_POINT ( 'NONE',  ( -109.5519304134525811, -278.8979240095968635, -281.4818681303011658 ) ) ;
#60642 = CARTESIAN_POINT ( 'NONE',  ( -34.95731865161447871, -290.8763717674611371, -193.7822246757606308 ) ) ;
#60643 = CARTESIAN_POINT ( 'NONE',  ( -3.569570110258568629, -287.2893896940269087, -201.3277687750509415 ) ) ;
#60644 = CARTESIAN_POINT ( 'NONE',  ( -21.00315195154998094, -286.7487581783250334, -195.1774844807272302 ) ) ;
#60645 = CARTESIAN_POINT ( 'NONE',  ( -45.63736041356587947, -283.3267614128931200, -342.9392243435241880 ) ) ;
#60646 = ORIENTED_EDGE ( 'NONE', *, *, #88318, .F. ) ;
#60647 = DIRECTION ( 'NONE',  ( 0.000000000000000000, 1.000000000000000000, 0.000000000000000000 ) ) ;
#60648 = CARTESIAN_POINT ( 'NONE',  ( -30.82747045714212675, -293.9939348471471590, -194.8249673091273166 ) ) ;
#60649 = CARTESIAN_POINT ( 'NONE',  ( 36.23454281326554849, -291.9718552417300543, -249.3411071071053868 ) ) ;
#60650 = CARTESIAN_POINT ( 'NONE',  ( 11.89706470054795240, -275.4068562313950679, -324.6420278999225957 ) ) ;
#60651 = ADVANCED_FACE ( 'NONE', ( #41565, #70488 ), #85600, .F. ) ;
#60652 = CARTESIAN_POINT ( 'NONE',  ( -113.6725936094580334, -296.0174851816216801, -261.0386994760402786 ) ) ;
#60653 = CARTESIAN_POINT ( 'NONE',  ( 2.632699257351296396, -291.0783868558146423, -208.3914105678887836 ) ) ;
#60654 = CARTESIAN_POINT ( 'NONE',  ( -111.1111930172054656, -294.7060404322562022, -276.9681024101976163 ) ) ;
#60655 = CARTESIAN_POINT ( 'NONE',  ( -84.09370055757085538, -292.5976536416226281, -213.7803707316678867 ) ) ;
#60656 = CARTESIAN_POINT ( 'NONE',  ( -7.155473100384013740, -293.5374214434013993, -203.5552965871385709 ) ) ;
#60657 = FACE_OUTER_BOUND ( 'NONE', #83184, .T. ) ;
#60658 = CARTESIAN_POINT ( 'NONE',  ( 19.95329039137341454, -292.2238954011986607, -319.0161536000966862 ) ) ;
#60659 = CARTESIAN_POINT ( 'NONE',  ( -111.9868657989353125, -298.4522530729223035, -278.1542108845709436 ) ) ;
#60660 = CARTESIAN_POINT ( 'NONE',  ( 21.36927718300752588, -289.1058965491647541, -314.1591588142248952 ) ) ;
#60661 = CARTESIAN_POINT ( 'NONE',  ( -42.66428027571386394, -279.0988923518869456, -345.5281116963840873 ) ) ;
#60662 = CARTESIAN_POINT ( 'NONE',  ( -84.63336088318990846, -276.4818810966186788, -330.6905201133657215 ) ) ;
#60663 = CARTESIAN_POINT ( 'NONE',  ( -70.08082301010752246, -272.9807356821661415, -200.7661047113763857 ) ) ;
#60664 = CARTESIAN_POINT ( 'NONE',  ( -1.761476353488416358, -280.6567830265450993, -335.7619383418527832 ) ) ;
#60665 = CARTESIAN_POINT ( 'NONE',  ( -90.78265971792666278, -276.1943246467036488, -324.7535736170409564 ) ) ;
#60666 = EDGE_CURVE ( 'NONE', #70970, #43675, #13999, .T. ) ;
#60667 = CARTESIAN_POINT ( 'NONE',  ( -106.4566453505326251, -294.9045789936268989, -295.4982061777914737 ) ) ;
#60668 = DIRECTION ( 'NONE',  ( 1.000000000000000000, 0.000000000000000000, 0.000000000000000000 ) ) ;
#60669 = CARTESIAN_POINT ( 'NONE',  ( -106.4054009945861168, -273.5217733763906836, -246.4007780283252487 ) ) ;
#60670 = CARTESIAN_POINT ( 'NONE',  ( 196.9534188175200029, 25.84350552936208700, 12.42857142857142350 ) ) ;
#60672 = CARTESIAN_POINT ( 'NONE',  ( 32.06247581584992901, -275.0832630219227894, -247.5697406013929083 ) ) ;
#60671 = CARTESIAN_POINT ( 'NONE',  ( -96.87598455088541982, -287.9419036202641564, -316.5571760960855272 ) ) ;
#60673 = CARTESIAN_POINT ( 'NONE',  ( -1.800723475625440217, -288.5944098374249052, -338.6680647639055906 ) ) ;
#60674 = CARTESIAN_POINT ( 'NONE',  ( -33.46609864687144409, -300.0803253697694117, -195.0046094052071055 ) ) ;
#60675 = CARTESIAN_POINT ( 'NONE',  ( -111.9287426032308872, -294.4660598388139192, -277.0385069591173419 ) ) ;
#60676 = CARTESIAN_POINT ( 'NONE',  ( -65.20318946247230940, -282.6042898598732336, -341.9846234622050360 ) ) ;
#60677 = CARTESIAN_POINT ( 'NONE',  ( -54.94434090351493438, -282.8906705383787994, 54.50000000000000711 ) ) ;
#60678 = CARTESIAN_POINT ( 'NONE',  ( -40.69529884830035371, -281.0941508278524452, -345.2987983457802557 ) ) ;
#60679 = DIRECTION ( 'NONE',  ( 0.000000000000000000, 0.000000000000000000, 1.000000000000000000 ) ) ;
#60680 = CARTESIAN_POINT ( 'NONE',  ( -110.7342668994143224, -289.3363972647138098, -271.1745344386482657 ) ) ;
#60681 = CARTESIAN_POINT ( 'NONE',  ( -70.79237701084589673, -281.6377308945866389, -336.6468801284265169 ) ) ;
#60682 = CARTESIAN_POINT ( 'NONE',  ( 197.4288403404172243, 41.88980437486004149, 11.72798125285449267 ) ) ;
#60683 = CARTESIAN_POINT ( 'NONE',  ( -57.23711263161519724, -331.8906705383788562, 57.50000000000000711 ) ) ;
#60684 = CARTESIAN_POINT ( 'NONE',  ( -78.32737713689711256, -289.5005245642581144, -207.5504904803935631 ) ) ;
#60685 = CARTESIAN_POINT ( 'NONE',  ( -90.71196182556371923, -274.7983362236321909, -219.5260891830804155 ) ) ;
#60686 = CARTESIAN_POINT ( 'NONE',  ( 13.42915876502997286, -283.5655176203714518, -327.7931232356754094 ) ) ;
#60688 = CARTESIAN_POINT ( 'NONE',  ( -109.8727451829732757, -284.4374211599986211, -279.0583553752116472 ) ) ;
#60687 = CARTESIAN_POINT ( 'NONE',  ( -41.09628269797579492, -272.0852301156956514, -194.8431711031664406 ) ) ;
#60689 = CARTESIAN_POINT ( 'NONE',  ( 35.94243518132184789, -277.0650297401658122, -277.0551771541302628 ) ) ;
#60690 = CARTESIAN_POINT ( 'NONE',  ( -45.91689934074382506, -277.9663590566264020, -343.0690483393344721 ) ) ;
#60691 = CARTESIAN_POINT ( 'NONE',  ( 29.31168984804137523, -284.0073380426781000, -304.7460892699423312 ) ) ;
#60692 = ORIENTED_EDGE ( 'NONE', *, *, #71569, .F. ) ;
#60693 = CARTESIAN_POINT ( 'NONE',  ( 123.4306832106270946, -178.2391364535880882, 0.000000000000000000 ) ) ;
#60694 = CARTESIAN_POINT ( 'NONE',  ( 28.10480402680632750, -293.9171528315736737, -311.0291932777930697 ) ) ;
#60696 = CARTESIAN_POINT ( 'NONE',  ( -19.44538900578974960, -288.2633913686266851, -197.8934089817844608 ) ) ;
#60695 = CIRCLE ( 'NONE', #19863, 5.568361562975243650 ) ;
#60697 = FACE_OUTER_BOUND ( 'NONE', #57032, .T. ) ;
#60698 = CARTESIAN_POINT ( 'NONE',  ( 25.22466315766302358, -284.4094976428775112, -220.5068182859052968 ) ) ;
#60699 = CARTESIAN_POINT ( 'NONE',  ( -112.9086949205890704, -277.5739520403763549, -284.3542396196921231 ) ) ;
#60700 = CARTESIAN_POINT ( 'NONE',  ( 6.057492742986257284, -291.0301712839860215, -207.7276567024939880 ) ) ;
#60701 = CARTESIAN_POINT ( 'NONE',  ( -96.33247147748181760, -286.6863907198519428, -226.1932942912849285 ) ) ;
#60702 = CARTESIAN_POINT ( 'NONE',  ( -43.26616232028376174, -278.8881364826787035, -344.1369592954919199 ) ) ;
#60703 = CARTESIAN_POINT ( 'NONE',  ( -18.34619209592591105, -287.7173918965106054, -196.2944349023662198 ) ) ;
#60704 = CARTESIAN_POINT ( 'NONE',  ( -0.2410931236640105890, -284.5588246236179657, -335.5419864141704238 ) ) ;
#60705 = CARTESIAN_POINT ( 'NONE',  ( 8.242771729229867006, -276.6146646364114758, -332.4840099729999565 ) ) ;
#60706 = CARTESIAN_POINT ( 'NONE',  ( -97.05573908548733186, -277.7329307282209925, -318.9948666897630574 ) ) ;
#60707 = CARTESIAN_POINT ( 'NONE',  ( -35.11783909226129197, -300.0003528430044071, -195.9203753877539782 ) ) ;
#60708 = CARTESIAN_POINT ( 'NONE',  ( 156.4851178187871312, 20.00000000000000000, -15.00000000000000000 ) ) ;
#60709 = CARTESIAN_POINT ( 'NONE',  ( 194.2870706637141325, 39.36132622696000993, 14.58823529411763431 ) ) ;
#60710 = CARTESIAN_POINT ( 'NONE',  ( -36.53280109627711880, -296.2017666697079221, -194.5965636609959404 ) ) ;
#60711 = CARTESIAN_POINT ( 'NONE',  ( 202.9738562182569694, 293.9636489450776367, -44.00000000000000000 ) ) ;
#60712 = CARTESIAN_POINT ( 'NONE',  ( -19.00755205941983661, -276.3173497832154339, -341.0848583818217890 ) ) ;
#60713 = CARTESIAN_POINT ( 'NONE',  ( -87.78648723225141737, -274.5709710616191614, -212.6422327271353083 ) ) ;
#60714 = CARTESIAN_POINT ( 'NONE',  ( 23.56795171037360603, -279.9855614980049836, -223.6188254416905465 ) ) ;
#60715 = CARTESIAN_POINT ( 'NONE',  ( 18.52657235348485898, -288.6296532150673215, -221.8151588811089425 ) ) ;
#60716 = CARTESIAN_POINT ( 'NONE',  ( -95.04440103841686494, -297.3915831473902358, -320.2921310073183463 ) ) ;
#60717 = CARTESIAN_POINT ( 'NONE',  ( -92.40088565864948578, -297.0237916151897366, -323.6198713195057621 ) ) ;
#60718 = CARTESIAN_POINT ( 'NONE',  ( -19.66315597169152696, -294.2800220465041434, -197.5923594514231354 ) ) ;
#60719 = CARTESIAN_POINT ( 'NONE',  ( 23.62145660569067829, -278.9606242160397755, -226.9615563584597453 ) ) ;
#60720 = CARTESIAN_POINT ( 'NONE',  ( 36.86663315238075000, -283.5562919829110911, -276.8528551379662304 ) ) ;
#60721 = CARTESIAN_POINT ( 'NONE',  ( -108.0674115361805718, -294.9361323342087076, -246.9774491519044375 ) ) ;
#60722 = CARTESIAN_POINT ( 'NONE',  ( -101.8521541926661769, -286.6889049307578148, -229.8044695643355624 ) ) ;
#60723 = CARTESIAN_POINT ( 'NONE',  ( 34.82356774758065399, -286.6419270364220893, -283.2607376132246486 ) ) ;
#60724 = CARTESIAN_POINT ( 'NONE',  ( 24.51469319637114452, -280.2928157066955919, -224.6763350482493138 ) ) ;
#60725 = CARTESIAN_POINT ( 'NONE',  ( 86.36035778855256240, 82.03965494544887349, -301.7430877023235212 ) ) ;
#60726 = ORIENTED_EDGE ( 'NONE', *, *, #48544, .F. ) ;
#60727 = CARTESIAN_POINT ( 'NONE',  ( -44.02208616709134503, -285.6320796258899009, -197.6461956547500733 ) ) ;
#60728 = ORIENTED_EDGE ( 'NONE', *, *, #3596, .T. ) ;
#60729 = CARTESIAN_POINT ( 'NONE',  ( -110.8078930676592506, -285.3540441091186040, -292.4114867239314890 ) ) ;
#60730 = CARTESIAN_POINT ( 'NONE',  ( 30.19275627893312119, -275.5117571331371664, -242.4581530986482107 ) ) ;
#60731 = CARTESIAN_POINT ( 'NONE',  ( -37.77941401554981127, -290.9671244651735265, -193.6714777573613446 ) ) ;
#60732 = CARTESIAN_POINT ( 'NONE',  ( 19.71346318239393725, -282.9052419346073179, -321.9950323594325141 ) ) ;
#60733 = CARTESIAN_POINT ( 'NONE',  ( -112.5563778921950586, -280.2346025174884971, -257.4979923012416521 ) ) ;
#60734 = CARTESIAN_POINT ( 'NONE',  ( 32.37504316569854979, -282.3048862137712831, -303.1259566819899760 ) ) ;
#60735 = CARTESIAN_POINT ( 'NONE',  ( -53.28691492658257545, -283.3380690714490697, -200.3538533559491555 ) ) ;
#60736 = CARTESIAN_POINT ( 'NONE',  ( -12.21535056456116841, -91.97447309684723393, -360.1559200363261084 ) ) ;
#60737 = ORIENTED_EDGE ( 'NONE', *, *, #64244, .F. ) ;
#60738 = CARTESIAN_POINT ( 'NONE',  ( 21.47892920326006561, -278.1890651935221968, -316.6436477195902057 ) ) ;
#60739 = CARTESIAN_POINT ( 'NONE',  ( 199.0379451319788870, 289.5412081999082829, -97.41078727901259526 ) ) ;
#60740 = CARTESIAN_POINT ( 'NONE',  ( 36.76975961077297939, -279.6925852846134148, -279.6882258245543653 ) ) ;
#60741 = CARTESIAN_POINT ( 'NONE',  ( -109.3748887871795574, -296.0648016639579510, -257.9067051112525633 ) ) ;
#60742 = CARTESIAN_POINT ( 'NONE',  ( 32.13309633229800255, -292.6343496558510537, -237.1800675261456774 ) ) ;
#60743 = LINE ( 'NONE', #39392, #41480 ) ;
#60745 = CARTESIAN_POINT ( 'NONE',  ( -42.74258219543229842, -287.5211522892533935, -344.0143886667376592 ) ) ;
#60744 = CARTESIAN_POINT ( 'NONE',  ( -43.22612960531466086, -296.5540940438037865, -194.1244600998590499 ) ) ;
#60746 = CARTESIAN_POINT ( 'NONE',  ( 27.29864803117867211, -294.9199669210070738, -233.7529178472987041 ) ) ;
#60747 = CARTESIAN_POINT ( 'NONE',  ( 28.08961680829964891, -288.4143448588559409, -236.7827668650305384 ) ) ;
#60748 = VERTEX_POINT ( 'NONE', #21206 ) ;
#60749 = CARTESIAN_POINT ( 'NONE',  ( 13.11477984448461598, -293.6786324589966739, -212.5081678321506047 ) ) ;
#60750 = CARTESIAN_POINT ( 'NONE',  ( -108.7789107327551079, -284.8417871090486528, -285.7408732046596356 ) ) ;
#60751 = CARTESIAN_POINT ( 'NONE',  ( -34.76056875060747586, -296.8787225071721991, -193.7587024660421662 ) ) ;
#60752 = CARTESIAN_POINT ( 'NONE',  ( 23.84043921676020972, -293.7339629927249689, -223.8539382171424563 ) ) ;
#60753 = CARTESIAN_POINT ( 'NONE',  ( -86.47855275024571142, -291.8833598305113810, -211.0880806614227936 ) ) ;
#60754 = CARTESIAN_POINT ( 'NONE',  ( 7.981603565306609305, -288.5792021865862012, -327.5869700670832572 ) ) ;
#60755 = VERTEX_POINT ( 'NONE', #88386 ) ;
#60756 = CARTESIAN_POINT ( 'NONE',  ( 140.6539576904058606, 250.0000000000000568, 12.00000000000000178 ) ) ;
#60757 = CARTESIAN_POINT ( 'NONE',  ( -40.41427878682304708, -299.8744588190737090, -194.6073536519148206 ) ) ;
#60758 = CARTESIAN_POINT ( 'NONE',  ( -36.92639498832856049, -272.8522061540618324, -193.7463297912194946 ) ) ;
#60759 = CARTESIAN_POINT ( 'NONE',  ( 28.35686650998900760, -281.0493618194070677, -302.8351962049384838 ) ) ;
#60760 = ORIENTED_EDGE ( 'NONE', *, *, #40423, .F. ) ;
#60761 = ADVANCED_FACE ( 'NONE', ( #51011 ), #79898, .T. ) ;
#60762 = CARTESIAN_POINT ( 'NONE',  ( -37.13343218396168055, -276.5572309816907364, -347.3123460101353430 ) ) ;
#60763 = CARTESIAN_POINT ( 'NONE',  ( -68.60311088225260789, -272.0342412623425048, -203.4954605661089033 ) ) ;
#60764 = CARTESIAN_POINT ( 'NONE',  ( -77.50980347881689170, -281.3677527964491674, -207.8707562732455472 ) ) ;
#60765 = CARTESIAN_POINT ( 'NONE',  ( 34.07987114704710052, -273.9554615985016994, -290.6517089689587010 ) ) ;
#60766 = CARTESIAN_POINT ( 'NONE',  ( -50.03760320576009946, -299.0916068100385132, -198.0704232228478077 ) ) ;
#60767 = CARTESIAN_POINT ( 'NONE',  ( -33.80710660935124423, -299.1770948104688159, -197.0513362399274229 ) ) ;
#60768 = CARTESIAN_POINT ( 'NONE',  ( -98.46307687774019257, -298.7640649792687100, -224.8352926383275872 ) ) ;
#60769 = VECTOR ( 'NONE', #80569, 1000.000000000000000 ) ;
#60770 = CARTESIAN_POINT ( 'NONE',  ( -69.40842366796222507, -271.6524719580954184, -202.1551375255288860 ) ) ;
#60771 = CARTESIAN_POINT ( 'NONE',  ( 35.81003336094614298, -294.2087214731897689, -270.7522010472350757 ) ) ;
#60772 = CARTESIAN_POINT ( 'NONE',  ( 28.01813084454555636, -291.6707173162600952, -236.5459230144966227 ) ) ;
#60773 = CARTESIAN_POINT ( 'NONE',  ( 82.64890176555634582, -299.5541904835127980, -195.3611179825600175 ) ) ;
#60774 = CARTESIAN_POINT ( 'NONE',  ( 36.82797193290609528, -276.3014956093302317, -290.8647588486030031 ) ) ;
#60775 = CARTESIAN_POINT ( 'NONE',  ( -74.27521574020947526, -273.7134378322872408, -207.3349863874383914 ) ) ;
#60776 = AXIS2_PLACEMENT_3D ( 'NONE', #12221, #46783, #57203 ) ;
#60777 = CARTESIAN_POINT ( 'NONE',  ( 24.69751471559726852, -280.8347160513006315, -315.1542568591549411 ) ) ;
#60778 = CARTESIAN_POINT ( 'NONE',  ( -25.17875651936905967, -296.8977247267555981, -344.5899816567116432 ) ) ;
#60779 = DIRECTION ( 'NONE',  ( 0.000000000000000000, 0.000000000000000000, -1.000000000000000000 ) ) ;
#60780 = CARTESIAN_POINT ( 'NONE',  ( -107.9196266375112998, -283.4947241350890863, -289.6790933721925398 ) ) ;
#60781 = CARTESIAN_POINT ( 'NONE',  ( -94.88369293235605539, -281.8847434509306709, -318.7437080750573841 ) ) ;
#60782 = EDGE_CURVE ( 'NONE', #47026, #6475, #30172, .T. ) ;
#60783 = EDGE_CURVE ( 'NONE', #26361, #14181, #74581, .T. ) ;
#60784 = CARTESIAN_POINT ( 'NONE',  ( 16.95373579792595464, -274.8339509894146886, -320.0526417017233598 ) ) ;
#60785 = CARTESIAN_POINT ( 'NONE',  ( 36.75636932795132594, -283.7053378330349460, -282.2790430312370518 ) ) ;
#60786 = LINE ( 'NONE', #18617, #26204 ) ;
#60787 = CARTESIAN_POINT ( 'NONE',  ( 160.5350683151633291, 275.5000000000000568, 20.22542485937379908 ) ) ;
#60788 = CARTESIAN_POINT ( 'NONE',  ( -76.00901147481471298, -271.9449645036021366, -204.6398238528950628 ) ) ;
#60789 = CARTESIAN_POINT ( 'NONE',  ( -50.95498404725360331, -279.2258922872036919, -344.2847740383422774 ) ) ;
#60790 = FACE_OUTER_BOUND ( 'NONE', #28052, .T. ) ;
#60791 = CARTESIAN_POINT ( 'NONE',  ( -93.31566659678372844, -285.7694239595713839, -321.1368692508020786 ) ) ;
#60792 = CARTESIAN_POINT ( 'NONE',  ( 156.4972887742121372, 15.41695093167107444, -9.987829044571977732 ) ) ;
#60793 = CARTESIAN_POINT ( 'NONE',  ( -54.53526744323139042, -287.2727716132861815, -343.4164821795676517 ) ) ;
#60794 = CARTESIAN_POINT ( 'NONE',  ( -23.40286736638519471, -122.5496321078137356, 21.50000000000000000 ) ) ;
#60795 = CARTESIAN_POINT ( 'NONE',  ( -106.1728823496114131, -295.6867771098327466, -244.7312974594291575 ) ) ;
#60796 = CARTESIAN_POINT ( 'NONE',  ( 22.14939115793219671, -286.3046816110265240, -314.7859417202719783 ) ) ;
#60797 = CARTESIAN_POINT ( 'NONE',  ( 116.7412556412048872, 151.1295779098236665, -261.7160256675778101 ) ) ;
#60798 = CARTESIAN_POINT ( 'NONE',  ( -111.2423151236370273, -294.7162722502666838, -257.5665975275372261 ) ) ;
#60799 = CARTESIAN_POINT ( 'NONE',  ( 21.85490609014552277, -286.6841344571441255, -318.5321637991604007 ) ) ;
#60800 = CARTESIAN_POINT ( 'NONE',  ( 36.48719834334961831, -283.1285743558139529, -268.5437643391194911 ) ) ;
#60801 = CARTESIAN_POINT ( 'NONE',  ( -13.75800069724405006, -280.9900435000882339, -342.5953420965402643 ) ) ;
#60802 = CARTESIAN_POINT ( 'NONE',  ( -80.40750505393187098, -289.6538554281773941, -329.3675222663868567 ) ) ;
#60803 = CARTESIAN_POINT ( 'NONE',  ( 33.89847087420039173, -283.2195696396389053, -288.8562226198936287 ) ) ;
#60804 = CARTESIAN_POINT ( 'NONE',  ( 1.195035870662750854, -283.3264104712855556, -332.6096808700619363 ) ) ;
#60805 = CARTESIAN_POINT ( 'NONE',  ( 36.11057925890029452, -289.3163342305804804, -253.4762966734355700 ) ) ;
#60806 = CARTESIAN_POINT ( 'NONE',  ( -101.1933853331745183, -273.4531112965436250, -227.2696249463543552 ) ) ;
#60807 = CARTESIAN_POINT ( 'NONE',  ( -31.26006513394235498, -274.1269369052573666, -193.5883830188325021 ) ) ;
#60808 = CARTESIAN_POINT ( 'NONE',  ( -68.51047276076144499, -293.6204823682541587, -202.5211590025788269 ) ) ;
#60809 = CARTESIAN_POINT ( 'NONE',  ( 139.6539576904058606, 275.0000000000000568, -10.49999999999999822 ) ) ;
#60810 = CARTESIAN_POINT ( 'NONE',  ( -110.4683760289727132, -281.2662352645559167, -253.7030783399848985 ) ) ;
#60811 = CARTESIAN_POINT ( 'NONE',  ( -23.30680261418458343, -274.8730716088636541, -344.2587802214222279 ) ) ;
#60812 = DIRECTION ( 'NONE',  ( 0.000000000000000000, 1.000000000000000000, 0.000000000000000000 ) ) ;
#60813 = CARTESIAN_POINT ( 'NONE',  ( -112.3480179013503744, -295.1218126160890733, -256.9263604243116106 ) ) ;
#60814 = CARTESIAN_POINT ( 'NONE',  ( -107.7087663347654285, -291.8585772610217077, -292.7767085358653958 ) ) ;
#60815 = CARTESIAN_POINT ( 'NONE',  ( -78.90622225098150011, -272.8242154691228620, -210.1640941364211699 ) ) ;
#60816 = CARTESIAN_POINT ( 'NONE',  ( -107.6690269568915994, -292.3618331913442034, -248.3009687442127529 ) ) ;
#60817 = CARTESIAN_POINT ( 'NONE',  ( -49.74031641792665681, -292.8315219245278627, -198.1314937105648539 ) ) ;
#60818 = CARTESIAN_POINT ( 'NONE',  ( -5.577999932653798787, -284.3887464086511159, -337.2259497909354877 ) ) ;
#60819 = CARTESIAN_POINT ( 'NONE',  ( -95.22651626368973155, -292.6563028435225533, -220.4617148057882048 ) ) ;
#60820 = CARTESIAN_POINT ( 'NONE',  ( -95.29836750323146077, -292.5462223569459184, -220.3978906781019873 ) ) ;
#60821 = CARTESIAN_POINT ( 'NONE',  ( 32.74958095056982899, -293.6558738629894378, -290.8073247116167295 ) ) ;
#60822 = CARTESIAN_POINT ( 'NONE',  ( 36.73860467801897300, -289.7037128782220066, -282.1524939225739104 ) ) ;
#60823 = CARTESIAN_POINT ( 'NONE',  ( 39.61987265259269009, -281.7492517272943360, -272.7934665616442658 ) ) ;
#60824 = CARTESIAN_POINT ( 'NONE',  ( -62.34504856052931387, -295.8092548418420051, -199.0579149401790460 ) ) ;
#60825 = CARTESIAN_POINT ( 'NONE',  ( -76.10488502040935543, -285.3828571136864980, -203.7684064659030980 ) ) ;
#60826 = CARTESIAN_POINT ( 'NONE',  ( 14.90009663019717223, -278.2916971847221248, -323.7495573974704826 ) ) ;
#60827 = CARTESIAN_POINT ( 'NONE',  ( -0.6712476517365167927, -284.5390993890048321, -204.9226209660616007 ) ) ;
#60828 = CARTESIAN_POINT ( 'NONE',  ( -62.02631362342228982, -275.5091540005923889, -342.0473562656083004 ) ) ;
#60830 = VECTOR ( 'NONE', #51318, 1000.000000000000000 ) ;
#60829 = DIRECTION ( 'NONE',  ( 0.000000000000000000, 0.000000000000000000, -1.000000000000000000 ) ) ;
#60831 = CARTESIAN_POINT ( 'NONE',  ( -65.34507733012496544, -282.9359737633875511, -337.8565728542171769 ) ) ;
#60832 = AXIS2_PLACEMENT_3D ( 'NONE', #91760, #28326, #6076 ) ;
#60833 = CARTESIAN_POINT ( 'NONE',  ( -61.93475399092118749, -280.9446255697283732, -197.7573221687828777 ) ) ;
#60834 = CARTESIAN_POINT ( 'NONE',  ( 38.55475922663300281, -286.4653778678508047, -258.7605743357725601 ) ) ;
#60835 = CARTESIAN_POINT ( 'NONE',  ( -23.30498707026846006, -296.6305102150933521, -343.0835497460565193 ) ) ;
#60836 = CARTESIAN_POINT ( 'NONE',  ( 1.987468316123474743, -276.1694666284984692, -205.0950707262607864 ) ) ;
#60837 = VECTOR ( 'NONE', #32943, 1000.000000000000000 ) ;
#60838 = CARTESIAN_POINT ( 'NONE',  ( 19.65719522678299569, -276.1699848890896760, -219.2497248943195700 ) ) ;
#60839 = CARTESIAN_POINT ( 'NONE',  ( -43.20920539759533341, -276.9616261248662568, -343.1249303237182744 ) ) ;
#60840 = CARTESIAN_POINT ( 'NONE',  ( -110.1445828276842747, -274.7446490534849204, -253.8812187734843633 ) ) ;
#60841 = CARTESIAN_POINT ( 'NONE',  ( -6.231675163225775194, -284.4616492663730014, -202.2868147826131349 ) ) ;
#60842 = TOROIDAL_SURFACE ( 'NONE', #33581, 1.000000000000000000, 0.5000000000000000000 ) ;
#60843 = CARTESIAN_POINT ( 'NONE',  ( -111.7794328813565841, -291.9463672578704063, -286.6541950712156108 ) ) ;
#60844 = CARTESIAN_POINT ( 'NONE',  ( 4.692086760122460731, -291.5546010140099042, -210.2373567126780358 ) ) ;
#60845 = VERTEX_POINT ( 'NONE', #7014 ) ;
#60846 = CARTESIAN_POINT ( 'NONE',  ( -22.73225063113101641, -291.9110379183019859, -198.8163664484579556 ) ) ;
#60847 = EDGE_LOOP ( 'NONE', ( #61207, #52541 ) ) ;
#60848 = CARTESIAN_POINT ( 'NONE',  ( -106.2297794422614032, -291.1959038415723171, -304.1852723105001246 ) ) ;
#60849 = CARTESIAN_POINT ( 'NONE',  ( -30.26075729855522312, -280.7953690375561564, -197.5525115200956634 ) ) ;
#60850 = EDGE_CURVE ( 'NONE', #25416, #4814, #23390, .T. ) ;
#60851 = CARTESIAN_POINT ( 'NONE',  ( -113.4662798553950438, -295.5892960423192335, -261.0583833959526032 ) ) ;
#60852 = CARTESIAN_POINT ( 'NONE',  ( 27.36352340955343720, -288.7504862338125236, -312.0110527152506279 ) ) ;
#60853 = CARTESIAN_POINT ( 'NONE',  ( 39.61882045983549716, -287.8644155687239277, -268.6810696876136717 ) ) ;
#60854 = CARTESIAN_POINT ( 'NONE',  ( -110.3305858718521080, -284.9140566143531714, -268.1908542738848382 ) ) ;
#60855 = CARTESIAN_POINT ( 'NONE',  ( -100.0921933642221262, -248.0253980568164707, -334.2282667577409825 ) ) ;
#60856 = CARTESIAN_POINT ( 'NONE',  ( -114.0693070538299025, -271.3720280936893801, -283.9001697967761970 ) ) ;
#60857 = CARTESIAN_POINT ( 'NONE',  ( 120.9637783430752194, 147.7793525261007517, -260.2308592555319819 ) ) ;
#60858 = CARTESIAN_POINT ( 'NONE',  ( -41.87678651537783736, -276.3078880379102316, -343.3945250170900181 ) ) ;
#60859 = CARTESIAN_POINT ( 'NONE',  ( -68.17991660165073142, -276.3872551470253711, -336.8822968477151107 ) ) ;
#60860 = CARTESIAN_POINT ( 'NONE',  ( -111.0156482867775196, -272.5011039155673416, -247.8654095336068792 ) ) ;
#60861 = CARTESIAN_POINT ( 'NONE',  ( 7.012673261725664631, -59.86950493046524002, -351.5097822906775491 ) ) ;
#60862 = CARTESIAN_POINT ( 'NONE',  ( -98.41990559247783210, -276.6192401504480358, -316.4559481810226202 ) ) ;
#60863 = ORIENTED_EDGE ( 'NONE', *, *, #53345, .F. ) ;
#60864 = CARTESIAN_POINT ( 'NONE',  ( -109.3384937489187365, -291.2121157218818439, -257.6443230883305091 ) ) ;
#60865 = CARTESIAN_POINT ( 'NONE',  ( -51.78031750999734584, -298.6749000152849476, -194.8371281121234802 ) ) ;
#60866 = CARTESIAN_POINT ( 'NONE',  ( -110.7562980512556550, -297.3359417346396754, -247.1665643613593204 ) ) ;
#60867 = CARTESIAN_POINT ( 'NONE',  ( -23.51675539574290141, -295.0373054540339695, -342.0916657439329924 ) ) ;
#60868 = ORIENTED_EDGE ( 'NONE', *, *, #69913, .T. ) ;
#60869 = CARTESIAN_POINT ( 'NONE',  ( -35.71747977770257876, -278.9521074997410892, -345.9165408602531784 ) ) ;
#60870 = CARTESIAN_POINT ( 'NONE',  ( 39.21621148718058691, -281.1619039793872616, -278.5182402958640182 ) ) ;
#60871 = CARTESIAN_POINT ( 'NONE',  ( -106.7417964493630791, -279.9462330764431499, -246.5862357033571755 ) ) ;
#60872 = CARTESIAN_POINT ( 'NONE',  ( 23.56898718091759548, -277.9246538853166157, -315.7908680092711506 ) ) ;
#60873 = CARTESIAN_POINT ( 'NONE',  ( -71.92599426686081188, -296.1602792394132280, -205.3906564031655364 ) ) ;
#60874 = DIRECTION ( 'NONE',  ( 0.000000000000000000, 1.000000000000000000, 0.000000000000000000 ) ) ;
#60875 = CARTESIAN_POINT ( 'NONE',  ( -95.27172446263537609, -278.0938915949686248, -314.7808465401516287 ) ) ;
#60876 = CARTESIAN_POINT ( 'NONE',  ( -10.41380252585087085, -275.1974309378805970, -198.3389197026997977 ) ) ;
#60877 = CARTESIAN_POINT ( 'NONE',  ( 34.60296919278211902, -286.5695158995300744, -296.5394315884936987 ) ) ;
#60878 = CARTESIAN_POINT ( 'NONE',  ( -70.54101747615872853, -275.6145636479400878, -203.1093077409857983 ) ) ;
#60879 = CARTESIAN_POINT ( 'NONE',  ( -6.826812122227570612, -275.2341638968416078, -340.4284423441138188 ) ) ;
#60880 = CARTESIAN_POINT ( 'NONE',  ( -21.10342142747762040, -288.0355915397917101, -341.6977847904311716 ) ) ;
#60881 = CARTESIAN_POINT ( 'NONE',  ( -106.5837236188485946, -284.3304859965283526, -236.9118284658580080 ) ) ;
#60882 = CARTESIAN_POINT ( 'NONE',  ( -10.63069602162725147, -280.9388972310754298, -339.4407650353487611 ) ) ;
#60884 = CARTESIAN_POINT ( 'NONE',  ( -27.62484166460048485, -284.2563766629464794, -196.5580228042815918 ) ) ;
#60883 = CARTESIAN_POINT ( 'NONE',  ( -6.506085041916287892, -279.0399432232309209, -203.5301494664145991 ) ) ;
#60885 = CARTESIAN_POINT ( 'NONE',  ( -49.03810851199094145, -291.2012050072701754, -344.4954494982267761 ) ) ;
#60886 = CARTESIAN_POINT ( 'NONE',  ( -110.0171913352463093, -279.8965676159797340, -259.7413290855270702 ) ) ;
#60887 = CARTESIAN_POINT ( 'NONE',  ( -92.65263417022424619, -271.2595425636271216, -219.6894121869859475 ) ) ;
#60888 = AXIS2_PLACEMENT_3D ( 'NONE', #85466, #20613, #85917 ) ;
#60889 = CARTESIAN_POINT ( 'NONE',  ( -5.805400873493357317, -281.0442634428700899, -339.7289941723872175 ) ) ;
#60890 = CARTESIAN_POINT ( 'NONE',  ( -1.635306520508392980, -296.5791324490617740, -336.3305588021367498 ) ) ;
#60891 = CARTESIAN_POINT ( 'NONE',  ( -70.76836225225842725, -277.8571602945608561, -202.1215966128965249 ) ) ;
#60892 = VECTOR ( 'NONE', #26632, 1000.000000000000000 ) ;
#60893 = CARTESIAN_POINT ( 'NONE',  ( -105.3596130347175830, -278.8458578835282538, -297.1464907029498477 ) ) ;
#60894 = CARTESIAN_POINT ( 'NONE',  ( -57.95884006883206041, -285.3178921283748650, -342.6991879834647534 ) ) ;
#60895 = AXIS2_PLACEMENT_3D ( 'NONE', #60072, #66695, #81812 ) ;
#60896 = CARTESIAN_POINT ( 'NONE',  ( 198.0308761633362451, 68.10075688722794496, 9.048087686121785822 ) ) ;
#60897 = CARTESIAN_POINT ( 'NONE',  ( -109.0717807365721796, -292.7788345443277649, -246.4462226930556596 ) ) ;
#60898 = AXIS2_PLACEMENT_3D ( 'NONE', #26558, #18992, #84298 ) ;
#60899 = CARTESIAN_POINT ( 'NONE',  ( 4.221867437276329404, -274.4916737333997503, -332.7908424578108111 ) ) ;
#60900 = ADVANCED_FACE ( 'NONE', ( #28785 ), #65257, .F. ) ;
#60901 = CARTESIAN_POINT ( 'NONE',  ( 26.22953056051999710, -286.1788157278412541, -227.1767770054204902 ) ) ;
#60902 = CARTESIAN_POINT ( 'NONE',  ( -109.2018237356184187, -289.1720842373956089, -253.4964591964692886 ) ) ;
#60903 = CARTESIAN_POINT ( 'NONE',  ( -43.41367318021437427, -261.6989687524993542, -437.8242190674686753 ) ) ;
#60904 = CARTESIAN_POINT ( 'NONE',  ( 36.09380205321358659, -274.2893168500118009, -274.3560216317447953 ) ) ;
#60905 = CARTESIAN_POINT ( 'NONE',  ( -39.75249119247741447, -293.2223002679822912, -344.5698066662969268 ) ) ;
#60906 = DIRECTION ( 'NONE',  ( 0.000000000000000000, 0.000000000000000000, -1.000000000000000000 ) ) ;
#60907 = CARTESIAN_POINT ( 'NONE',  ( 197.1656530321902494, 41.90019538913895758, 12.64285714285713702 ) ) ;
#60908 = CARTESIAN_POINT ( 'NONE',  ( 35.70032196455616713, -292.3137547521488955, -292.6209623261899537 ) ) ;
#60909 = CARTESIAN_POINT ( 'NONE',  ( -107.2971011534770298, -286.4630654634752318, -246.6917724943312180 ) ) ;
#60910 = CARTESIAN_POINT ( 'NONE',  ( -65.09804110336834526, -287.6496057294341995, -341.1525708390706200 ) ) ;
#60911 = CARTESIAN_POINT ( 'NONE',  ( 36.24454981381345675, -288.9860998229279403, -271.0234886567196213 ) ) ;
#60912 = EDGE_CURVE ( 'NONE', #56563, #92061, #20246, .T. ) ;
#60913 = CARTESIAN_POINT ( 'NONE',  ( 204.6539576904058606, 293.9636489450775230, 0.000000000000000000 ) ) ;
#60914 = CARTESIAN_POINT ( 'NONE',  ( 20.49138996257856249, -288.9848840174375937, -315.1913983257797440 ) ) ;
#60915 = CARTESIAN_POINT ( 'NONE',  ( 29.45623181886886144, -295.9918134000988630, -305.2386621550447785 ) ) ;
#60916 = CARTESIAN_POINT ( 'NONE',  ( -83.63170945779074827, -298.0521521680024080, -521.1711561948568487 ) ) ;
#60917 = CARTESIAN_POINT ( 'NONE',  ( 35.46680462655513821, -288.4541812801169840, -246.3812847724732933 ) ) ;
#60918 = CARTESIAN_POINT ( 'NONE',  ( -83.99681604864225903, -275.7669178214848102, -329.8634179780800082 ) ) ;
#60919 = CARTESIAN_POINT ( 'NONE',  ( -91.31118456961688423, -278.1274226897337485, -325.3269166717917074 ) ) ;
#60920 = CARTESIAN_POINT ( 'NONE',  ( -31.07124718639040495, -279.7959131297903355, -193.5853962490653828 ) ) ;
#60921 = CARTESIAN_POINT ( 'NONE',  ( -69.99940754903839490, -299.5996887559617221, -203.2394303311089629 ) ) ;
#60922 = CARTESIAN_POINT ( 'NONE',  ( -43.37491821897447153, -265.5697000172091293, -503.0412998836937390 ) ) ;
#60923 = CARTESIAN_POINT ( 'NONE',  ( -98.18273508716090703, -283.1492142510139729, -226.4829862028017544 ) ) ;
#60924 = CARTESIAN_POINT ( 'NONE',  ( 193.9723528053802397, 215.0000000000000568, 17.29054515234648548 ) ) ;
#60925 = CARTESIAN_POINT ( 'NONE',  ( -109.8074234743274076, -276.9014255598690397, -254.1913883450073683 ) ) ;
#60926 = CARTESIAN_POINT ( 'NONE',  ( 35.24946140037768316, -279.7942833017772841, -289.2164599249180696 ) ) ;
#60927 = CARTESIAN_POINT ( 'NONE',  ( -72.53825824055297744, -275.9893228037450967, -338.0802701167282862 ) ) ;
#60928 = CARTESIAN_POINT ( 'NONE',  ( -110.7427456301928856, -298.1651816732067459, -263.2518405327273854 ) ) ;
#60929 = CARTESIAN_POINT ( 'NONE',  ( 19.54494539847626911, -281.1744367786498628, -321.8722679609660418 ) ) ;
#60930 = CARTESIAN_POINT ( 'NONE',  ( -71.78623215759699860, -298.5264210434215215, -205.7172929439894915 ) ) ;
#60931 = CARTESIAN_POINT ( 'NONE',  ( -107.3287305190174834, -298.2656397175628058, -239.3251538602405617 ) ) ;
#60932 = CARTESIAN_POINT ( 'NONE',  ( -11.47876152423410012, -274.0651263854016406, -202.0194579617432282 ) ) ;
#60933 = CARTESIAN_POINT ( 'NONE',  ( 35.89748046692128014, -295.3441041799431446, -254.1456147269440748 ) ) ;
#60934 = CARTESIAN_POINT ( 'NONE',  ( 32.71114548599666705, -287.3087945676935533, -238.2703115212273133 ) ) ;
#60935 = CARTESIAN_POINT ( 'NONE',  ( -111.3028778141268589, -276.8298452275348041, -254.8373080206446275 ) ) ;
#60936 = CARTESIAN_POINT ( 'NONE',  ( -92.81061117759203682, -291.1172771414280760, -216.8792735966704299 ) ) ;
#60937 = CARTESIAN_POINT ( 'NONE',  ( 15.20664587493637754, -285.8757698668489979, -219.3505329986435299 ) ) ;
#60938 = CARTESIAN_POINT ( 'NONE',  ( -112.3674735616446299, -288.5774064209878702, -268.3814107934063600 ) ) ;
#60939 = VERTEX_POINT ( 'NONE', #58144 ) ;
#60940 = CARTESIAN_POINT ( 'NONE',  ( 201.9366853066881333, 285.6703355482916322, -112.9373754057687478 ) ) ;
#60941 = CARTESIAN_POINT ( 'NONE',  ( -5.771512504505313501, -288.1330864019253681, -336.2497489844104166 ) ) ;
#60942 = CARTESIAN_POINT ( 'NONE',  ( 202.6701092853567445, 300.2474117005756966, -4.951178257753966250 ) ) ;
#60943 = CARTESIAN_POINT ( 'NONE',  ( -90.26721016457766211, -284.7198748291708625, -326.0371448199137490 ) ) ;
#60944 = CARTESIAN_POINT ( 'NONE',  ( -22.22834588464579397, -291.2997836708109958, -195.0447033697467134 ) ) ;
#60945 = CARTESIAN_POINT ( 'NONE',  ( 37.19780101539632966, -282.9515460032649230, -254.4777995071097507 ) ) ;
#60946 = CARTESIAN_POINT ( 'NONE',  ( -36.77314726115923094, -281.3743265107244724, -193.8434177663166338 ) ) ;
#60947 = CARTESIAN_POINT ( 'NONE',  ( -80.62784257134325117, -283.4907761331751885, -329.2058946090111817 ) ) ;
#60948 = CARTESIAN_POINT ( 'NONE',  ( -93.66275172753762490, -297.2686260922384349, -217.7767815830889617 ) ) ;
#60949 = CARTESIAN_POINT ( 'NONE',  ( -106.7777621129673378, -274.1854271808723524, -246.2804873080846164 ) ) ;
#60950 = CARTESIAN_POINT ( 'NONE',  ( -0.4216908220641580329, -290.5655556653375129, -205.4713596146963823 ) ) ;
#60951 = CARTESIAN_POINT ( 'NONE',  ( -89.51369196214632495, -272.0913581842083886, -218.7354095356930941 ) ) ;
#60952 = ORIENTED_EDGE ( 'NONE', *, *, #10009, .T. ) ;
#60953 = CARTESIAN_POINT ( 'NONE',  ( 159.4851178187871312, 0.000000000000000000, -9.000000000000001776 ) ) ;
#60954 = CARTESIAN_POINT ( 'NONE',  ( -106.5437535757966998, -286.1108293599751846, -297.9310442091336313 ) ) ;
#60955 = CIRCLE ( 'NONE', #79141, 4.000000000000003553 ) ;
#60956 = CARTESIAN_POINT ( 'NONE',  ( -5.911760247855728956, -295.7282323973454368, -340.3157560695121902 ) ) ;
#60957 = CARTESIAN_POINT ( 'NONE',  ( -72.43021848497625115, -286.2261686717989733, -206.2166341382790620 ) ) ;
#60958 = CARTESIAN_POINT ( 'NONE',  ( 34.97525851975475319, -274.9386665362083022, -296.2680236554453472 ) ) ;
#60959 = CARTESIAN_POINT ( 'NONE',  ( -5.936167116395469456, -293.1056374952254941, -200.1542195160551785 ) ) ;
#60960 = CARTESIAN_POINT ( 'NONE',  ( 9.073040986028631849, -284.8212726493908917, -210.4780879564944200 ) ) ;
#60961 = CARTESIAN_POINT ( 'NONE',  ( -8.523074194401136339, -292.7524918422712972, -198.9802305487791330 ) ) ;
#60963 = CARTESIAN_POINT ( 'NONE',  ( -66.33352022100316958, -289.7756429435258951, -337.4342636827961996 ) ) ;
#60962 = CIRCLE ( 'NONE', #20131, 5.000000000000000888 ) ;
#60964 = DIRECTION ( 'NONE',  ( 1.000000000000000000, 0.000000000000000000, 0.000000000000000000 ) ) ;
#60965 = AXIS2_PLACEMENT_3D ( 'NONE', #54919, #89965, #25119 ) ;
#60966 = DIRECTION ( 'NONE',  ( -1.000000000000000000, 0.000000000000000000, 0.000000000000000000 ) ) ;
#60967 = CARTESIAN_POINT ( 'NONE',  ( -30.22320482856529722, -125.1503534454012936, -360.5410437172449178 ) ) ;
#60968 = CARTESIAN_POINT ( 'NONE',  ( -109.3296401210003523, -286.3944112642278697, -245.0541180135221566 ) ) ;
#60969 = CARTESIAN_POINT ( 'NONE',  ( -55.63300648810263738, -274.7666405000204009, -350.3538533559490702 ) ) ;
#60970 = EDGE_LOOP ( 'NONE', ( #56228, #86687, #92606, #71130 ) ) ;
#60971 = ADVANCED_FACE ( 'NONE', ( #1290 ), #839, .F. ) ;
#60973 = CARTESIAN_POINT ( 'NONE',  ( -36.20246041631732226, -281.9578624882905729, -343.6613786060121356 ) ) ;
#60972 = CIRCLE ( 'NONE', #83441, 0.5000000000000004441 ) ;
#60974 = CARTESIAN_POINT ( 'NONE',  ( -75.32946031783012586, -277.2110569084267127, -337.3138951266201389 ) ) ;
#60975 = CARTESIAN_POINT ( 'NONE',  ( -38.40486519006801558, -282.0389554383885979, -195.5226202331257355 ) ) ;
#60976 = CARTESIAN_POINT ( 'NONE',  ( -107.2154437152842945, -266.9835763933201065, -306.3795532216186643 ) ) ;
#60977 = EDGE_CURVE ( 'NONE', #70200, #55010, #4924, .T. ) ;
#60978 = CARTESIAN_POINT ( 'NONE',  ( -31.69805762668363158, -281.5569927075723626, -346.5763551601082781 ) ) ;
#60980 = AXIS2_PLACEMENT_3D ( 'NONE', #51916, #58587, #31097 ) ;
#60979 = CARTESIAN_POINT ( 'NONE',  ( -6.310229728316707032, -284.4819142837348522, -202.4582388971718387 ) ) ;
#60981 = CARTESIAN_POINT ( 'NONE',  ( -103.1682908359319839, -274.9089003659482273, -232.7435711099594187 ) ) ;
#60982 = CARTESIAN_POINT ( 'NONE',  ( -39.68473477704340269, -295.5746829940383122, -343.3975182829540245 ) ) ;
#60983 = ORIENTED_EDGE ( 'NONE', *, *, #5338, .F. ) ;
#60984 = CARTESIAN_POINT ( 'NONE',  ( -9.525401424345631085, -291.1080999299807104, -202.2812549465983238 ) ) ;
#60985 = CARTESIAN_POINT ( 'NONE',  ( -80.16252965506953387, -278.2664605796620663, -334.2976598376451420 ) ) ;
#60986 = CARTESIAN_POINT ( 'NONE',  ( -1.722629687625949035, -274.5381631485593630, -206.6264638329723482 ) ) ;
#60987 = CARTESIAN_POINT ( 'NONE',  ( 32.73173550489364914, -274.8718496277727468, -301.5252981818229614 ) ) ;
#60988 = DIRECTION ( 'NONE',  ( 0.000000000000000000, 0.000000000000000000, -1.000000000000000000 ) ) ;
#60989 = CARTESIAN_POINT ( 'NONE',  ( -44.50459460446958104, -271.9614922888616775, -195.6525544874369587 ) ) ;
#60990 = AXIS2_PLACEMENT_3D ( 'NONE', #85356, #91015, #84400 ) ;
#60991 = CARTESIAN_POINT ( 'NONE',  ( -4.737354725767092489, -296.0563668209754837, -339.4809271487356455 ) ) ;
#60992 = CARTESIAN_POINT ( 'NONE',  ( 194.5881128153457098, 0.000000000000000000, 10.00000000000000178 ) ) ;
#60993 = EDGE_CURVE ( 'NONE', #61449, #15987, #21551, .T. ) ;
#60994 = DIRECTION ( 'NONE',  ( 0.000000000000000000, 0.000000000000000000, 1.000000000000000000 ) ) ;
#60995 = AXIS2_PLACEMENT_3D ( 'NONE', #8831, #8379, #9290 ) ;
#60996 = CARTESIAN_POINT ( 'NONE',  ( -73.93923254637256548, -284.6298300622254942, -333.9394035806447505 ) ) ;
#60997 = CARTESIAN_POINT ( 'NONE',  ( 32.64152977366871511, -283.6955925247962114, -300.0983151194007519 ) ) ;
#60998 = CARTESIAN_POINT ( 'NONE',  ( -92.64166952185115633, -283.2203034464520783, -318.1902739854505739 ) ) ;
#60999 = CARTESIAN_POINT ( 'NONE',  ( 32.85288048449277909, -274.2510478427392968, -293.1462286413533889 ) ) ;
#61000 = CARTESIAN_POINT ( 'NONE',  ( -33.40746527298313140, -284.8625506324412981, -344.5047825522538574 ) ) ;
#61001 = CARTESIAN_POINT ( 'NONE',  ( -40.55519323025595924, -275.5731334400442734, -343.9969387944634036 ) ) ;
#61002 = CARTESIAN_POINT ( 'NONE',  ( -5.184822844517078089, -275.5653237701049534, -204.4673361643625924 ) ) ;
#61003 = CARTESIAN_POINT ( 'NONE',  ( 194.2870706637141325, 39.36132622696000993, 14.58823529411763431 ) ) ;
#61004 = CARTESIAN_POINT ( 'NONE',  ( -53.73601682802289048, -280.6498880562636487, -195.2374593115058303 ) ) ;
#61005 = TOROIDAL_SURFACE ( 'NONE', #9606, 25.50000000000000355, 0.5000000000000000000 ) ;
#61006 = ORIENTED_EDGE ( 'NONE', *, *, #84888, .F. ) ;
#61007 = DIRECTION ( 'NONE',  ( 0.000000000000000000, 0.000000000000000000, 1.000000000000000000 ) ) ;
#61008 = CARTESIAN_POINT ( 'NONE',  ( -26.81651820911489281, -288.0449209414952065, -195.2783111190236127 ) ) ;
#61009 = CARTESIAN_POINT ( 'NONE',  ( -12.96405449157867729, -293.9243993690338925, -339.3951554032333320 ) ) ;
#61010 = CARTESIAN_POINT ( 'NONE',  ( -113.9045171092163855, -289.9974451713500230, -262.6389360753772166 ) ) ;
#61011 = CARTESIAN_POINT ( 'NONE',  ( 15.77208358223047568, -285.0570126895580643, -218.8159921888677957 ) ) ;
#61013 = CARTESIAN_POINT ( 'NONE',  ( -86.58677046857999926, -289.5969896313118852, -215.0391265426446807 ) ) ;
#61012 = CARTESIAN_POINT ( 'NONE',  ( 35.86238062741225718, -286.0284778067418188, -262.8419772613049759 ) ) ;
#61014 = CARTESIAN_POINT ( 'NONE',  ( -5.640974070528423923, -287.6836297779189522, -204.1491145502959341 ) ) ;
#61015 = CARTESIAN_POINT ( 'NONE',  ( -112.3763323641495617, -276.5726598156686009, -268.7510845046080590 ) ) ;
#61016 = CARTESIAN_POINT ( 'NONE',  ( 16.11010880861870476, -286.7095308492217214, -324.7423389381839911 ) ) ;
#61017 = CARTESIAN_POINT ( 'NONE',  ( 21.40888422927025658, -288.9115637186320100, -223.7212466847239227 ) ) ;
#61018 = CARTESIAN_POINT ( 'NONE',  ( 22.66293520227894476, -286.1695701959802136, -315.6322143759053915 ) ) ;
#61019 = CARTESIAN_POINT ( 'NONE',  ( -48.35226777259792641, -284.1369962038935455, -342.7639898024030458 ) ) ;
#61020 = CARTESIAN_POINT ( 'NONE',  ( -68.57179437363420504, -291.4617104075195471, -338.7470438510124495 ) ) ;
#61021 = CARTESIAN_POINT ( 'NONE',  ( 201.2104617360081704, 250.0000000000000568, -15.00000000000000000 ) ) ;
#61022 = CARTESIAN_POINT ( 'NONE',  ( 165.2494399300530290, 8.542400036368780647, 9.974999999999996092 ) ) ;
#61023 = CARTESIAN_POINT ( 'NONE',  ( -98.76549261286159265, -299.0665086796157652, -226.3562101160223392 ) ) ;
#61024 = CARTESIAN_POINT ( 'NONE',  ( 28.21915272646883821, -279.0672813084037784, -233.9361921875835151 ) ) ;
#61025 = CARTESIAN_POINT ( 'NONE',  ( -56.13936762918189771, -291.0132844020712923, -195.8025523022004677 ) ) ;
#61026 = CARTESIAN_POINT ( 'NONE',  ( -82.41680434362213248, -295.8252478169389974, -211.8611398112899167 ) ) ;
#61027 = CARTESIAN_POINT ( 'NONE',  ( 33.79666536730879756, -280.4795664751766253, -288.8659133817051270 ) ) ;
#61028 = CARTESIAN_POINT ( 'NONE',  ( -70.10310767812671884, -271.6969289599835520, -203.5179853726775150 ) ) ;
#61029 = CARTESIAN_POINT ( 'NONE',  ( -31.54687434219142972, -296.2927845427873876, -343.6759092583322968 ) ) ;
#61030 = DIRECTION ( 'NONE',  ( 0.000000000000000000, 0.000000000000000000, 1.000000000000000000 ) ) ;
#61031 = CARTESIAN_POINT ( 'NONE',  ( -83.21176718700370145, -272.0127664526270905, -209.1839981144141518 ) ) ;
#61032 = CARTESIAN_POINT ( 'NONE',  ( 3.661382102867504873, -292.7488736743098912, -334.3974372014749861 ) ) ;
#61033 = AXIS2_PLACEMENT_3D ( 'NONE', #55663, #12574, #76027 ) ;
#61034 = CARTESIAN_POINT ( 'NONE',  ( -47.09034410794024694, -293.3511698088163371, -197.4204650049438499 ) ) ;
#61035 = CARTESIAN_POINT ( 'NONE',  ( 196.3496553477289979, 249.5000000000000568, -12.41762739670151205 ) ) ;
#61036 = CARTESIAN_POINT ( 'NONE',  ( 20.30381946967143136, -293.7211270258691229, -225.2898041768781354 ) ) ;
#61037 = DIRECTION ( 'NONE',  ( -1.000000000000000000, -0.000000000000000000, -0.000000000000000000 ) ) ;
#61038 = PRESENTATION_LAYER_ASSIGNMENT (  '', '', ( #17149 ) ) ;
#61040 = CARTESIAN_POINT ( 'NONE',  ( -28.89597898657987329, -294.9422432129071012, -342.9219226700741388 ) ) ;
#61039 = CARTESIAN_POINT ( 'NONE',  ( -82.90908606689013993, -281.6916673415432228, -330.4435144732991603 ) ) ;
#61041 = CIRCLE ( 'NONE', #85221, 27.00000000000000355 ) ;
#61042 = CARTESIAN_POINT ( 'NONE',  ( -27.37210054310012097, -282.9289394269802074, -346.7663427963810250 ) ) ;
#61043 = CARTESIAN_POINT ( 'NONE',  ( 37.36711674329588817, -283.3238512005738130, -258.7128930921769552 ) ) ;
#61044 = CARTESIAN_POINT ( 'NONE',  ( -57.74624281317331764, -285.4625034913224795, -196.0804570033125174 ) ) ;
#61045 = CARTESIAN_POINT ( 'NONE',  ( -112.0749672451352694, -288.6133317056160195, -265.5940688975930470 ) ) ;
#61046 = CARTESIAN_POINT ( 'NONE',  ( -21.88550880992767844, -281.3374224339623311, -345.0860395338518174 ) ) ;
#61047 = AXIS2_PLACEMENT_3D ( 'NONE', #84991, #13525, #13989 ) ;
#61048 = EDGE_CURVE ( 'NONE', #11917, #54554, #63902, .T. ) ;
#61049 = CARTESIAN_POINT ( 'NONE',  ( -34.69132753772392164, -287.9399116452678982, -347.0061963352706584 ) ) ;
#61050 = LINE ( 'NONE', #82338, #20427 ) ;
#61051 = CARTESIAN_POINT ( 'NONE',  ( -8.903984791742105998, -296.2740060686122661, -338.4758055268594035 ) ) ;
#61052 = CARTESIAN_POINT ( 'NONE',  ( -68.75641037366860076, -278.8823140277010566, -340.0297160302223460 ) ) ;
#61054 = CARTESIAN_POINT ( 'NONE',  ( -108.6264690372655650, -278.4283129252535218, -254.4745154352592351 ) ) ;
#61053 = CARTESIAN_POINT ( 'NONE',  ( 36.73559792748903874, -291.7497481715136018, -284.2495702668428521 ) ) ;
#61055 = CARTESIAN_POINT ( 'NONE',  ( 19.41422694405919103, -293.0108840301961095, -218.3249310863966457 ) ) ;
#61056 = AXIS2_PLACEMENT_3D ( 'NONE', #50294, #92920, #1047 ) ;
#61057 = CARTESIAN_POINT ( 'NONE',  ( -60.05334970038846620, -283.8400460926261530, -198.2406793992194025 ) ) ;
#61058 = CARTESIAN_POINT ( 'NONE',  ( -76.74197839477417915, -279.5793236921047651, -334.2385306546398738 ) ) ;
#61059 = CARTESIAN_POINT ( 'NONE',  ( 29.70065859092902727, -293.0061559313315911, -299.8353539322247343 ) ) ;
#61060 = CARTESIAN_POINT ( 'NONE',  ( -91.82532259941586972, -271.2771939937046000, -218.5585286426650384 ) ) ;
#61061 = EDGE_LOOP ( 'NONE', ( #46525, #32345, #25335, #8786, #80659, #69082, #34047 ) ) ;
#61062 = FACE_OUTER_BOUND ( 'NONE', #46389, .T. ) ;
#61063 = VECTOR ( 'NONE', #55314, 1000.000000000000114 ) ;
#61064 = CARTESIAN_POINT ( 'NONE',  ( 34.12646259419165062, -293.2606131899670459, -285.5964177754868274 ) ) ;
#61065 = DIRECTION ( 'NONE',  ( 0.000000000000000000, 0.000000000000000000, 1.000000000000000000 ) ) ;
#61066 = CARTESIAN_POINT ( 'NONE',  ( -37.37352853689063181, -286.5523547857346784, -340.3611179825599606 ) ) ;
#61067 = CARTESIAN_POINT ( 'NONE',  ( -80.48285289593823677, -296.5420516916870497, -206.8018494937207095 ) ) ;
#61068 = CARTESIAN_POINT ( 'NONE',  ( -43.64246329926915280, -287.2894238705015937, -194.0612411544955478 ) ) ;
#61069 = CARTESIAN_POINT ( 'NONE',  ( -78.17617355877236207, -289.4512879364974651, -330.9326818215802746 ) ) ;
#61070 = CARTESIAN_POINT ( 'NONE',  ( -93.24003146035299494, -279.3949705593958583, -318.3828246173822549 ) ) ;
#61071 = CARTESIAN_POINT ( 'NONE',  ( -102.1120315737294106, -298.7950788001650153, -234.5452252006443814 ) ) ;
#61072 = AXIS2_PLACEMENT_3D ( 'NONE', #15052, #15510, #9802 ) ;
#61073 = CARTESIAN_POINT ( 'NONE',  ( 9.541903779084519144, -279.5083501258902174, -213.8231064393754366 ) ) ;
#61074 = EDGE_LOOP ( 'NONE', ( #66199, #50727, #16127, #84816 ) ) ;
#61075 = CARTESIAN_POINT ( 'NONE',  ( -20.51140391415574271, -297.9241948780934877, -193.3831815583004641 ) ) ;
#61076 = CARTESIAN_POINT ( 'NONE',  ( -110.1235490894070921, -292.6744282285387726, -254.7368847777409826 ) ) ;
#61077 = CARTESIAN_POINT ( 'NONE',  ( 35.51604006505954914, -294.8690642353187741, -248.0409452780923232 ) ) ;
#61078 = DIRECTION ( 'NONE',  ( 0.000000000000000000, 0.000000000000000000, 1.000000000000000000 ) ) ;
#61079 = CARTESIAN_POINT ( 'NONE',  ( -110.0751374380402012, -291.3001388190311900, -263.0303768795393466 ) ) ;
#61080 = CARTESIAN_POINT ( 'NONE',  ( 197.9816010460261282, 65.99294033139044302, 9.931187365468728601 ) ) ;
#61081 = CARTESIAN_POINT ( 'NONE',  ( 18.52120524151442282, -290.9841152761231342, -219.1786865759690102 ) ) ;
#61082 = CARTESIAN_POINT ( 'NONE',  ( -108.8705253541002378, -297.2480267019304847, -241.7683982936289340 ) ) ;
#61083 = EDGE_CURVE ( 'NONE', #14651, #74347, #12434, .T. ) ;
#61084 = CARTESIAN_POINT ( 'NONE',  ( -92.75768271131310883, -296.8957873112638595, -222.7902687756990474 ) ) ;
#61085 = LINE ( 'NONE', #90835, #87235 ) ;
#61086 = CARTESIAN_POINT ( 'NONE',  ( 195.2312239546292574, 27.48493576247233250, 15.00000000000007638 ) ) ;
#61087 = CARTESIAN_POINT ( 'NONE',  ( -104.5361973912015401, -291.6004754151089742, -306.5219709673091870 ) ) ;
#61088 = CARTESIAN_POINT ( 'NONE',  ( -88.52914483777347243, -293.9090924074131408, -206.2264541496106460 ) ) ;
#61089 = ADVANCED_FACE ( 'NONE', ( #89299 ), #62389, .T. ) ;
#61090 = CARTESIAN_POINT ( 'NONE',  ( -40.06553033087357818, -288.0179972217203499, -195.5773685568224494 ) ) ;
#61091 = EDGE_CURVE ( 'NONE', #85305, #68325, #38660, .T. ) ;
#61092 = CARTESIAN_POINT ( 'NONE',  ( 35.92131433049313216, -273.3549442841310793, -255.0485703507428070 ) ) ;
#61093 = CARTESIAN_POINT ( 'NONE',  ( 20.31210428493328735, -278.1262986156413035, -317.4699913169359320 ) ) ;
#61094 = CARTESIAN_POINT ( 'NONE',  ( -25.14962116923609159, -290.2885025539889057, -196.8738378625922110 ) ) ;
#61095 = CARTESIAN_POINT ( 'NONE',  ( -68.48562749862624344, -279.3173872864225586, -339.4430911085285061 ) ) ;
#61096 = ORIENTED_EDGE ( 'NONE', *, *, #73934, .F. ) ;
#61097 = CARTESIAN_POINT ( 'NONE',  ( -70.26825741715420293, -282.8465380153288606, -335.6417582431500932 ) ) ;
#61098 = CARTESIAN_POINT ( 'NONE',  ( -114.0753947170813660, -279.6160508904845301, -271.6171115694641571 ) ) ;
#61099 = CARTESIAN_POINT ( 'NONE',  ( 33.96048603263501064, -279.9886430435101374, -242.2161422086392122 ) ) ;
#61100 = CARTESIAN_POINT ( 'NONE',  ( 43.74668670635536216, 12.16893915163007733, -329.0196699399712088 ) ) ;
#61101 = CARTESIAN_POINT ( 'NONE',  ( 39.47207304594562061, -276.5033894309517564, -271.1572026706411407 ) ) ;
#61102 = PRODUCT_CONTEXT ( 'NONE', #20284, 'mechanical' ) ;
#61103 = CARTESIAN_POINT ( 'NONE',  ( -0.3982295024258034610, -276.0541650090034977, -203.5788463470345562 ) ) ;
#61104 = CARTESIAN_POINT ( 'NONE',  ( -102.0455923789670294, -275.4805209788415823, -239.2376011013261916 ) ) ;
#61105 = ORIENTED_EDGE ( 'NONE', *, *, #5615, .F. ) ;
#61106 = ORIENTED_EDGE ( 'NONE', *, *, #78869, .T. ) ;
#61107 = AXIS2_PLACEMENT_3D ( 'NONE', #30970, #43755, #8249 ) ;
#61108 = DIRECTION ( 'NONE',  ( 0.000000000000000000, 1.000000000000000000, 0.000000000000000000 ) ) ;
#61109 = CARTESIAN_POINT ( 'NONE',  ( -56.13160983291376738, -290.3794706047376053, -341.2740767488010079 ) ) ;
#61110 = CARTESIAN_POINT ( 'NONE',  ( -102.9125124544062260, -291.8046479014522561, -308.8636117106902361 ) ) ;
#61111 = CARTESIAN_POINT ( 'NONE',  ( -110.4695548327274253, -289.9258994683572155, -268.4508303017759658 ) ) ;
#61112 = CARTESIAN_POINT ( 'NONE',  ( -85.46953200798462547, -284.9144249481172437, -210.3341348700142817 ) ) ;
#61113 = CARTESIAN_POINT ( 'NONE',  ( 60.83289261295100658, -250.0118895884541530, 22.50000000000000000 ) ) ;
#61114 = CARTESIAN_POINT ( 'NONE',  ( 31.06856185501822765, -280.3187569898180982, -298.0464294114511858 ) ) ;
#61115 = CARTESIAN_POINT ( 'NONE',  ( -7.703931367187408341, -290.5200834829938685, -338.4783187292500770 ) ) ;
#61116 = CARTESIAN_POINT ( 'NONE',  ( -94.83800723505883923, -282.3865700833115966, -316.4776460841226822 ) ) ;
#61117 = CARTESIAN_POINT ( 'NONE',  ( 35.51944217815985638, -282.7363620315924777, -260.3658404532135933 ) ) ;
#61118 = CARTESIAN_POINT ( 'NONE',  ( 36.16356842236982061, -288.7725403371177322, -292.5381252622189550 ) ) ;
#61119 = VECTOR ( 'NONE', #70114, 1000.000000000000000 ) ;
#61120 = CARTESIAN_POINT ( 'NONE',  ( -108.6682003086464761, -279.2538075289531889, -254.4760374648383845 ) ) ;
#61121 = CARTESIAN_POINT ( 'NONE',  ( -92.51538155098648986, -290.0790488923523753, -217.1455390022598522 ) ) ;
#61122 = CARTESIAN_POINT ( 'NONE',  ( -110.5286180618309402, -285.0596027625623492, -293.8103408665072038 ) ) ;
#61123 = CARTESIAN_POINT ( 'NONE',  ( -12.72933335143210343, -286.8560923676025709, -197.4655879084660626 ) ) ;
#61124 = CARTESIAN_POINT ( 'NONE',  ( -82.79306352419723680, -283.8600878613000305, -327.5501751696892825 ) ) ;
#61125 = ORIENTED_EDGE ( 'NONE', *, *, #61083, .F. ) ;
#61126 = DIRECTION ( 'NONE',  ( 0.000000000000000000, 0.7071067811867438602, 0.7071067811863512853 ) ) ;
#61127 = CARTESIAN_POINT ( 'NONE',  ( -58.61493065692390303, -293.6403389697273383, -197.6441657562770615 ) ) ;
#61128 = TOROIDAL_SURFACE ( 'NONE', #67128, 16.36528803885689243, 1.000000000000000000 ) ;
#61129 = CARTESIAN_POINT ( 'NONE',  ( 32.87844883609535174, -291.8474731359370935, -239.9896025288758779 ) ) ;
#61130 = AXIS2_PLACEMENT_3D ( 'NONE', #28711, #63321, #50002 ) ;
#61131 = CARTESIAN_POINT ( 'NONE',  ( 32.73806904357483916, -274.8920971404298825, -291.6703697371067960 ) ) ;
#61132 = CARTESIAN_POINT ( 'NONE',  ( -110.7050425453647335, -295.6102657435727679, -293.4515254851738746 ) ) ;
#61133 = CARTESIAN_POINT ( 'NONE',  ( -9.447257154994359141, -290.9031850680901812, -202.0967877339206780 ) ) ;
#61134 = CARTESIAN_POINT ( 'NONE',  ( 20.47143900786562654, -292.4361053614398429, -316.5940276273177005 ) ) ;
#61135 = CARTESIAN_POINT ( 'NONE',  ( -22.67620711218559748, -293.4491472572595967, -198.4441254269270303 ) ) ;
#61136 = CARTESIAN_POINT ( 'NONE',  ( 199.7873597692581029, 25.48215708847424565, 10.49999999999999822 ) ) ;
#61137 = VECTOR ( 'NONE', #29912, 1000.000000000000000 ) ;
#61138 = CARTESIAN_POINT ( 'NONE',  ( 27.89738819161332017, -291.0551154101930251, -233.0262846567994188 ) ) ;
#61139 = CARTESIAN_POINT ( 'NONE',  ( 22.72937136620262777, -296.1659469225631938, -315.2873301167448403 ) ) ;
#61140 = CARTESIAN_POINT ( 'NONE',  ( 30.70824988230531716, -288.8560226751339428, -297.5647694007143969 ) ) ;
#61141 = CARTESIAN_POINT ( 'NONE',  ( -38.49397032642803396, -279.0464212675569229, -345.7075119251946944 ) ) ;
#61142 = CARTESIAN_POINT ( 'NONE',  ( -82.32556824998403044, -276.4460758600843064, -332.3648301806337031 ) ) ;
#61143 = VECTOR ( 'NONE', #15760, 1000.000000000000000 ) ;
#61144 = CARTESIAN_POINT ( 'NONE',  ( -26.22845828252329525, -297.3851421146307530, -193.5240625362837363 ) ) ;
#61145 = CARTESIAN_POINT ( 'NONE',  ( -11.21528089560723274, -278.4749786837091960, -200.6020470126230464 ) ) ;
#61146 = CARTESIAN_POINT ( 'NONE',  ( -111.0587526299876515, -276.7074067776957804, -289.7058756206711791 ) ) ;
#61147 = CARTESIAN_POINT ( 'NONE',  ( -107.1701259474203596, -295.5410148275258848, -247.2819022478191471 ) ) ;
#61148 = CARTESIAN_POINT ( 'NONE',  ( -109.1683679093899144, -274.8324875907955516, -248.5990953173099456 ) ) ;
#61149 = CARTESIAN_POINT ( 'NONE',  ( -65.86055204674019592, -274.3203211373043473, -203.0516256829406814 ) ) ;
#61150 = LINE ( 'NONE', #2893, #35291 ) ;
#61152 = CARTESIAN_POINT ( 'NONE',  ( 33.50969327064054681, -275.1534774108990860, -252.7804451287752272 ) ) ;
#61151 = CARTESIAN_POINT ( 'NONE',  ( -67.42099764189555344, -287.4648311380520909, -339.4526707679829087 ) ) ;
#61153 = CARTESIAN_POINT ( 'NONE',  ( 38.55686124440615004, -287.3888839710847947, -257.3063253781451749 ) ) ;
#61154 = CARTESIAN_POINT ( 'NONE',  ( 17.85844122611258911, -300.7197990699097545, -194.9873902654363746 ) ) ;
#61155 = CARTESIAN_POINT ( 'NONE',  ( -97.08293841898321830, -293.9342288339367997, -315.4489961794517967 ) ) ;
#61156 = CARTESIAN_POINT ( 'NONE',  ( -104.2813765694811536, -283.2575490106374332, -308.1947425455101666 ) ) ;
#61157 = CARTESIAN_POINT ( 'NONE',  ( 73.43068321062709458, -134.2391364535880598, -5.025000000000002132 ) ) ;
#61158 = CARTESIAN_POINT ( 'NONE',  ( -2.901071364674446595, -278.5071072935193683, -203.7222381759013956 ) ) ;
#61159 = CARTESIAN_POINT ( 'NONE',  ( 204.4184720700929745, 287.8409256575666859, -5.149838471383963778 ) ) ;
#61160 = CARTESIAN_POINT ( 'NONE',  ( -110.7039167626998193, -289.3004684929671839, -273.9129526877747480 ) ) ;
#61161 = DIRECTION ( 'NONE',  ( -0.1455045995357750477, -0.000000000000000000, -0.9893575751536620722 ) ) ;
#61162 = CARTESIAN_POINT ( 'NONE',  ( -38.91467087911562572, -290.0322565414983274, -195.3776103601423699 ) ) ;
#61163 = CARTESIAN_POINT ( 'NONE',  ( -1.401246139056952167, -276.0580396519193869, -206.0116758496154716 ) ) ;
#61164 = CARTESIAN_POINT ( 'NONE',  ( 33.03041228520542205, -283.3607774926060756, -300.2683200310597726 ) ) ;
#61165 = ADVANCED_FACE ( 'NONE', ( #81742 ), #27582, .T. ) ;
#61167 = CARTESIAN_POINT ( 'NONE',  ( -29.44465309213074988, -282.9494795944524412, -342.9832183258961891 ) ) ;
#61166 = CARTESIAN_POINT ( 'NONE',  ( -112.9017001288127773, -270.6323071252278396, -270.3367248692900375 ) ) ;
#61168 = CARTESIAN_POINT ( 'NONE',  ( -40.82082042459323645, -275.4329483492452368, -196.8040741209401574 ) ) ;
#61169 = CARTESIAN_POINT ( 'NONE',  ( 35.74770136578801782, -276.2991583901867898, -266.1194408566408356 ) ) ;
#61170 = CARTESIAN_POINT ( 'NONE',  ( 30.59192902350789467, -283.9714973125862798, -302.2644155037862106 ) ) ;
#61171 = ORIENTED_EDGE ( 'NONE', *, *, #38735, .T. ) ;
#61172 = CARTESIAN_POINT ( 'NONE',  ( 203.2340568605973772, 295.9509986211770638, -54.00000000006198064 ) ) ;
#61173 = CARTESIAN_POINT ( 'NONE',  ( -30.59306562501696902, -294.8023632282826725, -347.0648071822886322 ) ) ;
#61174 = CARTESIAN_POINT ( 'NONE',  ( -94.53116604107296439, -287.1982117339554748, -222.3901705825836927 ) ) ;
#61175 = DIRECTION ( 'NONE',  ( 0.000000000000000000, 0.000000000000000000, -1.000000000000000000 ) ) ;
#61176 = CARTESIAN_POINT ( 'NONE',  ( -117.3452863284742733, -275.1604526064901393, -261.3791111993605227 ) ) ;
#61177 = CARTESIAN_POINT ( 'NONE',  ( -96.03248285041129861, -277.0795735837839970, -319.9752884853033947 ) ) ;
#61178 = CARTESIAN_POINT ( 'NONE',  ( -88.96463199667282140, -288.1633067178807437, -326.4103224293067456 ) ) ;
#61179 = CARTESIAN_POINT ( 'NONE',  ( -52.24791192551646901, -287.3779483856088746, -198.1910923459612661 ) ) ;
#61180 = CARTESIAN_POINT ( 'NONE',  ( -89.78827780428588312, -279.5644231429540127, -322.6577223796755902 ) ) ;
#61181 = CARTESIAN_POINT ( 'NONE',  ( -21.12683496526869575, -287.6815331340808939, -195.6906121650895614 ) ) ;
#61182 = CARTESIAN_POINT ( 'NONE',  ( 31.85726556961443379, -283.1746699740484701, -241.4387426918657980 ) ) ;
#61183 = CARTESIAN_POINT ( 'NONE',  ( 39.70741351921355999, -275.7289421212855700, -271.1695245178572691 ) ) ;
#61184 = CARTESIAN_POINT ( 'NONE',  ( -112.7940561520883591, -278.1925549419570984, -285.7866900977512614 ) ) ;
#61185 = CARTESIAN_POINT ( 'NONE',  ( -111.6784197933859275, -298.4216015120937300, -274.2811058297753561 ) ) ;
#61186 = AXIS2_PLACEMENT_3D ( 'NONE', #5782, #20917, #55970 ) ;
#61187 = CARTESIAN_POINT ( 'NONE',  ( 156.3365481965859374, 16.61859728808323666, 10.14856962220773617 ) ) ;
#61188 = ADVANCED_FACE ( 'NONE', ( #52864 ), #16892, .T. ) ;
#61189 = CARTESIAN_POINT ( 'NONE',  ( -112.3417001280813849, -275.0519495502701943, -270.3929463913696054 ) ) ;
#61190 = CARTESIAN_POINT ( 'NONE',  ( 96.48985628060853514, -297.8500639586717966, -194.6381542544558840 ) ) ;
#61191 = DIRECTION ( 'NONE',  ( -1.000000000000000000, 0.000000000000000000, 0.000000000000000000 ) ) ;
#61192 = CARTESIAN_POINT ( 'NONE',  ( -83.05013735437303524, -277.2047449216918267, -327.4238423791767900 ) ) ;
#61193 = CARTESIAN_POINT ( 'NONE',  ( -93.86271078175940374, -274.4642613820264501, -218.6369681025128955 ) ) ;
#61194 = CARTESIAN_POINT ( 'NONE',  ( 36.76103030286353857, -280.3586051216105943, -250.2711410957494422 ) ) ;
#61195 = CARTESIAN_POINT ( 'NONE',  ( 34.69142250384854265, -289.0903158901492702, -253.3004363684986799 ) ) ;
#61196 = CARTESIAN_POINT ( 'NONE',  ( -112.9628185808622192, -297.9386015700267194, -280.9529787642888436 ) ) ;
#61197 = CARTESIAN_POINT ( 'NONE',  ( -53.19202163374237813, -296.4559739928315025, -345.3605309012414182 ) ) ;
#61198 = ADVANCED_FACE ( 'NONE', ( #83137 ), #83508, .T. ) ;
#61199 = CARTESIAN_POINT ( 'NONE',  ( 7.761443472523162690, -294.6698512498923037, -210.6473435179227067 ) ) ;
#61200 = CARTESIAN_POINT ( 'NONE',  ( -65.48249506226881067, -277.6832125685359642, -201.0204799113909928 ) ) ;
#61201 = CARTESIAN_POINT ( 'NONE',  ( 16.28001923175133570, -282.7404475058839921, -218.6539394991268921 ) ) ;
#61202 = CARTESIAN_POINT ( 'NONE',  ( -50.17867404431141409, -295.9668801133246916, -197.0363179762350114 ) ) ;
#61203 = CARTESIAN_POINT ( 'NONE',  ( -73.87433644447233405, -285.1287193937960183, -337.2915549751027129 ) ) ;
#61204 = CONICAL_SURFACE ( 'NONE', #14374, 4.000000000000003553, 1.029744258676654534 ) ;
#61205 = CARTESIAN_POINT ( 'NONE',  ( 22.25085615772718839, -285.8772262047522190, -227.5794554563788381 ) ) ;
#61206 = CARTESIAN_POINT ( 'NONE',  ( 162.8811038778437421, 219.0089487911489812, -204.8009164393295123 ) ) ;
#61207 = ORIENTED_EDGE ( 'NONE', *, *, #22793, .F. ) ;
#61208 = CARTESIAN_POINT ( 'NONE',  ( 29.98291127326664451, -286.8380113863557312, -241.9550033858817528 ) ) ;
#61209 = VERTEX_POINT ( 'NONE', #31115 ) ;
#61210 = CARTESIAN_POINT ( 'NONE',  ( -69.04606380591251025, -284.5390704959723394, -340.2061668788211364 ) ) ;
#61211 = CARTESIAN_POINT ( 'NONE',  ( 19.01246479769613273, -275.2275219379220630, -223.9251881180274495 ) ) ;
#61212 = CARTESIAN_POINT ( 'NONE',  ( -30.90186084065257788, -284.9267281581383600, -194.0161342613318425 ) ) ;
#61213 = CARTESIAN_POINT ( 'NONE',  ( -69.48102541539080335, -290.5593684631805331, -200.7152596714730635 ) ) ;
#61214 = CARTESIAN_POINT ( 'NONE',  ( 1.245296188414876104, -281.4951930970142939, -203.9389880269300477 ) ) ;
#61215 = CARTESIAN_POINT ( 'NONE',  ( 196.8803347170859865, 20.19615242270662847, -12.49999999999999289 ) ) ;
#61216 = CARTESIAN_POINT ( 'NONE',  ( -102.8266319910048452, -280.5888348872528013, -231.0865159685884578 ) ) ;
#61217 = CARTESIAN_POINT ( 'NONE',  ( 38.12565972344505383, -282.0753262874368943, -285.5407717551344149 ) ) ;
#61218 = CARTESIAN_POINT ( 'NONE',  ( 7.450504543161054372, -284.1952119285919025, -214.2458315076590907 ) ) ;
#61219 = CARTESIAN_POINT ( 'NONE',  ( -107.3199604355249051, -262.9330320181824732, -317.7331714456881286 ) ) ;
#61220 = VERTEX_POINT ( 'NONE', #68960 ) ;
#61221 = CARTESIAN_POINT ( 'NONE',  ( 35.91084419087310664, -277.3546180294409282, -254.9985571154810771 ) ) ;
#61222 = CARTESIAN_POINT ( 'NONE',  ( -104.9347473080156163, -255.2955550898405193, -326.2820073762666766 ) ) ;
#61223 = CARTESIAN_POINT ( 'NONE',  ( 34.90934673734872007, -279.8149557726275702, -289.1638438378815863 ) ) ;
#61224 = CARTESIAN_POINT ( 'NONE',  ( -32.06026631913207581, -296.7465544766477024, -346.1771035322989860 ) ) ;
#61225 = CARTESIAN_POINT ( 'NONE',  ( -94.02684526694497436, -295.2480743567660966, -316.5401590733378612 ) ) ;
#61226 = CARTESIAN_POINT ( 'NONE',  ( -96.52750866996859713, -290.7215602056205626, -221.1821706045000155 ) ) ;
#61227 = CARTESIAN_POINT ( 'NONE',  ( 160.5350683151633291, 249.5000000000000568, 20.22542485937379908 ) ) ;
#61229 = CARTESIAN_POINT ( 'NONE',  ( 29.54350030742865485, -285.5354398154176465, -239.1712097474611767 ) ) ;
#61228 = CARTESIAN_POINT ( 'NONE',  ( -113.3588826612229639, -295.0292658904818950, -278.1067136155596700 ) ) ;
#61230 = CARTESIAN_POINT ( 'NONE',  ( 33.53302600010901813, -295.7003214018989752, -292.4436603379149915 ) ) ;
#61231 = CARTESIAN_POINT ( 'NONE',  ( -9.320762240904400642, -287.7414342166643451, -202.4058504348868723 ) ) ;
#61232 = EDGE_LOOP ( 'NONE', ( #31379, #49116, #4562, #1694 ) ) ;
#61233 = CARTESIAN_POINT ( 'NONE',  ( 39.20553797929906636, -294.4209674763781663, -264.5869902942046679 ) ) ;
#61234 = CARTESIAN_POINT ( 'NONE',  ( -97.57953334127418543, -284.4683925823658797, -311.7940750023726650 ) ) ;
#61235 = CARTESIAN_POINT ( 'NONE',  ( -112.4961179033775522, -295.5343145222853423, -255.4673260894332429 ) ) ;
#61236 = CARTESIAN_POINT ( 'NONE',  ( -103.0829987075748448, -291.8763781031692588, -230.4811240711913456 ) ) ;
#61237 = CARTESIAN_POINT ( 'NONE',  ( -101.6359888281575365, -291.6015297351016216, -228.0071148928085165 ) ) ;
#61238 = CARTESIAN_POINT ( 'NONE',  ( -108.3499231793004327, -290.4953967718241756, -287.2972410231224671 ) ) ;
#61239 = ORIENTED_EDGE ( 'NONE', *, *, #8590, .F. ) ;
#61240 = CARTESIAN_POINT ( 'NONE',  ( 82.64890176555634582, -299.5541904835127980, -197.7570935515975918 ) ) ;
#61241 = CARTESIAN_POINT ( 'NONE',  ( -36.92950625991289115, -299.9176694314135716, -194.5961815503768548 ) ) ;
#61242 = CARTESIAN_POINT ( 'NONE',  ( -113.1490700837806003, -271.4900487068189250, -258.9884009044006348 ) ) ;
#61243 = CARTESIAN_POINT ( 'NONE',  ( 33.99229161686636758, -280.3928902655889033, -253.7819120100527357 ) ) ;
#61244 = ORIENTED_EDGE ( 'NONE', *, *, #56056, .F. ) ;
#61245 = CARTESIAN_POINT ( 'NONE',  ( 39.56951231019630200, -275.0341785101417145, -268.3136062407267559 ) ) ;
#61246 = CARTESIAN_POINT ( 'NONE',  ( -109.8275895882569131, -294.8575033894813373, -283.7165863621206654 ) ) ;
#61247 = CARTESIAN_POINT ( 'NONE',  ( -54.21199183059562188, -279.1313864684050259, -342.7070051932167871 ) ) ;
#61248 = CARTESIAN_POINT ( 'NONE',  ( 35.59139518428406745, -273.5121605587906970, -256.5181020326321004 ) ) ;
#61249 = CARTESIAN_POINT ( 'NONE',  ( -110.1320633464270173, -297.8858419255379317, -260.5588414901434362 ) ) ;
#61250 = CARTESIAN_POINT ( 'NONE',  ( -66.95676868256512648, -298.7343323176042418, -203.2864081614265217 ) ) ;
#61251 = CARTESIAN_POINT ( 'NONE',  ( -72.92537711763402797, -299.1892153442483959, -202.9215531611147298 ) ) ;
#61252 = CARTESIAN_POINT ( 'NONE',  ( -46.65223985163488862, -271.9546172902489047, -195.5833094340492551 ) ) ;
#61253 = CARTESIAN_POINT ( 'NONE',  ( 35.00743672500120596, -294.0657235268195109, -259.8971290277253843 ) ) ;
#61254 = CARTESIAN_POINT ( 'NONE',  ( -0.9496202824729688130, -291.1200860321305868, -206.3856654188712412 ) ) ;
#61255 = CARTESIAN_POINT ( 'NONE',  ( -23.40286736638519471, -134.2391364535880598, -21.50000000000000000 ) ) ;
#61256 = ADVANCED_FACE ( 'NONE', ( #82681 ), #44181, .T. ) ;
#61257 = CARTESIAN_POINT ( 'NONE',  ( 33.65433975390517674, -275.6655776260096786, -240.5741054012914333 ) ) ;
#61258 = CARTESIAN_POINT ( 'NONE',  ( -37.15381829456106999, -298.3878581469235769, -197.3371132438529685 ) ) ;
#61259 = CARTESIAN_POINT ( 'NONE',  ( 37.99514284250686558, -283.4904078664116014, -267.1028007542923888 ) ) ;
#61260 = CARTESIAN_POINT ( 'NONE',  ( -67.70116118732174471, -282.1271301440829689, -340.5864794834035933 ) ) ;
#61261 = CYLINDRICAL_SURFACE ( 'NONE', #65721, 4.999999999999990230 ) ;
#61262 = CARTESIAN_POINT ( 'NONE',  ( -73.88629885156321109, -282.7476298618543638, -333.7994023444343838 ) ) ;
#61263 = AXIS2_PLACEMENT_3D ( 'NONE', #89893, #81858, #17007 ) ;
#61264 = CARTESIAN_POINT ( 'NONE',  ( -82.79533508452522028, -281.6714023077923343, -330.2929990674005012 ) ) ;
#61265 = CARTESIAN_POINT ( 'NONE',  ( 34.73807216750496707, -274.3209220712727756, -285.1895145423513327 ) ) ;
#61266 = CARTESIAN_POINT ( 'NONE',  ( -34.79805432837309809, -282.0841675863708247, -195.3541177916236222 ) ) ;
#61267 = CARTESIAN_POINT ( 'NONE',  ( 211.1232656141943949, 1.000000000000000888, 7.000000000000000000 ) ) ;
#61268 = LINE ( 'NONE', #61716, #495 ) ;
#61269 = CARTESIAN_POINT ( 'NONE',  ( -83.08342137367077385, -271.8379385012563034, -209.3513851557187309 ) ) ;
#61270 = CARTESIAN_POINT ( 'NONE',  ( -100.5413933777107900, -280.0042594206789772, -311.1479043380187477 ) ) ;
#61271 = DIRECTION ( 'NONE',  ( 0.000000000000000000, 0.000000000000000000, 1.000000000000000000 ) ) ;
#61272 = CARTESIAN_POINT ( 'NONE',  ( -92.87827025563065320, -287.1838003544532398, -219.0496198482255181 ) ) ;
#61273 = ORIENTED_EDGE ( 'NONE', *, *, #32523, .F. ) ;
#61274 = CARTESIAN_POINT ( 'NONE',  ( 208.1426553406905953, 36.40695478883779401, 14.84194439653754394 ) ) ;
#61275 = CARTESIAN_POINT ( 'NONE',  ( 23.62112409745348174, -286.1473191155689619, -314.1341037901555637 ) ) ;
#61276 = AXIS2_PLACEMENT_3D ( 'NONE', #79954, #87499, #22648 ) ;
#61277 = LINE ( 'NONE', #55085, #16486 ) ;
#61278 = CARTESIAN_POINT ( 'NONE',  ( -108.8605086271576994, -295.5635368191865950, -253.8629199863998167 ) ) ;
#61279 = CARTESIAN_POINT ( 'NONE',  ( -26.31441578364136902, -287.0500409453898669, -343.8246395955183061 ) ) ;
#61280 = CARTESIAN_POINT ( 'NONE',  ( 154.8793480878648268, 20.01712742761865371, -11.60576973086971542 ) ) ;
#61281 = CARTESIAN_POINT ( 'NONE',  ( -103.2363275121843742, -294.0761666386493971, -306.1786936673113928 ) ) ;
#61282 = CARTESIAN_POINT ( 'NONE',  ( -7.595381012763462891, -284.9148164410742083, -200.0350266332745264 ) ) ;
#61283 = CARTESIAN_POINT ( 'NONE',  ( 18.55729277409077937, -282.4732417805408318, -222.1572573345381159 ) ) ;
#61284 = CARTESIAN_POINT ( 'NONE',  ( -91.72436864482629915, -282.0543659227286639, -323.4318196740168787 ) ) ;
#61285 = CARTESIAN_POINT ( 'NONE',  ( -3.366371430787300500, -288.5907394986638224, -335.0288430176313454 ) ) ;
#61286 = CARTESIAN_POINT ( 'NONE',  ( -74.82139689060470289, -280.9683005205362178, -206.9728690477283521 ) ) ;
#61287 = CARTESIAN_POINT ( 'NONE',  ( -41.06961524653080176, -280.8068708255669890, -197.2946798859501030 ) ) ;
#61288 = CARTESIAN_POINT ( 'NONE',  ( 17.14440229512996794, -288.8039296238887346, -218.2313875354229822 ) ) ;
#61289 = CARTESIAN_POINT ( 'NONE',  ( -87.46387014799482529, -297.5422283037543139, -211.8377003311239832 ) ) ;
#61290 = VERTEX_POINT ( 'NONE', #53333 ) ;
#61291 = CARTESIAN_POINT ( 'NONE',  ( -66.22722039019882345, -273.6843462982731694, -198.9702939169441436 ) ) ;
#61292 = CARTESIAN_POINT ( 'NONE',  ( -11.71876487408031942, -294.3671831855201049, -200.1967479695250915 ) ) ;
#61293 = CARTESIAN_POINT ( 'NONE',  ( 139.6925840978351232, -135.2391364535880882, 22.50000000000000000 ) ) ;
#61294 = CARTESIAN_POINT ( 'NONE',  ( 10.64812456238590066, -278.9090924074130839, -330.4860931364851808 ) ) ;
#61295 = EDGE_LOOP ( 'NONE', ( #47913, #4968, #82348, #88786 ) ) ;
#61296 = CARTESIAN_POINT ( 'NONE',  ( 9.366427474328158809, -274.4122399590690975, -329.3205112761508531 ) ) ;
#61297 = CARTESIAN_POINT ( 'NONE',  ( 208.6208076322478746, 32.98517505407394168, 12.09245862095555601 ) ) ;
#61298 = CARTESIAN_POINT ( 'NONE',  ( -40.38765757333001716, -296.4144736929819146, -194.1704320683369360 ) ) ;
#61299 = CARTESIAN_POINT ( 'NONE',  ( -5.255838620602536260, -273.8345196278169169, -204.6632560731589479 ) ) ;
#61300 = CARTESIAN_POINT ( 'NONE',  ( -100.3140262802480578, -292.5944743208195291, -232.0832668081976919 ) ) ;
#61301 = CARTESIAN_POINT ( 'NONE',  ( -0.7315389881543790107, -284.3188441072293244, -334.6858419652319299 ) ) ;
#61302 = CARTESIAN_POINT ( 'NONE',  ( -111.4277742342994770, -292.2138600974926703, -251.6038216787700037 ) ) ;
#61303 = CARTESIAN_POINT ( 'NONE',  ( -106.8196575601372160, -292.2811587237740127, -238.2018574513158455 ) ) ;
#61304 = CARTESIAN_POINT ( 'NONE',  ( -42.39184327807954844, -294.9509342211956664, -343.1862239466129267 ) ) ;
#61305 = CARTESIAN_POINT ( 'NONE',  ( 35.94504206854879413, -289.3476537100062274, -254.4220442554704960 ) ) ;
#61306 = CARTESIAN_POINT ( 'NONE',  ( 21.06471466625051292, -281.0413661851348479, -220.1644744070667628 ) ) ;
#61307 = CARTESIAN_POINT ( 'NONE',  ( -112.5131537814035596, -294.5344638699883717, -278.0140097385419153 ) ) ;
#61308 = CARTESIAN_POINT ( 'NONE',  ( -4.165758162109444385, -282.4600952944311416, -339.8619859655595974 ) ) ;
#61309 = CARTESIAN_POINT ( 'NONE',  ( 37.22871072067736264, -277.4760285213617976, -266.0187067795313851 ) ) ;
#61310 = EDGE_CURVE ( 'NONE', #12065, #83022, #68486, .T. ) ;
#61311 = CARTESIAN_POINT ( 'NONE',  ( -25.97897899706188696, -275.0485102041932919, -345.2690217507361012 ) ) ;
#61312 = DIRECTION ( 'NONE',  ( 0.000000000000000000, 0.000000000000000000, -1.000000000000000000 ) ) ;
#61313 = CARTESIAN_POINT ( 'NONE',  ( -48.34413205242784528, -282.7036278771045090, -342.5894706792235525 ) ) ;
#61314 = CARTESIAN_POINT ( 'NONE',  ( -82.01977402536080319, -280.6629638597428311, -208.1366980945376213 ) ) ;
#61315 = CARTESIAN_POINT ( 'NONE',  ( 22.21498129637733854, -287.2629107389572596, -318.8154868346142621 ) ) ;
#61316 = CARTESIAN_POINT ( 'NONE',  ( -19.85417759692977313, -294.0400414178182018, -198.3903920338735247 ) ) ;
#61317 = CARTESIAN_POINT ( 'NONE',  ( 17.49953028613967021, -276.4195405220847874, -217.3809546641495558 ) ) ;
#61318 = CARTESIAN_POINT ( 'NONE',  ( 38.64980932666259861, -276.9845087851921335, -279.6711557744969241 ) ) ;
#61319 = CARTESIAN_POINT ( 'NONE',  ( -71.65606146089955075, -277.3521719186881569, -334.8075436313520186 ) ) ;
#61320 = CARTESIAN_POINT ( 'NONE',  ( -78.54207375752608300, -299.4966662501169594, -207.8283818438405035 ) ) ;
#61321 = CARTESIAN_POINT ( 'NONE',  ( -90.95908084453942877, -283.2891324060518627, -218.0832887304998735 ) ) ;
#61322 = CARTESIAN_POINT ( 'NONE',  ( 38.83160638164084588, -293.0754463219067247, -258.8960487176551055 ) ) ;
#61323 = CARTESIAN_POINT ( 'NONE',  ( -51.51630576280037843, -290.8306627055935678, -345.2311451536955360 ) ) ;
#61324 = CARTESIAN_POINT ( 'NONE',  ( -30.76561074184070321, -291.0575578014143048, -197.3475499146429399 ) ) ;
#61325 = ORIENTED_EDGE ( 'NONE', *, *, #63388, .T. ) ;
#61326 = CARTESIAN_POINT ( 'NONE',  ( 3.839378203651969024, -291.1692602114912916, -205.9343876785895020 ) ) ;
#61327 = CARTESIAN_POINT ( 'NONE',  ( 12.92078424213064913, -292.4444249347257596, -217.3915970138668001 ) ) ;
#61328 = ORIENTED_EDGE ( 'NONE', *, *, #59496, .T. ) ;
#61329 = CARTESIAN_POINT ( 'NONE',  ( -37.48714727442480665, -290.1335623523838763, -347.0648889991185229 ) ) ;
#61330 = CARTESIAN_POINT ( 'NONE',  ( -110.4534051396120446, -279.2358177885050168, -267.9131134802931342 ) ) ;
#61331 = ADVANCED_FACE ( 'NONE', ( #82219 ), #23991, .F. ) ;
#61332 = CARTESIAN_POINT ( 'NONE',  ( -99.66230709163096435, -296.0671678049372986, -225.6662138221333294 ) ) ;
#61333 = CARTESIAN_POINT ( 'NONE',  ( -43.66616751021834375, -286.6257701435818035, -193.6703801939447374 ) ) ;
#61334 = CARTESIAN_POINT ( 'NONE',  ( -3.502480597322533917, -286.8199143526628063, -201.2043388997380191 ) ) ;
#61335 = CARTESIAN_POINT ( 'NONE',  ( -90.75403265264685615, -284.1695977731365019, -320.1527861718582813 ) ) ;
#61336 = CARTESIAN_POINT ( 'NONE',  ( 5.351633954136511662, -58.18680328362809462, -354.6685698517738956 ) ) ;
#61337 = CARTESIAN_POINT ( 'NONE',  ( 178.3994555490664595, 253.9822658848526657, -165.8744343721958785 ) ) ;
#61338 = CARTESIAN_POINT ( 'NONE',  ( -110.4036248592226883, -268.2063041062111779, -295.2719097700364159 ) ) ;
#61339 = ADVANCED_FACE ( 'NONE', ( #2693 ), #60464, .T. ) ;
#61340 = PRODUCT_DEFINITION_FORMATION_WITH_SPECIFIED_SOURCE ( 'ANY', '', #28567, .NOT_KNOWN. ) ;
#61341 = CARTESIAN_POINT ( 'NONE',  ( -64.40235718648879981, -276.6116120984796680, -338.3878774470868507 ) ) ;
#61342 = CARTESIAN_POINT ( 'NONE',  ( -1.330328075974988478, -275.4832278153446623, -334.2731347728691844 ) ) ;
#61343 = CARTESIAN_POINT ( 'NONE',  ( -51.78291062434480807, -297.3799286863383600, -194.7358077258001003 ) ) ;
#61344 = CARTESIAN_POINT ( 'NONE',  ( -54.25878813547573287, -170.2527245721807674, -361.3251189563821981 ) ) ;
#61345 = CARTESIAN_POINT ( 'NONE',  ( -92.98689987490215003, -276.5147790370451162, -322.9434431916723156 ) ) ;
#61346 = CARTESIAN_POINT ( 'NONE',  ( -98.69559955160239895, -274.8808547389016326, -228.8731122167084493 ) ) ;
#61347 = ORIENTED_EDGE ( 'NONE', *, *, #40483, .T. ) ;
#61348 = VECTOR ( 'NONE', #63807, 1000.000000000000000 ) ;
#61349 = CARTESIAN_POINT ( 'NONE',  ( -110.1834597593814351, -290.9617243231936072, -276.6414324256516011 ) ) ;
#61350 = CARTESIAN_POINT ( 'NONE',  ( -29.09146248775674692, -298.9558089973359074, -193.5215010717849964 ) ) ;
#61351 = CARTESIAN_POINT ( 'NONE',  ( -112.5416896459395417, -297.2487730923247113, -254.0365000909214359 ) ) ;
#61352 = CARTESIAN_POINT ( 'NONE',  ( -67.29326840376492669, -295.6228645130847781, -336.9473674665405838 ) ) ;
#61353 = ORIENTED_EDGE ( 'NONE', *, *, #77868, .T. ) ;
#61354 = CARTESIAN_POINT ( 'NONE',  ( -109.2878775550504429, -280.1745326767582469, -293.6175345735392739 ) ) ;
#61355 = CARTESIAN_POINT ( 'NONE',  ( -8.068112327127085592, -282.1866345898757231, -341.5694470780718461 ) ) ;
#61356 = CARTESIAN_POINT ( 'NONE',  ( -41.85916117406565462, -278.0516909924560878, -343.4695893313004262 ) ) ;
#61357 = CARTESIAN_POINT ( 'NONE',  ( 38.61161238814129604, -277.3580691624371752, -273.9731442986214347 ) ) ;
#61358 = CARTESIAN_POINT ( 'NONE',  ( -111.0343129463638547, -271.0682070554903476, -267.5920783070110360 ) ) ;
#61359 = CARTESIAN_POINT ( 'NONE',  ( 151.6573119020006288, 20.00000000000000000, -4.897109440893268939 ) ) ;
#61360 = CARTESIAN_POINT ( 'NONE',  ( -100.5817726090219963, -278.2176230215943065, -306.9275952081090395 ) ) ;
#61361 = CARTESIAN_POINT ( 'NONE',  ( -13.12309273342502003, -275.1618187473196713, -197.4391194084294625 ) ) ;
#61362 = CARTESIAN_POINT ( 'NONE',  ( 35.90836172644844737, -286.5164785535055785, -292.4911209200318467 ) ) ;
#61363 = CARTESIAN_POINT ( 'NONE',  ( -73.01659179066888328, -275.5799314223348802, -204.3313919983325491 ) ) ;
#61364 = CARTESIAN_POINT ( 'NONE',  ( 21.26691320780884453, -274.7917814940661287, -319.3880160849798813 ) ) ;
#61365 = DIRECTION ( 'NONE',  ( 0.000000000000000000, -0.000000000000000000, -1.000000000000000000 ) ) ;
#61366 = CARTESIAN_POINT ( 'NONE',  ( -90.71755185143608458, -289.0302182399763069, -320.4713006811011837 ) ) ;
#61367 = CARTESIAN_POINT ( 'NONE',  ( -113.7174336871463396, -284.0127916790894460, -261.4134864651146017 ) ) ;
#61368 = CARTESIAN_POINT ( 'NONE',  ( 3.937045986351015880, -280.7281057818884733, -331.8563086408301501 ) ) ;
#61370 = CARTESIAN_POINT ( 'NONE',  ( -111.7479600948059328, -282.6609840543524683, -268.1199859514173909 ) ) ;
#61369 = CARTESIAN_POINT ( 'NONE',  ( 29.51554515754934727, -279.7139326480127579, -239.4902141343162612 ) ) ;
#61371 = CARTESIAN_POINT ( 'NONE',  ( 18.45970729333602023, -290.2506100977726078, -320.4919304166546112 ) ) ;
#61372 = CARTESIAN_POINT ( 'NONE',  ( -101.1646098885806708, -280.2509444133464740, -234.1151982997666039 ) ) ;
#61373 = FACE_OUTER_BOUND ( 'NONE', #65387, .T. ) ;
#61374 = CARTESIAN_POINT ( 'NONE',  ( 23.12505890027613731, -279.3267916984418662, -223.9694224978204602 ) ) ;
#61375 = CARTESIAN_POINT ( 'NONE',  ( -19.87785883529945963, -294.2766665372810735, -197.3692922573578414 ) ) ;
#61376 = CARTESIAN_POINT ( 'NONE',  ( -96.02041585157451209, -277.4494121126649588, -222.0627145472533073 ) ) ;
#61377 = CARTESIAN_POINT ( 'NONE',  ( -45.91182601263462715, -277.8149640871089332, -343.0096489186244071 ) ) ;
#61378 = CARTESIAN_POINT ( 'NONE',  ( -68.40499038298966639, -285.4594106739762083, -338.8229797264590388 ) ) ;
#61379 = LINE ( 'NONE', #40940, #5056 ) ;
#61380 = CARTESIAN_POINT ( 'NONE',  ( -68.73626708208199432, -291.3817169367707720, -339.1044142728047177 ) ) ;
#61381 = CARTESIAN_POINT ( 'NONE',  ( 36.98561309977826994, -286.9937232199565642, -289.8446836032106262 ) ) ;
#61382 = CARTESIAN_POINT ( 'NONE',  ( -94.04153049951951004, -289.6152080190131528, -223.1019042607424865 ) ) ;
#61383 = CARTESIAN_POINT ( 'NONE',  ( -48.18343439336755551, -268.6864615527640012, -433.8888687766993826 ) ) ;
#61384 = CARTESIAN_POINT ( 'NONE',  ( 33.99185867087999213, -274.0051692665829819, -252.6759018827022771 ) ) ;
#61385 = CARTESIAN_POINT ( 'NONE',  ( -7.513373677495008174, -292.7964785155708682, -338.3538637370785409 ) ) ;
#61386 = SURFACE_SIDE_STYLE ('',( #61835 ) ) ;
#61387 = FACE_OUTER_BOUND ( 'NONE', #49644, .T. ) ;
#61388 = CARTESIAN_POINT ( 'NONE',  ( 17.00948576330940298, -291.2891394793577433, -216.7268545940153217 ) ) ;
#61389 = CARTESIAN_POINT ( 'NONE',  ( -84.17106336680740242, -286.9962781486806875, -213.2556727458677130 ) ) ;
#61390 = CARTESIAN_POINT ( 'NONE',  ( 22.47570041525208140, -286.4269637230739818, -317.2419871467597545 ) ) ;
#61391 = EDGE_CURVE ( 'NONE', #63080, #39909, #80477, .T. ) ;
#61392 = CARTESIAN_POINT ( 'NONE',  ( -40.01334061122588537, -287.4432019572795980, -196.8203996320497708 ) ) ;
#61393 = CARTESIAN_POINT ( 'NONE',  ( 115.2448031289451222, -299.5541904835127980, -198.8526868767648352 ) ) ;
#61394 = CARTESIAN_POINT ( 'NONE',  ( 33.54247527635438075, -288.1158489833282488, -252.1988328905676724 ) ) ;
#61395 = CARTESIAN_POINT ( 'NONE',  ( 37.60405666649064216, -295.6384516039051960, -278.6875295515017115 ) ) ;
#61396 = CARTESIAN_POINT ( 'NONE',  ( -95.06524177541561471, -275.9624327789842368, -319.1387311271998328 ) ) ;
#61397 = CARTESIAN_POINT ( 'NONE',  ( -87.07829578468785314, -278.0559330804764500, -329.1847129839409263 ) ) ;
#61398 = CARTESIAN_POINT ( 'NONE',  ( -50.29499807841217773, -289.9678772898131456, -195.9196895457591268 ) ) ;
#61399 = CARTESIAN_POINT ( 'NONE',  ( -64.74232811921139330, -279.7041910848450357, -198.3451387244329283 ) ) ;
#61400 = CARTESIAN_POINT ( 'NONE',  ( -35.79761705321728726, -300.0514629402524065, -195.7157852367089390 ) ) ;
#61401 = CARTESIAN_POINT ( 'NONE',  ( -43.46186634799974513, -256.7147672836524066, -495.8094554426511991 ) ) ;
#61402 = CARTESIAN_POINT ( 'NONE',  ( -111.8629285205952897, -282.4375830952704405, -279.2713490570718591 ) ) ;
#61403 = CARTESIAN_POINT ( 'NONE',  ( -48.18343439339132317, -266.0193969580586781, -497.3422536412688828 ) ) ;
#61404 = CARTESIAN_POINT ( 'NONE',  ( -108.8009961343364012, -276.9536952206743763, -250.2035018576559935 ) ) ;
#61405 = CARTESIAN_POINT ( 'NONE',  ( 18.28262132308068288, -280.2540963088529224, -320.7454723108579628 ) ) ;
#61406 = CARTESIAN_POINT ( 'NONE',  ( -75.01093283198058259, -276.0244077164914529, -336.7217739507690339 ) ) ;
#61407 = CIRCLE ( 'NONE', #29499, 4.000000000000003553 ) ;
#61408 = CARTESIAN_POINT ( 'NONE',  ( -73.62709049711578757, -297.0632615374768193, -334.5021984130257238 ) ) ;
#61409 = CARTESIAN_POINT ( 'NONE',  ( -67.77139653902742111, -282.3625946972241536, -340.7566156138795463 ) ) ;
#61410 = CARTESIAN_POINT ( 'NONE',  ( -98.65109707473668266, -298.0478409866923357, -230.2122883406818232 ) ) ;
#61411 = CARTESIAN_POINT ( 'NONE',  ( -77.95495267552034591, -298.8336284172539195, -205.5239219474385663 ) ) ;
#61412 = CARTESIAN_POINT ( 'NONE',  ( 20.70092020750152884, -274.5957205646369061, -226.0331798433515758 ) ) ;
#61413 = CARTESIAN_POINT ( 'NONE',  ( 5.629242589961247489, -294.6339370983061485, -208.8279753140617743 ) ) ;
#61414 = CARTESIAN_POINT ( 'NONE',  ( 38.10871369454270052, -287.9110536380823646, -285.7310580775337030 ) ) ;
#61415 = CARTESIAN_POINT ( 'NONE',  ( 2.826228734243690255, -274.6592971622505388, -334.6633726329814067 ) ) ;
#61416 = CARTESIAN_POINT ( 'NONE',  ( -74.42918108061037685, -289.3646693668756598, -337.8559372751926730 ) ) ;
#61417 = ADVANCED_FACE ( 'NONE', ( #3622 ), #90238, .T. ) ;
#61418 = CARTESIAN_POINT ( 'NONE',  ( 25.15774563281336995, -286.0866525304282959, -232.1874657156944295 ) ) ;
#61419 = CARTESIAN_POINT ( 'NONE',  ( -109.3057593288156113, -288.8240063711422749, -249.2382670070191466 ) ) ;
#61420 = ORIENTED_EDGE ( 'NONE', *, *, #58419, .F. ) ;
#61421 = CARTESIAN_POINT ( 'NONE',  ( 88.37812178648184158, 82.46720509654242903, -304.8213980281626618 ) ) ;
#61422 = CARTESIAN_POINT ( 'NONE',  ( -73.58093152415898430, -289.0546347464799624, -333.8161171322937548 ) ) ;
#61423 = CYLINDRICAL_SURFACE ( 'NONE', #73166, 0.5000000000000004441 ) ;
#61424 = CARTESIAN_POINT ( 'NONE',  ( -85.94411423481727752, -284.6481988035160384, -329.7801852529115081 ) ) ;
#61425 = CARTESIAN_POINT ( 'NONE',  ( 29.27740950945138110, -292.1138533835527937, -232.2203990129869737 ) ) ;
#61426 = CARTESIAN_POINT ( 'NONE',  ( 37.46538932571372982, -282.9689897271921950, -255.8580222907608288 ) ) ;
#61427 = CARTESIAN_POINT ( 'NONE',  ( -19.88512593388098892, -281.5870419396055695, -195.8180022544659096 ) ) ;
#61428 = CARTESIAN_POINT ( 'NONE',  ( -61.53672519101359484, -283.2085972770206013, -339.2881580002921851 ) ) ;
#61429 = CARTESIAN_POINT ( 'NONE',  ( 24.11904343356764713, -278.1367644770287484, -313.4337773170307742 ) ) ;
#61430 = CARTESIAN_POINT ( 'NONE',  ( -107.7730309721822124, -296.9506773564249897, -239.1097205282081291 ) ) ;
#61431 = CARTESIAN_POINT ( 'NONE',  ( -51.67391808818965870, -275.1802827099421052, -198.2268631980161047 ) ) ;
#61432 = CARTESIAN_POINT ( 'NONE',  ( -6.569656479832156393, -290.4783527478678593, -202.3542937983152683 ) ) ;
#61433 = CARTESIAN_POINT ( 'NONE',  ( -99.60927132711695720, -271.8805023964864631, -231.5039425651470424 ) ) ;
#61434 = ORIENTED_EDGE ( 'NONE', *, *, #44228, .T. ) ;
#61435 = DIRECTION ( 'NONE',  ( -0.000000000000000000, -1.000000000000000000, -0.000000000000000000 ) ) ;
#61436 = CARTESIAN_POINT ( 'NONE',  ( -102.2588566181382106, -286.9623344743721987, -233.8263512287691697 ) ) ;
#61437 = CARTESIAN_POINT ( 'NONE',  ( 6.448821540586438417, -295.5524777293240959, -333.3852067386901581 ) ) ;
#61438 = CARTESIAN_POINT ( 'NONE',  ( -74.77942668136779503, -286.1908312449459686, -207.5733062774455107 ) ) ;
#61439 = ADVANCED_FACE ( 'NONE', ( #4091 ), #32962, .F. ) ;
#61440 = CARTESIAN_POINT ( 'NONE',  ( -22.99466727141519229, -275.9318096968128202, -345.8272230398811189 ) ) ;
#61441 = CARTESIAN_POINT ( 'NONE',  ( -13.90542449179094930, -292.9997356293948769, -197.0655184142523240 ) ) ;
#61442 = CARTESIAN_POINT ( 'NONE',  ( 37.08138574416904731, -285.5113130251838811, -256.1657042154923829 ) ) ;
#61443 = CARTESIAN_POINT ( 'NONE',  ( -25.02900512212269746, -292.5383591334406219, -194.3733437478906012 ) ) ;
#61444 = CARTESIAN_POINT ( 'NONE',  ( -72.36527503667066696, -289.8625635077495417, -334.4347996891973480 ) ) ;
#61445 = CYLINDRICAL_SURFACE ( 'NONE', #5155, 7.910944475430059519 ) ;
#61446 = CARTESIAN_POINT ( 'NONE',  ( -82.33893616535382876, -218.9925579527750301, -348.9763288427828343 ) ) ;
#61447 = CARTESIAN_POINT ( 'NONE',  ( -68.23793463958713801, -287.1738228914134652, -200.5748802341978489 ) ) ;
#61448 = CARTESIAN_POINT ( 'NONE',  ( -99.86837403722181250, -276.6952119285918457, -220.4570493818173702 ) ) ;
#61449 = VERTEX_POINT ( 'NONE', #54727 ) ;
#61450 = CARTESIAN_POINT ( 'NONE',  ( 22.37323797389218072, -279.8809646230564567, -227.8363929208654781 ) ) ;
#61451 = CARTESIAN_POINT ( 'NONE',  ( -112.0643677754729595, -278.4509914101101913, -251.8065837479296363 ) ) ;
#61452 = CARTESIAN_POINT ( 'NONE',  ( -75.46107267245471917, -281.5430959746002486, -205.9047935234524971 ) ) ;
#61453 = CARTESIAN_POINT ( 'NONE',  ( -104.7603843068534104, -262.4557100720102767, -316.6309476432972474 ) ) ;
#61454 = CARTESIAN_POINT ( 'NONE',  ( 24.61877116015681466, -280.7246355570950413, -315.0991609931664925 ) ) ;
#61455 = CARTESIAN_POINT ( 'NONE',  ( -24.84211793245598443, -284.2323434094514596, -196.7178524456427908 ) ) ;
#61456 = CARTESIAN_POINT ( 'NONE',  ( -23.61084004444499485, -299.9819473029384085, -194.3703956122839998 ) ) ;
#61457 = CARTESIAN_POINT ( 'NONE',  ( -55.81281796273394491, -295.7886654723936317, -341.1016354192264544 ) ) ;
#61458 = EDGE_LOOP ( 'NONE', ( #417, #33131, #26753, #29531, #77486, #62844 ) ) ;
#61459 = CARTESIAN_POINT ( 'NONE',  ( -5.814994546087259408, -291.1603951620834323, -203.9596646753071809 ) ) ;
#61460 = CARTESIAN_POINT ( 'NONE',  ( 37.14208259394408174, -276.4431242236773301, -289.4786203918422984 ) ) ;
#61461 = CARTESIAN_POINT ( 'NONE',  ( 30.17481857447199545, -275.1785295998173524, -242.4701479630790857 ) ) ;
#61462 = CARTESIAN_POINT ( 'NONE',  ( 19.81472236261294739, -273.7755261625891308, -219.1495490646263988 ) ) ;
#61463 = CARTESIAN_POINT ( 'NONE',  ( 0.000000000000000000, 0.000000000000000000, -9.000000000000001776 ) ) ;
#61464 = CARTESIAN_POINT ( 'NONE',  ( -58.11829912362318140, -271.7836733630734329, -198.2428810843090048 ) ) ;
#61465 = EDGE_CURVE ( 'NONE', #13609, #135, #66904, .T. ) ;
#61466 = CARTESIAN_POINT ( 'NONE',  ( -44.72051730037452444, -296.5689367847056701, -346.4677762402475878 ) ) ;
#61467 = CARTESIAN_POINT ( 'NONE',  ( 153.1745786719506270, 129.2309077672098283, 12.62609896151546351 ) ) ;
#61468 = CARTESIAN_POINT ( 'NONE',  ( 175.2296996224750103, 275.5000000000000568, 24.50000000000000355 ) ) ;
#61469 = CARTESIAN_POINT ( 'NONE',  ( -96.16157294211976136, -285.0206594225489880, -314.1155307486350807 ) ) ;
#61470 = CARTESIAN_POINT ( 'NONE',  ( 38.51907482650000958, -283.3782910712143348, -275.5688201612044281 ) ) ;
#61471 = CARTESIAN_POINT ( 'NONE',  ( -105.6572487490586241, -284.2476244511596519, -244.3442295329869012 ) ) ;
#61472 = CARTESIAN_POINT ( 'NONE',  ( -81.31217839892325117, -276.0612432209869098, -329.6319999886777623 ) ) ;
#61473 = CARTESIAN_POINT ( 'NONE',  ( -23.81761041706950266, -284.7379508881656420, -343.3540250022544456 ) ) ;
#61474 = CARTESIAN_POINT ( 'NONE',  ( -96.66252507877891276, -276.4247662693406937, -314.1058112127864774 ) ) ;
#61475 = CARTESIAN_POINT ( 'NONE',  ( 21.72210377702268858, -276.0259536602487742, -226.9365495615540169 ) ) ;
#61476 = CARTESIAN_POINT ( 'NONE',  ( -113.5582899549025058, -279.4823359841267916, -260.1993774051363175 ) ) ;
#61477 = ORIENTED_EDGE ( 'NONE', *, *, #73959, .F. ) ;
#61478 = CARTESIAN_POINT ( 'NONE',  ( 196.8803347170859865, 20.19615242270663558, 12.49999999999999289 ) ) ;
#61479 = CARTESIAN_POINT ( 'NONE',  ( -96.62889079012583693, -287.0543867561888760, -223.1876666720501987 ) ) ;
#61480 = CARTESIAN_POINT ( 'NONE',  ( -50.51028373539165273, -294.4218007088908280, -342.3277083718405152 ) ) ;
#61481 = CARTESIAN_POINT ( 'NONE',  ( -95.38681836540783365, -289.2180863572851308, -320.7999624938732381 ) ) ;
#61483 = CARTESIAN_POINT ( 'NONE',  ( -97.57312137477052261, -289.3857976213455458, -227.2610938846886199 ) ) ;
#61482 = CARTESIAN_POINT ( 'NONE',  ( 18.23300165627940217, -285.4447545129391983, -222.1239182315387382 ) ) ;
#61484 = CARTESIAN_POINT ( 'NONE',  ( -67.93596766645501361, -284.6680758788762660, -337.0778422711407529 ) ) ;
#61485 = CARTESIAN_POINT ( 'NONE',  ( 20.17989833638084107, -274.2169863135529795, -318.4887229749992912 ) ) ;
#61486 = CARTESIAN_POINT ( 'NONE',  ( -62.91358121270257442, -284.1245327268627534, -198.5800667750541209 ) ) ;
#61487 = CARTESIAN_POINT ( 'NONE',  ( 36.32092951419483029, -289.3712653618989634, -256.2608468642360435 ) ) ;
#61488 = CARTESIAN_POINT ( 'NONE',  ( 18.93158292204115156, -284.8598328238511499, -220.4510693306722828 ) ) ;
#61489 = CARTESIAN_POINT ( 'NONE',  ( 24.33505303338034764, -283.0390337919583885, -309.9434359571995969 ) ) ;
#61490 = CARTESIAN_POINT ( 'NONE',  ( -73.52197408791941768, -291.5311599035569543, -336.2621993457808571 ) ) ;
#61491 = LINE ( 'NONE', #90778, #88197 ) ;
#61492 = CARTESIAN_POINT ( 'NONE',  ( 153.6987871352711181, 19.48326534539917887, -11.45812909362560639 ) ) ;
#61493 = CARTESIAN_POINT ( 'NONE',  ( -94.47631268537686822, -297.7915505840637138, -319.8075561569701222 ) ) ;
#61494 = CARTESIAN_POINT ( 'NONE',  ( 1.455780395478187828, -278.5700010461696934, -206.1156628961948059 ) ) ;
#61495 = CARTESIAN_POINT ( 'NONE',  ( 36.55169625369870801, -292.4841139265116681, -249.2436295050563331 ) ) ;
#61496 = CARTESIAN_POINT ( 'NONE',  ( -97.52343850647956458, -295.5420461995283858, -227.6457954173676512 ) ) ;
#61497 = CARTESIAN_POINT ( 'NONE',  ( 31.53832800146757265, -279.8957251927471361, -244.5872050574532466 ) ) ;
#61498 = CARTESIAN_POINT ( 'NONE',  ( 26.52360592865664657, -273.1149907170185429, -232.0180952566425390 ) ) ;
#61499 = CARTESIAN_POINT ( 'NONE',  ( 36.20156353142176897, -294.8723754790291878, -270.7459023020772975 ) ) ;
#61500 = FACE_OUTER_BOUND ( 'NONE', #91414, .T. ) ;
#61501 = CARTESIAN_POINT ( 'NONE',  ( -110.4678789762892990, -271.4092890200255965, -248.0180792343690541 ) ) ;
#61502 = CARTESIAN_POINT ( 'NONE',  ( -32.10501939145949279, -293.2268402529552986, -346.1802083345339724 ) ) ;
#61503 = CARTESIAN_POINT ( 'NONE',  ( 29.26417206702861407, -294.5567129385108842, -238.9514180124777170 ) ) ;
#61504 = DIRECTION ( 'NONE',  ( -1.000000000000000000, -0.000000000000000000, -0.000000000000000000 ) ) ;
#61505 = CARTESIAN_POINT ( 'NONE',  ( 33.93505744973376892, -294.5728157658050463, -286.9156028189549943 ) ) ;
#61506 = FACE_OUTER_BOUND ( 'NONE', #1557, .T. ) ;
#61508 = CARTESIAN_POINT ( 'NONE',  ( -3.143756393969438179, -294.5870452864601248, -334.8553087624939053 ) ) ;
#61507 = CARTESIAN_POINT ( 'NONE',  ( -8.688179225933367889, -280.6993297854849629, -340.1113648317503362 ) ) ;
#61509 = CARTESIAN_POINT ( 'NONE',  ( 28.30500385160923926, -282.0790964816146698, -310.7053016491167909 ) ) ;
#61510 = CARTESIAN_POINT ( 'NONE',  ( -76.75071982764404765, -283.2309225159081052, -336.5491155393883105 ) ) ;
#61511 = CARTESIAN_POINT ( 'NONE',  ( -112.2011284414167989, -288.5773692399648667, -268.3886428612408395 ) ) ;
#61512 = CYLINDRICAL_SURFACE ( 'NONE', #6422, 0.5000000000000004441 ) ;
#61513 = CARTESIAN_POINT ( 'NONE',  ( 37.00639391132412470, -279.8146009653883652, -253.1260813463499630 ) ) ;
#61514 = CARTESIAN_POINT ( 'NONE',  ( 14.38503507160792161, -287.2656527834864733, -327.0531835923711697 ) ) ;
#61515 = CARTESIAN_POINT ( 'NONE',  ( 175.2296996224750103, 247.0000000000001137, 0.000000000000000000 ) ) ;
#61516 = CARTESIAN_POINT ( 'NONE',  ( -10.17677864706474722, -296.2916617261439001, -338.9796829379534415 ) ) ;
#61517 = CARTESIAN_POINT ( 'NONE',  ( -70.03232798151306326, -278.8995801838204898, -339.4401173282693094 ) ) ;
#61518 = CARTESIAN_POINT ( 'NONE',  ( -57.11486062434031652, -279.4566356340969833, -200.0680912254142925 ) ) ;
#61519 = CARTESIAN_POINT ( 'NONE',  ( 11.11714006095851204, -292.8683760509114791, -210.4532291340083532 ) ) ;
#61520 = CARTESIAN_POINT ( 'NONE',  ( -104.5153971260959480, -282.1762925267153150, -305.0731624576172862 ) ) ;
#61521 = CARTESIAN_POINT ( 'NONE',  ( -69.42180986089981332, -279.4743752147767282, -338.1680043409789391 ) ) ;
#61522 = CARTESIAN_POINT ( 'NONE',  ( 24.61995384112986684, -293.1496043309717265, -309.4968696820446894 ) ) ;
#61523 = CARTESIAN_POINT ( 'NONE',  ( -83.95301859143829404, -295.4115979741238220, -211.6041129812376482 ) ) ;
#61524 = ORIENTED_EDGE ( 'NONE', *, *, #83427, .T. ) ;
#61525 = DIRECTION ( 'NONE',  ( 0.7957555401921980742, 0.6056179655966482667, 0.000000000000000000 ) ) ;
#61526 = CARTESIAN_POINT ( 'NONE',  ( -9.212978297705529229, -294.1818684772928236, -337.8044273669349309 ) ) ;
#61527 = CARTESIAN_POINT ( 'NONE',  ( 208.2002815004974252, 0.04196010845019423202, -7.500000000000014211 ) ) ;
#61528 = CARTESIAN_POINT ( 'NONE',  ( 27.33386217378598815, -291.4809262143062369, -301.5434626090942629 ) ) ;
#61529 = CARTESIAN_POINT ( 'NONE',  ( -114.1802237732302387, -271.7494487974028061, -270.3509185704776883 ) ) ;
#61530 = CARTESIAN_POINT ( 'NONE',  ( 23.61233811165435270, -279.0840084129175693, -225.3621101606552770 ) ) ;
#61531 = CARTESIAN_POINT ( 'NONE',  ( -78.27285679202557844, -286.8289287694049108, -205.7241418291234538 ) ) ;
#61532 = CARTESIAN_POINT ( 'NONE',  ( -42.66603306456350708, -288.9543693118744159, -343.2172950924804695 ) ) ;
#61533 = CARTESIAN_POINT ( 'NONE',  ( -89.56361126698323005, -279.3244425694189772, -322.4295198765239547 ) ) ;
#61534 = CARTESIAN_POINT ( 'NONE',  ( -110.6830428665489450, -274.2594826906876619, -262.1460184820764425 ) ) ;
#61535 = CARTESIAN_POINT ( 'NONE',  ( -48.68426251022908957, -275.9945798105036374, -342.9281435129106512 ) ) ;
#61536 = ORIENTED_EDGE ( 'NONE', *, *, #899, .T. ) ;
#61537 = CARTESIAN_POINT ( 'NONE',  ( -37.60332984904555076, -297.7156808445990919, -193.3827064533411146 ) ) ;
#61538 = CARTESIAN_POINT ( 'NONE',  ( -109.8353161666531292, -292.6917963651112018, -253.3942188511090876 ) ) ;
#61539 = CARTESIAN_POINT ( 'NONE',  ( 6.174032552145646946, -296.0728509225353378, -332.9779720756002916 ) ) ;
#61540 = CARTESIAN_POINT ( 'NONE',  ( 198.9506515269325178, 68.58287003106127599, -4.213754548338595640 ) ) ;
#61541 = CARTESIAN_POINT ( 'NONE',  ( -109.8896582381250937, -291.0852390379755548, -279.3436812136667982 ) ) ;
#61542 = CARTESIAN_POINT ( 'NONE',  ( 156.8041522122653930, 275.5000000000000568, 16.89672165344857646 ) ) ;
#61543 = CARTESIAN_POINT ( 'NONE',  ( 38.21112658040112109, -291.6197507629605639, -264.6975630184206238 ) ) ;
#61544 = CARTESIAN_POINT ( 'NONE',  ( -43.29235780551449864, -298.3123637854193362, -193.5594111415594227 ) ) ;
#61545 = CARTESIAN_POINT ( 'NONE',  ( -105.8241808029595745, -296.5584312415042518, -244.8728916037269698 ) ) ;
#61546 = CARTESIAN_POINT ( 'NONE',  ( 208.0393982316568326, 37.47427918878999265, 12.00000000000000000 ) ) ;
#61547 = CARTESIAN_POINT ( 'NONE',  ( 195.2258176893294035, 27.09966188323243586, 15.00706248549522925 ) ) ;
#61548 = CARTESIAN_POINT ( 'NONE',  ( -112.9815466882613606, -292.2041933408694376, -259.9077001395103821 ) ) ;
#61549 = CARTESIAN_POINT ( 'NONE',  ( -86.96033596737727578, -287.3602571626767030, -214.2738096480571528 ) ) ;
#61550 = CARTESIAN_POINT ( 'NONE',  ( -51.89363856869665170, -271.8654817022522252, -196.9031983860462844 ) ) ;
#61551 = CARTESIAN_POINT ( 'NONE',  ( -13.62944216140255982, -276.2825356963100489, -199.7987837056423643 ) ) ;
#61552 = CARTESIAN_POINT ( 'NONE',  ( 26.08744408407482496, -291.1041843294155456, -231.3009497301416388 ) ) ;
#61553 = CARTESIAN_POINT ( 'NONE',  ( -98.63629697510526739, -279.8117827392970298, -314.9171776963686966 ) ) ;
#61554 = SHAPE_REPRESENTATION ( 'Metal Foot Protection Guard', ( #18940 ), #91438 ) ;
#61555 = CARTESIAN_POINT ( 'NONE',  ( 24.21179613797572827, -281.4466253359879602, -309.8884051730248643 ) ) ;
#61556 = CARTESIAN_POINT ( 'NONE',  ( -88.99374129097709840, -278.8379479188694177, -327.0493809011744588 ) ) ;
#61557 = CARTESIAN_POINT ( 'NONE',  ( -28.25678522229615908, -278.9597868732846564, -194.2454716615108907 ) ) ;
#61558 = CARTESIAN_POINT ( 'NONE',  ( -84.40583500399526429, -218.0948329967893642, -349.5577229382324163 ) ) ;
#61559 = CARTESIAN_POINT ( 'NONE',  ( 9.357681950251764746, -275.6177469845693508, -209.4350322245835514 ) ) ;
#61560 = EDGE_CURVE ( 'NONE', #90042, #63082, #16487, .T. ) ;
#61561 = CARTESIAN_POINT ( 'NONE',  ( 6.817839845103098817, -276.1606719208120353, -208.0657226290591950 ) ) ;
#61562 = CARTESIAN_POINT ( 'NONE',  ( -95.95921662488163406, -298.4090924074130271, -317.1477375740089997 ) ) ;
#61563 = ORIENTED_EDGE ( 'NONE', *, *, #90310, .T. ) ;
#61564 = DIRECTION ( 'NONE',  ( -0.000000000000000000, -1.000000000000000000, -0.000000000000000000 ) ) ;
#61565 = CARTESIAN_POINT ( 'NONE',  ( -95.18601776173989037, -290.9997319683336627, -315.4176125127284536 ) ) ;
#61566 = CARTESIAN_POINT ( 'NONE',  ( 13.55133964658240053, -288.5130015190085260, -213.8647306276573374 ) ) ;
#61567 = CARTESIAN_POINT ( 'NONE',  ( -68.80936241708438672, -288.8257457813284645, -336.3435315383437114 ) ) ;
#61568 = CARTESIAN_POINT ( 'NONE',  ( -29.46300093431857903, -285.6570733878498345, -193.8271189874319020 ) ) ;
#61569 = DIRECTION ( 'NONE',  ( -1.000000000000000000, 0.000000000000000000, 0.000000000000000000 ) ) ;
#61570 = CARTESIAN_POINT ( 'NONE',  ( 34.85200946160615132, -279.7514410338675930, -254.9871473504247774 ) ) ;
#61571 = CARTESIAN_POINT ( 'NONE',  ( 28.74718094033504556, -288.9594990387930693, -236.4377144467182177 ) ) ;
#61572 = CARTESIAN_POINT ( 'NONE',  ( 1.449971091069490958, -281.0038303665621697, -333.0778106514468959 ) ) ;
#61573 = CARTESIAN_POINT ( 'NONE',  ( -109.5244966888453888, -279.6854236707175687, -284.2437333962120078 ) ) ;
#61574 = CARTESIAN_POINT ( 'NONE',  ( 0.6134218090894920650, -289.5006452849897300, -337.1462158489534318 ) ) ;
#61575 = CARTESIAN_POINT ( 'NONE',  ( -95.31802922739805695, -278.4195060548344713, -314.8215915070111350 ) ) ;
#61576 = CARTESIAN_POINT ( 'NONE',  ( -111.5412756187544261, -289.1070073158556397, -289.4512742759040975 ) ) ;
#61577 = CARTESIAN_POINT ( 'NONE',  ( -105.2940793232880026, -285.8203593148964501, -234.3774983283701090 ) ) ;
#61578 = CARTESIAN_POINT ( 'NONE',  ( -32.31670539856073532, -286.6062361674736962, -193.5737716788744081 ) ) ;
#61579 = CARTESIAN_POINT ( 'NONE',  ( -109.4214679451498853, -284.8723010540758196, -258.7273982196827546 ) ) ;
#61580 = ORIENTED_EDGE ( 'NONE', *, *, #91011, .F. ) ;
#61581 = CARTESIAN_POINT ( 'NONE',  ( 140.6539576904058606, 250.5000000000000568, 12.50000000000000000 ) ) ;
#61582 = CARTESIAN_POINT ( 'NONE',  ( -112.8789282410077561, -292.3298204791718717, -276.8714205272397635 ) ) ;
#61583 = CARTESIAN_POINT ( 'NONE',  ( 35.89271610987277228, -292.5186696272881477, -292.6768108312361392 ) ) ;
#61584 = CARTESIAN_POINT ( 'NONE',  ( 34.93740733541853416, -274.7700269064890790, -282.4629565876073229 ) ) ;
#61585 = CARTESIAN_POINT ( 'NONE',  ( -114.2074343173303248, -295.9461899181725926, -266.7318064453463649 ) ) ;
#61586 = CARTESIAN_POINT ( 'NONE',  ( -88.39711606821805390, -289.8010988518086037, -217.1488024720823375 ) ) ;
#61587 = CARTESIAN_POINT ( 'NONE',  ( -7.601414920228121375, -292.8967370202886400, -338.1501680024688312 ) ) ;
#61588 = CARTESIAN_POINT ( 'NONE',  ( -110.5172093716584953, -291.6743380765848315, -276.6792795940152132 ) ) ;
#61589 = DIRECTION ( 'NONE',  ( -0.000000000000000000, -0.000000000000000000, 1.000000000000000000 ) ) ;
#61590 = CARTESIAN_POINT ( 'NONE',  ( 35.31713995567030651, -291.3044901842745276, -251.0572673468768983 ) ) ;
#61591 = CARTESIAN_POINT ( 'NONE',  ( -91.39072905797685564, -297.8208941614880700, -322.4320005777087772 ) ) ;
#61592 = CARTESIAN_POINT ( 'NONE',  ( 35.78681571125072480, -288.4302701689059063, -265.5593704035121050 ) ) ;
#61593 = CARTESIAN_POINT ( 'NONE',  ( 29.10488408497458579, -278.0026853319333782, -306.0137065524402260 ) ) ;
#61594 = CARTESIAN_POINT ( 'NONE',  ( -110.2932645535070151, -277.0498069350354058, -293.9003250733066466 ) ) ;
#61595 = CARTESIAN_POINT ( 'NONE',  ( -95.44227462878096446, -296.4307105408476559, -219.9977073298028927 ) ) ;
#61596 = CARTESIAN_POINT ( 'NONE',  ( 21.63093920567703776, -274.4119381339535835, -315.0847339572242731 ) ) ;
#61597 = CARTESIAN_POINT ( 'NONE',  ( -32.85220798371379658, -278.1890079382548606, -196.0566183925323855 ) ) ;
#61598 = CARTESIAN_POINT ( 'NONE',  ( 19.29552080841105166, -276.0991754117393384, -223.6775479536968874 ) ) ;
#61599 = CARTESIAN_POINT ( 'NONE',  ( -17.58515827736567516, -275.2012800044492451, -343.9554076225475114 ) ) ;
#61600 = DIRECTION ( 'NONE',  ( 1.000000000000000000, 0.000000000000000000, 0.000000000000000000 ) ) ;
#61601 = CARTESIAN_POINT ( 'NONE',  ( -36.49128131194280655, -298.8659001945193836, -197.1995205611631263 ) ) ;
#61602 = CARTESIAN_POINT ( 'NONE',  ( 164.7123623445222904, 3.000000000000000000, -9.000000000000001776 ) ) ;
#61604 = CARTESIAN_POINT ( 'NONE',  ( -34.03855549380171652, -273.9281724191407648, -197.4358875060958667 ) ) ;
#61603 = CARTESIAN_POINT ( 'NONE',  ( 17.43157566775478173, -286.2944982594826229, -322.1133649038514477 ) ) ;
#61605 = CARTESIAN_POINT ( 'NONE',  ( -34.66682091908305097, -289.0194085136268427, -347.3146430559266946 ) ) ;
#61606 = CARTESIAN_POINT ( 'NONE',  ( 95.53882501024096996, -301.6877222252096544, -194.9613191052525565 ) ) ;
#61607 = CARTESIAN_POINT ( 'NONE',  ( -109.9476671421566323, -294.7858889351487619, -252.1868659936057497 ) ) ;
#61608 = EDGE_CURVE ( 'NONE', #79037, #90280, #44885, .T. ) ;
#61609 = CARTESIAN_POINT ( 'NONE',  ( 1.301628852008377857, -279.7513899201317713, -203.8862910276628782 ) ) ;
#61610 = EDGE_CURVE ( 'NONE', #9799, #78639, #1880, .T. ) ;
#61611 = CARTESIAN_POINT ( 'NONE',  ( 180.6899167944524436, 8.542400036368780647, 10.00000000000000000 ) ) ;
#61612 = CARTESIAN_POINT ( 'NONE',  ( -79.18647895631424660, -277.4878362949309007, -208.0580722848341964 ) ) ;
#61613 = FACE_OUTER_BOUND ( 'NONE', #44411, .T. ) ;
#61614 = CARTESIAN_POINT ( 'NONE',  ( -106.9429893934029110, -289.6548281415971360, -247.0632417422967819 ) ) ;
#61615 = DIRECTION ( 'NONE',  ( -0.9849620900324524975, 0.000000000000000000, 0.1727706028203382094 ) ) ;
#61616 = DIRECTION ( 'NONE',  ( -0.9893575751536621832, 0.000000000000000000, 0.1455045995357737432 ) ) ;
#61617 = CARTESIAN_POINT ( 'NONE',  ( -112.3678546950538362, -288.5773692419674035, -268.3843062701905069 ) ) ;
#61618 = CARTESIAN_POINT ( 'NONE',  ( -62.28238122372991370, -275.2418924425022055, -201.0165422859898854 ) ) ;
#61619 = CARTESIAN_POINT ( 'NONE',  ( -21.82775345596143168, -284.2823426414564096, -345.1803919028450878 ) ) ;
#61621 = CARTESIAN_POINT ( 'NONE',  ( -110.3093251802722961, -284.5808290741047131, -268.1872517854639568 ) ) ;
#61620 = CARTESIAN_POINT ( 'NONE',  ( 6.811864119086142644, -296.6223629286291157, -195.0207196009186532 ) ) ;
#61622 = CARTESIAN_POINT ( 'NONE',  ( -81.43848552385682638, -274.8646183644429470, -211.3832579355976691 ) ) ;
#61623 = CARTESIAN_POINT ( 'NONE',  ( -38.09425688055099357, -274.8453181833588133, -197.2035115027000529 ) ) ;
#61624 = CARTESIAN_POINT ( 'NONE',  ( -63.19798050311779747, -285.3891191477447933, -340.7632018540765557 ) ) ;
#61625 = CARTESIAN_POINT ( 'NONE',  ( -47.29289401283886463, -296.9814875110316166, -197.7536808889494182 ) ) ;
#61626 = ORIENTED_EDGE ( 'NONE', *, *, #56487, .T. ) ;
#61627 = CARTESIAN_POINT ( 'NONE',  ( 203.4918146885830481, 295.8998777880566422, -54.00000000006195933 ) ) ;
#61628 = CARTESIAN_POINT ( 'NONE',  ( 37.76177754168008960, -293.1723935388689029, -253.3176585523507356 ) ) ;
#61629 = CARTESIAN_POINT ( 'NONE',  ( -88.84725495041318766, -287.3042677641889213, -216.3331194698016589 ) ) ;
#61630 = DIRECTION ( 'NONE',  ( -2.312964634635742267E-15, 0.000000000000000000, 1.000000000000000000 ) ) ;
#61631 = CARTESIAN_POINT ( 'NONE',  ( -37.30987171927208834, -271.5523547857346784, -190.3611179825600175 ) ) ;
#61632 = CARTESIAN_POINT ( 'NONE',  ( -98.68070804685318365, -277.1314987317454097, -316.6610580569629292 ) ) ;
#61633 = CARTESIAN_POINT ( 'NONE',  ( -110.4587335633697620, -289.2239738649168430, -248.9055863497066525 ) ) ;
#61634 = CARTESIAN_POINT ( 'NONE',  ( 8.237837126473619875, -283.9360829183072497, -328.3332409107633225 ) ) ;
#61635 = CARTESIAN_POINT ( 'NONE',  ( -101.4494962044501705, -279.8108276321997892, -307.4527048382374232 ) ) ;
#61636 = CARTESIAN_POINT ( 'NONE',  ( 1.208609612536031275, -287.9816049563006572, -204.3725716139126973 ) ) ;
#61637 = CARTESIAN_POINT ( 'NONE',  ( 32.93568061977403971, -283.2105256904349062, -244.0189320777680564 ) ) ;
#61638 = CARTESIAN_POINT ( 'NONE',  ( 11.78406013720823964, -274.8791515353786963, -210.9988357890421753 ) ) ;
#61639 = CARTESIAN_POINT ( 'NONE',  ( -93.33545199929558578, -277.6630877529099166, -323.2930920257721823 ) ) ;
#61640 = CARTESIAN_POINT ( 'NONE',  ( -64.06351671530785552, -297.3234540689977621, -339.8942007019927587 ) ) ;
#61641 = FACE_OUTER_BOUND ( 'NONE', #23810, .T. ) ;
#61642 = FACE_OUTER_BOUND ( 'NONE', #4941, .T. ) ;
#61643 = CARTESIAN_POINT ( 'NONE',  ( -4.062703894991550158, -296.6041284862747602, -194.6067220786430880 ) ) ;
#61644 = CARTESIAN_POINT ( 'NONE',  ( -74.04961317085174244, -277.0618020572221667, -333.5316614481918123 ) ) ;
#61645 = CARTESIAN_POINT ( 'NONE',  ( -38.36756563531905329, -275.2446298607903259, -193.7650585525773010 ) ) ;
#61646 = CARTESIAN_POINT ( 'NONE',  ( 0.6701143928098732827, -288.3261633126162451, -206.7948747367249496 ) ) ;
#61647 = CARTESIAN_POINT ( 'NONE',  ( -110.9183084765487735, -297.8165728502071374, -290.5895746169477434 ) ) ;
#61648 = CARTESIAN_POINT ( 'NONE',  ( -96.19644211928942923, -297.0940644155557493, -319.4134174006304647 ) ) ;
#61649 = CARTESIAN_POINT ( 'NONE',  ( -98.26847706228650736, -293.1454919964240275, -226.8228107717127955 ) ) ;
#61650 = CARTESIAN_POINT ( 'NONE',  ( -90.76498441072926937, -277.2926712025489451, -217.8855981709258174 ) ) ;
#61651 = CARTESIAN_POINT ( 'NONE',  ( 36.45713297567899502, -283.3412445047342771, -260.2296440644144013 ) ) ;
#61652 = CARTESIAN_POINT ( 'NONE',  ( -111.5174836037884774, -270.6800391692093513, -262.0064817008655496 ) ) ;
#61653 = CARTESIAN_POINT ( 'NONE',  ( -33.10376765255829667, -284.8597511755815503, -346.0202278069147042 ) ) ;
#61654 = CARTESIAN_POINT ( 'NONE',  ( 35.42940636871686166, -286.5889295323000852, -279.2263383793293201 ) ) ;
#61655 = CARTESIAN_POINT ( 'NONE',  ( -20.56528858298729290, -109.1840546197655470, -362.3597369185399657 ) ) ;
#61656 = ORIENTED_EDGE ( 'NONE', *, *, #74648, .T. ) ;
#61657 = CARTESIAN_POINT ( 'NONE',  ( -25.13410883894809444, -285.8786893664658351, -198.3163175086395995 ) ) ;
#61658 = ORIENTED_EDGE ( 'NONE', *, *, #39601, .F. ) ;
#61659 = CARTESIAN_POINT ( 'NONE',  ( -112.2202933879071054, -285.4237050203911394, -286.9348557239857769 ) ) ;
#61660 = CARTESIAN_POINT ( 'NONE',  ( 8.971375338740864791, -299.1396686334033461, -197.2955806747803535 ) ) ;
#61661 = CARTESIAN_POINT ( 'NONE',  ( 11.83448627258825425, -285.5123635919666185, -211.5576456572826771 ) ) ;
#61662 = CARTESIAN_POINT ( 'NONE',  ( -8.959283811377348528, -281.3557079400586076, -199.0360967272378048 ) ) ;
#61663 =( LENGTH_UNIT ( ) NAMED_UNIT ( * ) SI_UNIT ( .MILLI., .METRE. ) );
#61664 = CARTESIAN_POINT ( 'NONE',  ( -28.32630538649357277, -281.6845454442236587, -194.5357499768319940 ) ) ;
#61665 = CARTESIAN_POINT ( 'NONE',  ( 15.14381404256942787, -281.1018422207299636, -213.9764870977493558 ) ) ;
#61666 = CARTESIAN_POINT ( 'NONE',  ( -67.68488546085839630, -283.1237833571631768, -207.2794874003663779 ) ) ;
#61667 = CARTESIAN_POINT ( 'NONE',  ( 45.84035832368225272, 12.14739099000767730, -332.1170644278120676 ) ) ;
#61668 = ORIENTED_EDGE ( 'NONE', *, *, #26752, .T. ) ;
#61669 = CARTESIAN_POINT ( 'NONE',  ( 18.82777259319304264, -278.2412231372006772, -319.8275887456744613 ) ) ;
#61670 = CARTESIAN_POINT ( 'NONE',  ( 153.2297941377568407, 207.2841453618251819, -217.1594761235724320 ) ) ;
#61671 = CARTESIAN_POINT ( 'NONE',  ( 37.34829943842961342, -279.5851454590617209, -271.3603852724700687 ) ) ;
#61672 = CARTESIAN_POINT ( 'NONE',  ( -7.607660556225663839, -294.1967127028186724, -200.4194464810985323 ) ) ;
#61673 = CARTESIAN_POINT ( 'NONE',  ( -38.35201194435276051, -294.4137330658026599, -343.4560695084881559 ) ) ;
#61674 = CARTESIAN_POINT ( 'NONE',  ( -112.2559168738368669, -290.2792572273092446, -252.8286614250167474 ) ) ;
#61675 = PLANE ( 'NONE',  #76248 ) ;
#61677 = CARTESIAN_POINT ( 'NONE',  ( 34.49367532732674135, -285.7305907533730078, -253.3913801277508071 ) ) ;
#61676 = CARTESIAN_POINT ( 'NONE',  ( -94.22516100884091372, -294.4291879782468868, -321.3990278339487077 ) ) ;
#61678 = CARTESIAN_POINT ( 'NONE',  ( 23.58843184267866633, -294.8310414569473323, -227.9313664620355837 ) ) ;
#61679 = CARTESIAN_POINT ( 'NONE',  ( -108.5103788932554636, -286.1077729990337843, -252.0236524524885340 ) ) ;
#61680 = ORIENTED_EDGE ( 'NONE', *, *, #87037, .F. ) ;
#61681 = CARTESIAN_POINT ( 'NONE',  ( 37.84257486308012375, -294.6878001315683377, -285.8577307696962748 ) ) ;
#61682 = CARTESIAN_POINT ( 'NONE',  ( -84.89709012618668282, -284.2216005811472428, -325.8270834352526890 ) ) ;
#61683 = CARTESIAN_POINT ( 'NONE',  ( -65.47204102606404774, -294.2067780506824874, -341.6261811681040399 ) ) ;
#61684 = CARTESIAN_POINT ( 'NONE',  ( -112.1623766457083349, -291.5742273284855060, -252.8675423958449642 ) ) ;
#61685 = CARTESIAN_POINT ( 'NONE',  ( -95.61841011882198416, -291.7235285240469125, -220.1080016883039150 ) ) ;
#61686 = CARTESIAN_POINT ( 'NONE',  ( -23.78309366172603490, -289.0408803685299972, -342.1426170189960771 ) ) ;
#61687 = ORIENTED_EDGE ( 'NONE', *, *, #53825, .T. ) ;
#61688 = DIRECTION ( 'NONE',  ( 0.000000000000000000, 0.000000000000000000, 1.000000000000000000 ) ) ;
#61689 = CARTESIAN_POINT ( 'NONE',  ( -37.27878502387808624, -299.9133432668988348, -194.5955393664444841 ) ) ;
#61690 = CARTESIAN_POINT ( 'NONE',  ( -107.7066562029457089, -271.7363077118395154, -239.9486306444150898 ) ) ;
#61691 = CARTESIAN_POINT ( 'NONE',  ( 19.02485570723045427, -279.9497379580461711, -223.5846208274220146 ) ) ;
#61692 = ORIENTED_EDGE ( 'NONE', *, *, #53477, .F. ) ;
#61693 = CARTESIAN_POINT ( 'NONE',  ( 21.80757117620698438, -274.3975131968944652, -221.1585712227553415 ) ) ;
#61694 = CARTESIAN_POINT ( 'NONE',  ( -90.53302526049461108, -295.7618794506587392, -219.2842815334317379 ) ) ;
#61695 = CARTESIAN_POINT ( 'NONE',  ( 16.50995796980268793, -278.1368192719580748, -321.4577362698927914 ) ) ;
#61696 = CARTESIAN_POINT ( 'NONE',  ( -5.986066114848981101, -272.6083415682933833, -203.0730083407317750 ) ) ;
#61697 = CARTESIAN_POINT ( 'NONE',  ( -107.2427461482248390, -297.4600600140454958, -292.9079945410235837 ) ) ;
#61698 = CARTESIAN_POINT ( 'NONE',  ( -109.1849137494126580, -297.4393913849345381, -285.0105136649997917 ) ) ;
#61699 = DIRECTION ( 'NONE',  ( -0.000000000000000000, -0.000000000000000000, -1.000000000000000000 ) ) ;
#61700 = CARTESIAN_POINT ( 'NONE',  ( -100.1034411153165991, -298.7290044283499810, -227.1247058303513882 ) ) ;
#61701 = CARTESIAN_POINT ( 'NONE',  ( -32.04458707427265551, -296.1181581694353326, -195.1962435526542379 ) ) ;
#61702 = CARTESIAN_POINT ( 'NONE',  ( 31.89490615158765152, -293.8904685894862041, -246.7475723268689194 ) ) ;
#61703 = CARTESIAN_POINT ( 'NONE',  ( 19.81483159065459176, -291.4761587397313178, -223.9892042655206126 ) ) ;
#61704 = CARTESIAN_POINT ( 'NONE',  ( 209.3190042249899250, 30.23012903947020646, 14.26380412667039188 ) ) ;
#61705 = CARTESIAN_POINT ( 'NONE',  ( 2.380857498295728458, -275.0618641025213833, -204.4699553064321549 ) ) ;
#61706 = CARTESIAN_POINT ( 'NONE',  ( -78.85681564543277489, -273.6421770151165447, -210.2539385205406575 ) ) ;
#61707 = CARTESIAN_POINT ( 'NONE',  ( 35.60603866203060619, -283.7736923825752342, -289.2564669135535951 ) ) ;
#61708 = CARTESIAN_POINT ( 'NONE',  ( 1.827186276290179823, -281.2244271097814590, -336.0809522062260726 ) ) ;
#61709 = CARTESIAN_POINT ( 'NONE',  ( -104.8900091063205480, -277.4245540456624326, -307.1107947223466113 ) ) ;
#61710 = CYLINDRICAL_SURFACE ( 'NONE', #70238, 7.999999999999992895 ) ;
#61711 = CARTESIAN_POINT ( 'NONE',  ( -110.3887706229250085, -283.8140340680066629, -265.4441880852010058 ) ) ;
#61712 = CARTESIAN_POINT ( 'NONE',  ( 22.77319316338241606, -280.1672660011499829, -315.4857014618617086 ) ) ;
#61713 = CARTESIAN_POINT ( 'NONE',  ( -11.06042472033237800, -275.2774481595370730, -339.0973491870378211 ) ) ;
#61714 = CARTESIAN_POINT ( 'NONE',  ( -103.2298473196971713, -281.0295542470021246, -234.4242296509845858 ) ) ;
#61715 = DIRECTION ( 'NONE',  ( -0.000000000000000000, -1.000000000000000000, -0.000000000000000000 ) ) ;
#61716 = CARTESIAN_POINT ( 'NONE',  ( 185.2169494693457921, 250.0000000000000568, 22.91843887563416615 ) ) ;
#61717 = CARTESIAN_POINT ( 'NONE',  ( -36.92344601342082910, -272.4572174972324206, -194.1493462586157079 ) ) ;
#61718 = B_SPLINE_CURVE_WITH_KNOTS ( 'NONE', 3,
 ( #19208, #70361, #32489, #47606, #5486, #20145, #62303, #25828, #91143, #68942, #48067, #27251, #49028, #19669 ),
 .UNSPECIFIED., .F., .F.,
 ( 4, 2, 2, 2, 2, 2, 4 ),
 ( 0.000000000000000000, 0.001076125775146711833, 0.001614188662720042597, 0.002152251550293373793, 0.003228377325440022309, 0.003766440213013335508, 0.004304503100586647840 ),
 .UNSPECIFIED. ) ;
#61719 = CARTESIAN_POINT ( 'NONE',  ( -73.19930813355162513, -279.5265209579058023, -336.4383094284160620 ) ) ;
#61720 = EDGE_CURVE ( 'NONE', #51424, #24735, #26062, .T. ) ;
#61721 = DIRECTION ( 'NONE',  ( 0.000000000000000000, 1.000000000000000000, 0.000000000000000000 ) ) ;
#61722 = CARTESIAN_POINT ( 'NONE',  ( -73.56376682094546027, -285.4486933774028898, -336.7314492666141632 ) ) ;
#61723 = CARTESIAN_POINT ( 'NONE',  ( 159.3464669004252130, 15.95758591462619336, -10.08665682397418983 ) ) ;
#61724 = CARTESIAN_POINT ( 'NONE',  ( -4.661502229877561909, -286.6216043090495305, -337.8806908614707822 ) ) ;
#61725 = CYLINDRICAL_SURFACE ( 'NONE', #55834, 0.5000000000000004441 ) ;
#61726 = CARTESIAN_POINT ( 'NONE',  ( -110.6077436098145768, -295.4045861318891752, -265.9773551691940270 ) ) ;
#61727 = CARTESIAN_POINT ( 'NONE',  ( -5.280047729139999646, -286.7652392031147883, -337.3156990769847425 ) ) ;
#61728 = CARTESIAN_POINT ( 'NONE',  ( -113.2098679957031493, -271.2709011634024137, -296.4525692007673570 ) ) ;
#61729 = CARTESIAN_POINT ( 'NONE',  ( -112.2072278674401531, -294.6096294047426909, -265.8718638674570798 ) ) ;
#61730 = CARTESIAN_POINT ( 'NONE',  ( -70.74509997123259097, -284.0994285422036114, -201.7541166295424375 ) ) ;
#61731 = CARTESIAN_POINT ( 'NONE',  ( 32.99997958420892274, -283.4470534781863762, -292.8545588516321345 ) ) ;
#61732 = CARTESIAN_POINT ( 'NONE',  ( -96.39918681714449633, -282.1420044092341186, -318.1956631655522187 ) ) ;
#61733 = CARTESIAN_POINT ( 'NONE',  ( 5.844624518468904739, -288.4484808899330801, -329.2793726299055947 ) ) ;
#61734 = CARTESIAN_POINT ( 'NONE',  ( -72.42648506604072622, -281.0033995892246139, -205.6739261749698642 ) ) ;
#61735 = CARTESIAN_POINT ( 'NONE',  ( 29.11508965688805617, -281.9416790250525651, -239.6440461672289644 ) ) ;
#61736 = CARTESIAN_POINT ( 'NONE',  ( 30.22406979101944557, -289.9715057260395952, -303.8446337056924449 ) ) ;
#61737 = VERTEX_POINT ( 'NONE', #59122 ) ;
#61738 = CARTESIAN_POINT ( 'NONE',  ( -96.93607219985013046, -273.2069953152112021, -221.5808175174131236 ) ) ;
#61739 = CARTESIAN_POINT ( 'NONE',  ( -108.5128722171562714, -292.2382798057213336, -293.0376917566769635 ) ) ;
#61740 = CARTESIAN_POINT ( 'NONE',  ( 159.4851178187871312, 3.000000000000000000, -9.000000000000001776 ) ) ;
#61741 = CARTESIAN_POINT ( 'NONE',  ( -115.3288506153726871, -298.8376638359844719, -288.1938231032136741 ) ) ;
#61742 = ORIENTED_EDGE ( 'NONE', *, *, #33379, .T. ) ;
#61743 = CARTESIAN_POINT ( 'NONE',  ( 35.85559431217997428, -273.3323524544736642, -253.2116385803447258 ) ) ;
#61744 = CARTESIAN_POINT ( 'NONE',  ( 197.0969223827550536, 71.90335919811118970, 12.15580473211910473 ) ) ;
#61745 = CARTESIAN_POINT ( 'NONE',  ( -55.89541940631961836, -293.6870707472124309, -344.2678153406051251 ) ) ;
#61746 = CARTESIAN_POINT ( 'NONE',  ( -38.07507084467897585, -273.3913078115546114, -197.2628633115357673 ) ) ;
#61747 = CARTESIAN_POINT ( 'NONE',  ( 28.85900960654986847, -289.5066803082945057, -302.7366300421691676 ) ) ;
#61748 = CARTESIAN_POINT ( 'NONE',  ( -65.68328017059339174, -285.1880983808048882, -338.7468920703397544 ) ) ;
#61749 = CARTESIAN_POINT ( 'NONE',  ( -39.21557508759703126, -293.4543665593869832, -193.9603899851933875 ) ) ;
#61750 = CARTESIAN_POINT ( 'NONE',  ( -109.9681002367401135, -292.1739520399975163, -246.1389439068909439 ) ) ;
#61751 = CARTESIAN_POINT ( 'NONE',  ( -52.36769633436161797, -291.6877866536235047, -198.8723961294197125 ) ) ;
#61752 = CARTESIAN_POINT ( 'NONE',  ( -104.0280200930546641, -287.0064152868697533, -236.0400548394829627 ) ) ;
#61753 = CARTESIAN_POINT ( 'NONE',  ( -2.392038180182951113, -280.6683031818170662, -201.7350128943758705 ) ) ;
#61754 = CARTESIAN_POINT ( 'NONE',  ( -111.1878491669540381, -294.8366627391303609, -254.2989303348274177 ) ) ;
#61755 = CARTESIAN_POINT ( 'NONE',  ( -13.42395082226543224, -282.5832479676305979, -343.5522463564098530 ) ) ;
#61756 = CARTESIAN_POINT ( 'NONE',  ( 12.35616036713719268, -276.6128957670105706, -215.1467677941314491 ) ) ;
#61757 = CARTESIAN_POINT ( 'NONE',  ( -21.39648532958013050, -288.7662352645559167, -200.3538533559491555 ) ) ;
#61758 = CARTESIAN_POINT ( 'NONE',  ( -88.39750893331228099, -275.8983340109349456, -326.3397734286518244 ) ) ;
#61759 = CARTESIAN_POINT ( 'NONE',  ( 208.4306832106270804, -199.2391364535880882, 0.000000000000000000 ) ) ;
#61760 = CARTESIAN_POINT ( 'NONE',  ( -61.56103168232197476, -282.8829826070968920, -339.3448907544527628 ) ) ;
#61761 = CARTESIAN_POINT ( 'NONE',  ( -105.8275000105147257, -280.2022760054974810, -235.9252415360201098 ) ) ;
#61762 = CARTESIAN_POINT ( 'NONE',  ( 23.09477475923405265, -287.2457204057055264, -317.7135876576458031 ) ) ;
#61763 = CARTESIAN_POINT ( 'NONE',  ( -14.55543027648865007, -294.1117480074439641, -199.9426550750086733 ) ) ;
#61764 = CARTESIAN_POINT ( 'NONE',  ( 11.25960873806925200, -276.3123692145800305, -211.6039555493101432 ) ) ;
#61765 = CARTESIAN_POINT ( 'NONE',  ( 25.72848013901437980, -276.2918157665897638, -227.0314313166890656 ) ) ;
#61766 = CARTESIAN_POINT ( 'NONE',  ( -110.1584954130612601, -278.4536533850556452, -265.1925273706037842 ) ) ;
#61767 = CARTESIAN_POINT ( 'NONE',  ( -47.54736812926478251, -299.9224262400600765, -196.1744654553654925 ) ) ;
#61768 = CARTESIAN_POINT ( 'NONE',  ( -88.94065543887441549, -283.3248562392004146, -216.1617062192939613 ) ) ;
#61769 = CARTESIAN_POINT ( 'NONE',  ( -4.609280072800064687, -292.1384201422026194, -200.6880746373742852 ) ) ;
#61770 = CARTESIAN_POINT ( 'NONE',  ( 26.78272143995865662, -289.6990484588970389, -311.6227404202854814 ) ) ;
#61771 = CARTESIAN_POINT ( 'NONE',  ( -25.34502083228317204, -291.1288499121718019, -197.9885670057450398 ) ) ;
#61772 = EDGE_LOOP ( 'NONE', ( #33697, #90633, #74592, #35441 ) ) ;
#61773 = CARTESIAN_POINT ( 'NONE',  ( -44.82116619460498441, -290.5341019360635073, -194.2647721673558578 ) ) ;
#61774 = CARTESIAN_POINT ( 'NONE',  ( 20.20217807723913950, -292.5851971834346159, -225.3876807377890543 ) ) ;
#61775 = VERTEX_POINT ( 'NONE', #37326 ) ;
#61776 = CARTESIAN_POINT ( 'NONE',  ( -82.65887779399071178, -290.7351921953559781, -332.2307059666654254 ) ) ;
#61777 = CARTESIAN_POINT ( 'NONE',  ( -110.3010914625495928, -278.8458396717747405, -273.3635674477395696 ) ) ;
#61778 = CARTESIAN_POINT ( 'NONE',  ( -111.2975919183238460, -295.2171995835493021, -290.6593587899989757 ) ) ;
#61779 = CARTESIAN_POINT ( 'NONE',  ( -78.47495036605826613, -286.1652749493692909, -205.3890585162750426 ) ) ;
#61780 = CARTESIAN_POINT ( 'NONE',  ( -30.88985682315427894, -286.4648368923487851, -193.6398219820470388 ) ) ;
#61782 = CARTESIAN_POINT ( 'NONE',  ( -108.9994259045149931, -284.7002132494902185, -284.4059684052884336 ) ) ;
#61781 = CIRCLE ( 'NONE', #45121, 0.5000000000000017764 ) ;
#61783 = CARTESIAN_POINT ( 'NONE',  ( -113.9563424175841249, -273.7439901500910651, -270.3762929349610431 ) ) ;
#61784 = CARTESIAN_POINT ( 'NONE',  ( 137.3882156427991390, 180.6064192809313909, -240.3616213788371283 ) ) ;
#61785 = CARTESIAN_POINT ( 'NONE',  ( 178.9112196240999992, 251.4731691113353236, -164.2126119813759715 ) ) ;
#61786 = CARTESIAN_POINT ( 'NONE',  ( 3.027542779753411573, -273.8063717156109647, -209.2847822823411263 ) ) ;
#61787 = CARTESIAN_POINT ( 'NONE',  ( 35.95223312036172558, -274.4528782497610564, -268.8693332707915147 ) ) ;
#61788 = CARTESIAN_POINT ( 'NONE',  ( -85.17325803495880621, -296.9191686114214690, -210.0977877455485157 ) ) ;
#61789 = CARTESIAN_POINT ( 'NONE',  ( -92.77482839370959766, -239.7623855883933857, -339.1558859853604986 ) ) ;
#61790 = CARTESIAN_POINT ( 'NONE',  ( 27.22359873830451704, -274.7795192335319712, -311.5036896027992839 ) ) ;
#61791 = CARTESIAN_POINT ( 'NONE',  ( -67.49052412720305938, -275.4113190183768438, -202.7526883425835251 ) ) ;
#61792 = ORIENTED_EDGE ( 'NONE', *, *, #24971, .F. ) ;
#61793 = CARTESIAN_POINT ( 'NONE',  ( -105.3412525188624045, -274.0924095737876769, -234.7843024903218065 ) ) ;
#61794 = CARTESIAN_POINT ( 'NONE',  ( -58.70113780472167520, -289.8281797772984874, -340.2835781494169396 ) ) ;
#61795 = CARTESIAN_POINT ( 'NONE',  ( -71.99204873566625906, -296.3014567289501429, -338.9432742808064631 ) ) ;
#61796 = CARTESIAN_POINT ( 'NONE',  ( -68.15857400180846071, -298.1506699728736862, -199.8072200716321731 ) ) ;
#61797 = CARTESIAN_POINT ( 'NONE',  ( -92.18927209325447336, -296.0311434916832241, -318.5352173933906670 ) ) ;
#61798 = ORIENTED_EDGE ( 'NONE', *, *, #93067, .T. ) ;
#61799 = EDGE_CURVE ( 'NONE', #86528, #58102, #22202, .T. ) ;
#61800 = CARTESIAN_POINT ( 'NONE',  ( -48.26125739924071212, -279.1100843173926478, -345.1808229464237456 ) ) ;
#61801 = ORIENTED_EDGE ( 'NONE', *, *, #4649, .F. ) ;
#61802 = CARTESIAN_POINT ( 'NONE',  ( 27.80259150927189182, -280.5222561422730791, -229.3253587791473080 ) ) ;
#61803 = CARTESIAN_POINT ( 'NONE',  ( -36.45132540264958010, -277.9820129269591575, -343.6035076930010064 ) ) ;
#61804 = CARTESIAN_POINT ( 'NONE',  ( -25.90013305583154946, -278.6684842869273666, -345.4814518129636554 ) ) ;
#61805 = CARTESIAN_POINT ( 'NONE',  ( -103.5428822824225534, -276.0962889277454337, -306.3584829065293889 ) ) ;
#61806 = CARTESIAN_POINT ( 'NONE',  ( -109.6445916786506274, -273.1874762735358217, -259.5137285536690683 ) ) ;
#61807 = CARTESIAN_POINT ( 'NONE',  ( 9.416850655049715968, -297.2234503871736706, -196.7834957107979790 ) ) ;
#61808 = FACE_OUTER_BOUND ( 'NONE', #21842, .T. ) ;
#61809 = CARTESIAN_POINT ( 'NONE',  ( -109.2857212142774301, -278.5546557279030822, -282.8066459144263263 ) ) ;
#61810 = CARTESIAN_POINT ( 'NONE',  ( 36.66311010202157661, -286.4814646207431679, -289.7669505293973771 ) ) ;
#61811 = CARTESIAN_POINT ( 'NONE',  ( 10.49007060466537666, -276.7123369542541695, -212.5258196686554015 ) ) ;
#61812 = CARTESIAN_POINT ( 'NONE',  ( 206.7809450508160865, 35.77530089738195329, 14.49999999999999822 ) ) ;
#61813 = CARTESIAN_POINT ( 'NONE',  ( -106.1879713544767299, -289.4203594134405080, -295.1157673435341735 ) ) ;
#61814 = CARTESIAN_POINT ( 'NONE',  ( -97.96918328365069328, -283.2678753185803089, -317.6646175712123750 ) ) ;
#61815 = EDGE_CURVE ( 'NONE', #93705, #54449, #23025, .T. ) ;
#61816 = CARTESIAN_POINT ( 'NONE',  ( 31.26557468018033248, -280.1587699166595371, -298.1282902344638615 ) ) ;
#61817 = B_SPLINE_CURVE_WITH_KNOTS ( 'NONE', 3,
 ( #90544, #54124, #17690, #54584, #20379, #5702, #47475, #82539 ),
 .UNSPECIFIED., .F., .F.,
 ( 4, 2, 2, 4 ),
 ( 2.841933599792538093E-17, 0.001370196721548293728, 0.002055295082322467371, 0.002740393443096640798 ),
 .UNSPECIFIED. ) ;
#61819 = CARTESIAN_POINT ( 'NONE',  ( -98.52584599908749396, -283.2116020439131034, -227.9379539621903916 ) ) ;
#61818 = CARTESIAN_POINT ( 'NONE',  ( 9.666770678202762923, -279.2881889945341527, -213.6768483925877433 ) ) ;
#61820 = CARTESIAN_POINT ( 'NONE',  ( -13.52940195129821177, -290.7433003103289479, -341.5342403475561923 ) ) ;
#61821 = CARTESIAN_POINT ( 'NONE',  ( -109.8821778902806727, -279.6105375055316244, -281.5418867918415913 ) ) ;
#61822 = CARTESIAN_POINT ( 'NONE',  ( 153.6947954963213760, 20.34868745056155959, -12.70025883435339864 ) ) ;
#61823 = CARTESIAN_POINT ( 'NONE',  ( -14.50043690629413362, -294.3482656844052485, -198.8693767043140213 ) ) ;
#61824 = CARTESIAN_POINT ( 'NONE',  ( -111.7209650602492985, -276.9898321192069943, -254.7517902831631886 ) ) ;
#61825 = CARTESIAN_POINT ( 'NONE',  ( -8.691091834693455809, -277.3185046426877420, -337.6281954159796328 ) ) ;
#61826 = CARTESIAN_POINT ( 'NONE',  ( -96.58339680265815730, -285.9190198425260405, -316.6261134549433223 ) ) ;
#61827 = DIRECTION ( 'NONE',  ( -1.000000000000000000, -0.000000000000000000, -0.000000000000000000 ) ) ;
#61828 = CARTESIAN_POINT ( 'NONE',  ( -111.7115557554895133, -292.3011281923740512, -283.7921675866518854 ) ) ;
#61829 = CARTESIAN_POINT ( 'NONE',  ( -78.64588175427462602, -293.6078344819043764, -333.0237903765516307 ) ) ;
#61830 = CARTESIAN_POINT ( 'NONE',  ( 37.86756833272411882, -286.5512697743581043, -254.5580960424597663 ) ) ;
#61831 = CARTESIAN_POINT ( 'NONE',  ( -106.4527194294426380, -289.2953449765810774, -244.3297865404355491 ) ) ;
#61832 = DIRECTION ( 'NONE',  ( -0.7071067811864494290, 8.659560562353731078E-17, 0.7071067811866457165 ) ) ;
#61833 = CARTESIAN_POINT ( 'NONE',  ( 28.46466553028474777, -274.6790778534708011, -303.1983470878130333 ) ) ;
#61834 = CARTESIAN_POINT ( 'NONE',  ( -15.24741628013194905, -292.9027502300475021, -341.2862498786924448 ) ) ;
#61835 = SURFACE_STYLE_FILL_AREA ( #47123 ) ;
#61836 = LINE ( 'NONE', #24915, #74610 ) ;
#61837 = CARTESIAN_POINT ( 'NONE',  ( -79.19778501283552430, -289.9787171685997009, -206.4953334003015186 ) ) ;
#61838 = CARTESIAN_POINT ( 'NONE',  ( -70.35842355555413974, -287.2096857055699388, -204.3444710870405459 ) ) ;
#61839 = CARTESIAN_POINT ( 'NONE',  ( -4.787788183634853034, -286.8691795759041838, -339.0355591239228943 ) ) ;
#61840 = EDGE_CURVE ( 'NONE', #64275, #26750, #89143, .T. ) ;
#61841 = CARTESIAN_POINT ( 'NONE',  ( -98.60760005059161415, -286.5387798743906842, -229.5951465862859777 ) ) ;
#61842 = DIRECTION ( 'NONE',  ( -0.000000000000000000, 1.000000000000000000, 0.000000000000000000 ) ) ;
#61843 = CARTESIAN_POINT ( 'NONE',  ( -81.58433094222112913, -286.2350274175871618, -212.0928474995660338 ) ) ;
#61844 = CARTESIAN_POINT ( 'NONE',  ( 20.04119715018747883, -294.8589025322291377, -221.4987077065173082 ) ) ;
#61845 = AXIS2_PLACEMENT_3D ( 'NONE', #42727, #36564, #51228 ) ;
#61846 = CARTESIAN_POINT ( 'NONE',  ( -112.9366163918105883, -276.6526533676092185, -268.7402689221095216 ) ) ;
#61847 = CARTESIAN_POINT ( 'NONE',  ( -6.579250699816183712, -276.9924331444652239, -340.9403477577145054 ) ) ;
#61848 = CARTESIAN_POINT ( 'NONE',  ( 19.31545630746252584, -290.9419942586628736, -220.3487549054204919 ) ) ;
#61849 = CARTESIAN_POINT ( 'NONE',  ( -91.05816846703244494, -279.3148217051064535, -215.1184886317592486 ) ) ;
#61850 = CARTESIAN_POINT ( 'NONE',  ( -110.4916491207447251, -298.3394665757891175, -285.2884422388504504 ) ) ;
#61851 = CARTESIAN_POINT ( 'NONE',  ( -48.18343439339133027, -273.4572633953990248, -501.0766502679427958 ) ) ;
#61852 = LINE ( 'NONE', #25843, #13333 ) ;
#61853 = CARTESIAN_POINT ( 'NONE',  ( -108.4027662223042370, -276.9713366982268781, -248.8857747593772558 ) ) ;
#61854 = CARTESIAN_POINT ( 'NONE',  ( 28.00644727378776366, -280.0435018214005254, -307.2720657957934236 ) ) ;
#61855 = CARTESIAN_POINT ( 'NONE',  ( 204.5044540939250055, -147.7221692137691775, 10.75739200365177695 ) ) ;
#61856 = CARTESIAN_POINT ( 'NONE',  ( 38.86316984842187594, -273.9707267780482880, -265.5033829570034527 ) ) ;
#61857 = CARTESIAN_POINT ( 'NONE',  ( -84.91102871554552678, -297.2420197399135304, -326.7119077935265068 ) ) ;
#61858 = CARTESIAN_POINT ( 'NONE',  ( 35.31180129020641800, -280.7848916590746171, -295.0813327202610594 ) ) ;
#61859 = CARTESIAN_POINT ( 'NONE',  ( 10.45411433616792252, -295.3141056561549931, -325.8495723414083045 ) ) ;
#61860 = CARTESIAN_POINT ( 'NONE',  ( -60.01800384170071823, -299.0795797461608458, -197.2369145107730901 ) ) ;
#61861 = CARTESIAN_POINT ( 'NONE',  ( -85.32086176758463125, -273.0344852712404986, -215.2474979412859284 ) ) ;
#61862 = CARTESIAN_POINT ( 'NONE',  ( -99.98365724561688239, -293.1101111241162016, -229.0237257701417661 ) ) ;
#61863 = CARTESIAN_POINT ( 'NONE',  ( 18.35003018030980826, -286.9910099010896261, -217.1106295021070025 ) ) ;
#61864 = CARTESIAN_POINT ( 'NONE',  ( 38.32231115665356924, -273.6304875881065186, -265.5423339125887878 ) ) ;
#61865 = CARTESIAN_POINT ( 'NONE',  ( -31.82889751765750219, -288.8178525183249690, -347.2160763128621284 ) ) ;
#61866 = CARTESIAN_POINT ( 'NONE',  ( 1.426009652876563782, -287.5788774304659228, -332.4938237524259534 ) ) ;
#61867 = CARTESIAN_POINT ( 'NONE',  ( -102.8503788927215084, -289.0380696716037505, -233.8424425862099554 ) ) ;
#61868 = ORIENTED_EDGE ( 'NONE', *, *, #39228, .F. ) ;
#61869 = CARTESIAN_POINT ( 'NONE',  ( 198.5843229385366726, 69.20886829666338258, 9.718619512930896320 ) ) ;
#61870 = CARTESIAN_POINT ( 'NONE',  ( 31.45524049038889203, -287.3870214156676752, -294.9572437573685875 ) ) ;
#61871 = CARTESIAN_POINT ( 'NONE',  ( 164.2231345125756263, 300.2961574867697436, -7.500000000000000000 ) ) ;
#61872 = CARTESIAN_POINT ( 'NONE',  ( -81.41662811903604791, -284.5764467986614363, -333.2765623931563823 ) ) ;
#61873 = CARTESIAN_POINT ( 'NONE',  ( 38.58205543801906146, -292.7530540957635594, -281.6926471693149097 ) ) ;
#61874 = CARTESIAN_POINT ( 'NONE',  ( -22.73965536964717415, -281.8360094825371789, -195.5195905845205573 ) ) ;
#61875 = CARTESIAN_POINT ( 'NONE',  ( -41.00166701588969431, -281.3221999881022839, -193.9287495705772812 ) ) ;
#61876 = CARTESIAN_POINT ( 'NONE',  ( -7.255417066997774889, -282.4795289046936659, -336.8866015445254334 ) ) ;
#61877 = CARTESIAN_POINT ( 'NONE',  ( -46.11751120001068216, -279.1634940181720594, -344.8979323227834470 ) ) ;
#61878 = CARTESIAN_POINT ( 'NONE',  ( -105.9577023256337185, -296.1008837772716333, -305.4191531795616470 ) ) ;
#61879 = CARTESIAN_POINT ( 'NONE',  ( -27.23884825033445978, -275.4982778080797630, -197.5144380451885979 ) ) ;
#61880 = CARTESIAN_POINT ( 'NONE',  ( -110.8931712491901749, -288.7402756840113511, -257.3375499817615832 ) ) ;
#61881 = CARTESIAN_POINT ( 'NONE',  ( -70.59552866683937111, -296.5233027525680995, -205.0140867333433334 ) ) ;
#61882 = VERTEX_POINT ( 'NONE', #52925 ) ;
#61883 = FACE_OUTER_BOUND ( 'NONE', #88462, .T. ) ;
#61884 = CARTESIAN_POINT ( 'NONE',  ( -99.31927630328665657, -287.0335818043434983, -229.1289188010974271 ) ) ;
#61885 = CARTESIAN_POINT ( 'NONE',  ( -39.08696827218560799, -296.1532395277390606, -347.0321460828203612 ) ) ;
#61886 = CARTESIAN_POINT ( 'NONE',  ( -105.6631424160158161, -285.5502410245010765, -244.3597104883670283 ) ) ;
#61887 = CARTESIAN_POINT ( 'NONE',  ( 18.72315065344179885, -275.3282999676742406, -322.7972955681944427 ) ) ;
#61888 = CARTESIAN_POINT ( 'NONE',  ( -112.5420391258298878, -291.4055387729696918, -254.2296795115352381 ) ) ;
#61889 = CARTESIAN_POINT ( 'NONE',  ( -32.36353232082194609, -284.2538528623061325, -194.7470828097350477 ) ) ;
#61890 = CARTESIAN_POINT ( 'NONE',  ( 15.42058298479754974, -293.1065686548539020, -214.2354055956243428 ) ) ;
#61891 = CARTESIAN_POINT ( 'NONE',  ( -102.8625357173389716, -290.4487604618014416, -302.5963097822548207 ) ) ;
#61892 = CARTESIAN_POINT ( 'NONE',  ( 128.9467878515196162, -299.5541904835127980, -195.3611179825600175 ) ) ;
#61893 = CARTESIAN_POINT ( 'NONE',  ( 154.3984422716669940, 19.39780977728399591, -12.47739260116905236 ) ) ;
#61894 = CARTESIAN_POINT ( 'NONE',  ( -107.2659097474429899, -264.6957166766804903, -305.4471583230359784 ) ) ;
#61895 = CARTESIAN_POINT ( 'NONE',  ( -47.14791445113996105, -284.6947006952134984, -346.0350627207626530 ) ) ;
#61896 = CARTESIAN_POINT ( 'NONE',  ( -69.91165696735023971, -286.9809262143061801, -337.9199732462171255 ) ) ;
#61897 = ORIENTED_EDGE ( 'NONE', *, *, #36317, .T. ) ;
#61898 = CARTESIAN_POINT ( 'NONE',  ( 30.31202254033113164, -280.0953339040042920, -242.1263896873278441 ) ) ;
#61899 = CARTESIAN_POINT ( 'NONE',  ( 31.83441851047345850, -275.6539562771033616, -304.2524577740957170 ) ) ;
#61900 = CARTESIAN_POINT ( 'NONE',  ( -110.0774823086269265, -280.7787490018314998, -252.7675276394120090 ) ) ;
#61901 = CARTESIAN_POINT ( 'NONE',  ( 104.9614017666556407, 114.4850001852085768, -281.3012701160373581 ) ) ;
#61902 = CARTESIAN_POINT ( 'NONE',  ( 34.03061303885380084, -280.4750190945214854, -297.6484631254596138 ) ) ;
#61903 = CARTESIAN_POINT ( 'NONE',  ( -110.8074603620060259, -282.7436680862338108, -257.0746221734004280 ) ) ;
#61904 = CARTESIAN_POINT ( 'NONE',  ( -36.22580109295046924, -299.8260745248370540, -194.3741156519464823 ) ) ;
#61905 = CARTESIAN_POINT ( 'NONE',  ( -28.88263444934930391, -295.4345110711901157, -342.9823661880266741 ) ) ;
#61906 = ORIENTED_EDGE ( 'NONE', *, *, #12664, .F. ) ;
#61907 = CARTESIAN_POINT ( 'NONE',  ( -28.02735765637791587, -290.8575379229812370, -197.4095014941110549 ) ) ;
#61908 = CARTESIAN_POINT ( 'NONE',  ( 39.03735201124917609, -276.3208549875936342, -279.7272370890412958 ) ) ;
#61909 = CARTESIAN_POINT ( 'NONE',  ( 29.08604667910517705, -275.1425530550601479, -239.9674884841780624 ) ) ;
#61910 = CARTESIAN_POINT ( 'NONE',  ( 7.067237077276159241, -273.5612970577896590, -207.7712323599128865 ) ) ;
#61911 = CARTESIAN_POINT ( 'NONE',  ( -32.12788024951596100, -272.1177395468341729, -195.5298027718906724 ) ) ;
#61912 = CARTESIAN_POINT ( 'NONE',  ( 180.2288731078812702, 214.9910457053126720, -24.90909090909092782 ) ) ;
#61913 = VECTOR ( 'NONE', #81959, 1000.000000000000000 ) ;
#61914 = LINE ( 'NONE', #83669, #77519 ) ;
#61915 = CARTESIAN_POINT ( 'NONE',  ( -37.52755671434548645, -284.1342414025808694, -343.6824772921255544 ) ) ;
#61916 = CARTESIAN_POINT ( 'NONE',  ( 19.04679684927533856, -284.0137909534382743, -321.3725098920343157 ) ) ;
#61917 = CARTESIAN_POINT ( 'NONE',  ( -87.75881478372605216, -284.6733862353213453, -217.4271287337541310 ) ) ;
#61918 = CARTESIAN_POINT ( 'NONE',  ( -41.92642186165905116, -275.5107209694161838, -344.0313078368051265 ) ) ;
#61919 = CARTESIAN_POINT ( 'NONE',  ( -26.54002244950858724, -284.7738365682291715, -343.8584321605129617 ) ) ;
#61920 = CARTESIAN_POINT ( 'NONE',  ( -110.8615457380539340, -276.9568481582520008, -276.1139129462578694 ) ) ;
#61921 = CARTESIAN_POINT ( 'NONE',  ( 198.6884013828325521, 64.61450673763174279, 9.555809373750800972 ) ) ;
#61922 = CARTESIAN_POINT ( 'NONE',  ( 28.13121531422804011, -276.1861268284859534, -237.3834980543300617 ) ) ;
#61923 = DIRECTION ( 'NONE',  ( 0.000000000000000000, -1.000000000000000000, 0.000000000000000000 ) ) ;
#61924 = CARTESIAN_POINT ( 'NONE',  ( -112.2466121693338295, -279.5696559271012802, -253.2318163756536649 ) ) ;
#61925 = EDGE_LOOP ( 'NONE', ( #91244, #84808, #6681, #61239 ) ) ;
#61926 = CARTESIAN_POINT ( 'NONE',  ( 198.6639115758706282, 17.12212513345059151, 10.45170682515551164 ) ) ;
#61927 = CARTESIAN_POINT ( 'NONE',  ( -37.99593755795142869, -287.9044470443560044, -194.5991390091889457 ) ) ;
#61928 = CARTESIAN_POINT ( 'NONE',  ( -86.60623650512609117, -294.9552560944425750, -324.4500002238842740 ) ) ;
#61929 = CARTESIAN_POINT ( 'NONE',  ( -114.0855863780710564, -289.9616909165201832, -265.4940131380938624 ) ) ;
#61930 = EDGE_CURVE ( 'NONE', #85436, #58191, #12352, .T. ) ;
#61931 = CARTESIAN_POINT ( 'NONE',  ( 25.82709335916489835, -285.2678952497789737, -231.7906948365903474 ) ) ;
#61933 = CARTESIAN_POINT ( 'NONE',  ( -69.43702529255786260, -289.8638040297339558, -203.6548155200333099 ) ) ;
#61932 = CARTESIAN_POINT ( 'NONE',  ( 35.70694275621561786, -286.2433843592186236, -279.2645268563812238 ) ) ;
#61934 = CARTESIAN_POINT ( 'NONE',  ( -101.3450524992450283, -286.2473712684401903, -234.3305891629819655 ) ) ;
#61935 = CARTESIAN_POINT ( 'NONE',  ( -34.39582984381018349, -275.0149512536929137, -345.3032456508428254 ) ) ;
#61936 = CARTESIAN_POINT ( 'NONE',  ( -29.52453639315038103, -284.5494708129585888, -194.5631472584524886 ) ) ;
#61937 = CARTESIAN_POINT ( 'NONE',  ( -97.50377935892751680, -299.1640323899787859, -225.5565875564690543 ) ) ;
#61938 = CARTESIAN_POINT ( 'NONE',  ( 36.75407569789460638, -285.3890465478248757, -257.6422897795365543 ) ) ;
#61939 = CARTESIAN_POINT ( 'NONE',  ( 34.56297956985122966, -282.3098040861296454, -256.3981476393850585 ) ) ;
#61940 = CARTESIAN_POINT ( 'NONE',  ( -15.46098991042042492, -290.7698964495539826, -342.3270414939656803 ) ) ;
#61941 = CARTESIAN_POINT ( 'NONE',  ( 208.4306832106270804, -142.7221692137691775, 0.000000000000000000 ) ) ;
#61942 = CYLINDRICAL_SURFACE ( 'NONE', #3492, 4.103083949679980691 ) ;
#61943 = CARTESIAN_POINT ( 'NONE',  ( -103.3331209589990038, -297.9848315658342699, -307.2708249365308006 ) ) ;
#61944 = CARTESIAN_POINT ( 'NONE',  ( -49.44011554625806326, -277.8977340686983553, -196.3433566639332071 ) ) ;
#61945 = CARTESIAN_POINT ( 'NONE',  ( -16.66022970355939847, -291.5099242788823517, -196.3581747903004100 ) ) ;
#61946 = CARTESIAN_POINT ( 'NONE',  ( -108.2221050657300765, -295.2209196503710587, -249.8085363459832422 ) ) ;
#61947 = CARTESIAN_POINT ( 'NONE',  ( 27.28077401663080792, -280.7113718197099388, -305.3636794913035146 ) ) ;
#61948 = CARTESIAN_POINT ( 'NONE',  ( 16.50500617276932402, -272.9042914306951388, -218.8875793137998471 ) ) ;
#61949 = CARTESIAN_POINT ( 'NONE',  ( 33.78125297579861552, -294.6245412795799439, -251.8470957023897085 ) ) ;
#61950 = CARTESIAN_POINT ( 'NONE',  ( 39.58706461736020543, -290.0519495502702512, -270.3284710469133074 ) ) ;
#61951 = CARTESIAN_POINT ( 'NONE',  ( -103.2411790222717087, -295.5383631549463530, -231.7866989438958569 ) ) ;
#61952 = CARTESIAN_POINT ( 'NONE',  ( 18.76610242438108500, -292.4987351209083499, -321.6811558648663549 ) ) ;
#61953 = ADVANCED_FACE ( 'NONE', ( #87505 ), #22652, .T. ) ;
#61954 = CARTESIAN_POINT ( 'NONE',  ( -92.12384150760014734, -292.6751418966863412, -221.2068201637980280 ) ) ;
#61955 = EDGE_CURVE ( 'NONE', #83166, #37793, #81804, .T. ) ;
#61956 = DIRECTION ( 'NONE',  ( 0.9693563597868444237, 0.2456588035076248677, -0.000000000000000000 ) ) ;
#61957 = CARTESIAN_POINT ( 'NONE',  ( -38.91127114659439457, -292.8347961503388319, -197.2164792571050214 ) ) ;
#61958 = FACE_OUTER_BOUND ( 'NONE', #47748, .T. ) ;
#61960 = CARTESIAN_POINT ( 'NONE',  ( -7.270246031502023421, -292.4579246911467862, -203.8426419889135843 ) ) ;
#61959 = CARTESIAN_POINT ( 'NONE',  ( -91.27452030472841216, -281.8346503915630024, -322.9886555450844412 ) ) ;
#61961 = CARTESIAN_POINT ( 'NONE',  ( 21.61001375088902776, -282.2191246445926822, -319.8959080874147389 ) ) ;
#61962 = CARTESIAN_POINT ( 'NONE',  ( -33.06416573163687644, -282.6664083488201982, -347.2341673600084277 ) ) ;
#61963 = CARTESIAN_POINT ( 'NONE',  ( 9.098239688096295907, -286.4127103745565819, -329.0412714693239877 ) ) ;
#61964 = CARTESIAN_POINT ( 'NONE',  ( 32.91988840049522480, -280.4158573086644992, -300.2620116619760324 ) ) ;
#61965 = CARTESIAN_POINT ( 'NONE',  ( 39.03834907244375785, -286.5590980742975376, -277.2589867325837076 ) ) ;
#61966 = DIRECTION ( 'NONE',  ( 0.000000000000000000, -1.000000000000000000, 0.000000000000000000 ) ) ;
#61967 = CARTESIAN_POINT ( 'NONE',  ( 33.11658072861089153, -295.4400758530240978, -292.3172349924735727 ) ) ;
#61968 = CARTESIAN_POINT ( 'NONE',  ( 33.64365787055034929, -277.3405534871892542, -298.7825623721442980 ) ) ;
#61969 = CARTESIAN_POINT ( 'NONE',  ( -39.69766389053298639, -279.6885039081295190, -197.3654668857656418 ) ) ;
#61970 = CARTESIAN_POINT ( 'NONE',  ( 39.44090743966724233, -293.6465202733311344, -264.5791477658112854 ) ) ;
#61971 = CARTESIAN_POINT ( 'NONE',  ( -1.088236823255665175, -280.6548145239515293, -336.6705762207873818 ) ) ;
#61972 = ADVANCED_FACE ( 'NONE', ( #38718 ), #36102, .T. ) ;
#61974 = CARTESIAN_POINT ( 'NONE',  ( 35.65801755045901444, -292.6880730879821044, -276.2305018100163920 ) ) ;
#61973 = VECTOR ( 'NONE', #71547, 1000.000000000000000 ) ;
#61975 = CARTESIAN_POINT ( 'NONE',  ( -94.04192548860704903, -295.2335761265449605, -221.1910238512157036 ) ) ;
#61976 = ORIENTED_EDGE ( 'NONE', *, *, #6158, .F. ) ;
#61977 = CARTESIAN_POINT ( 'NONE',  ( -4.314445822074130632, -294.1122834535618153, -335.5455879334134579 ) ) ;
#61978 = DIRECTION ( 'NONE',  ( -0.000000000000000000, -1.000000000000000000, -0.000000000000000000 ) ) ;
#61979 = AXIS2_PLACEMENT_3D ( 'NONE', #37587, #9645, #30982 ) ;
#61980 = CARTESIAN_POINT ( 'NONE',  ( 30.91033621190086578, -290.8380690714489560, -254.8156830097664738 ) ) ;
#61981 = CARTESIAN_POINT ( 'NONE',  ( -36.53163284054154758, -297.1208148081067861, -193.5965360629227803 ) ) ;
#61982 = CARTESIAN_POINT ( 'NONE',  ( 25.68106271542059105, -280.2543228823050754, -312.4139043813443664 ) ) ;
#61983 = CARTESIAN_POINT ( 'NONE',  ( -85.21742987243534628, -286.7216552534935090, -210.6852202275717900 ) ) ;
#61984 = CARTESIAN_POINT ( 'NONE',  ( -26.47698553936530530, -288.7435041215287583, -342.5991326974644835 ) ) ;
#61985 = CARTESIAN_POINT ( 'NONE',  ( -45.97024486336496096, -278.6835328600971025, -343.5986705769190053 ) ) ;
#61986 = CARTESIAN_POINT ( 'NONE',  ( -108.2617752005481151, -294.8764038408161241, -246.9124571777710173 ) ) ;
#61987 = CARTESIAN_POINT ( 'NONE',  ( -107.9680292408225597, -274.4347567752539021, -248.7765098765487437 ) ) ;
#61988 = CARTESIAN_POINT ( 'NONE',  ( -109.6800331247346350, -277.1831215343365216, -282.8570925155178202 ) ) ;
#61989 = ORIENTED_EDGE ( 'NONE', *, *, #87285, .T. ) ;
#61990 = CARTESIAN_POINT ( 'NONE',  ( -112.4428150783791551, -272.5980163036712156, -253.3663382617036177 ) ) ;
#61991 = CARTESIAN_POINT ( 'NONE',  ( -111.5562268422951888, -292.3893012345352531, -276.7779036592502848 ) ) ;
#61992 = CARTESIAN_POINT ( 'NONE',  ( 37.57452534993619508, -295.3291901494370677, -284.3600939016120606 ) ) ;
#61993 = FACE_OUTER_BOUND ( 'NONE', #75072, .T. ) ;
#61994 = CARTESIAN_POINT ( 'NONE',  ( -94.17831061124951475, -290.5542076525889570, -316.3338531345516458 ) ) ;
#61995 = CARTESIAN_POINT ( 'NONE',  ( -48.18343439339135159, -251.8661507411202365, -450.2476286390481164 ) ) ;
#61996 = EDGE_LOOP ( 'NONE', ( #18420, #43838 ) ) ;
#61997 = CARTESIAN_POINT ( 'NONE',  ( -113.5504586543767545, -297.0700329378709057, -281.0239587129651113 ) ) ;
#61998 = CARTESIAN_POINT ( 'NONE',  ( -99.67802396944000520, -288.1137912945842459, -313.4248871045240890 ) ) ;
#61999 = CARTESIAN_POINT ( 'NONE',  ( -54.59455488739089191, -298.1695626392007625, -195.3405655046613845 ) ) ;
#62000 = DIRECTION ( 'NONE',  ( 0.000000000000000000, 1.000000000000000000, 0.000000000000000000 ) ) ;
#62001 = CARTESIAN_POINT ( 'NONE',  ( 195.7694206965761623, 25.16799831920000940, 14.25285053635913535 ) ) ;
#62002 = CARTESIAN_POINT ( 'NONE',  ( -103.1902414082874770, -291.5646672956302154, -309.0230412759524370 ) ) ;
#62003 = CARTESIAN_POINT ( 'NONE',  ( 13.84574458161073096, -290.9090924074130839, -334.4957818155094174 ) ) ;
#62004 = CARTESIAN_POINT ( 'NONE',  ( -105.7799410536550226, -286.1549196048806607, -300.6305018968373588 ) ) ;
#62005 = CARTESIAN_POINT ( 'NONE',  ( 34.51213430789309911, -286.4594353561856792, -296.5078931113799285 ) ) ;
#62006 = CARTESIAN_POINT ( 'NONE',  ( -2.026527581831383706, -272.5208028060419565, -204.3848569729614439 ) ) ;
#62007 = CARTESIAN_POINT ( 'NONE',  ( -103.3178379009176666, -274.9336751837110455, -235.7753055979397345 ) ) ;
#62008 = CARTESIAN_POINT ( 'NONE',  ( -104.1483268116819971, -288.1956878634434247, -303.1969037359135086 ) ) ;
#62009 = CARTESIAN_POINT ( 'NONE',  ( -37.10662138636033802, -278.9096130583695867, -346.1384066330168139 ) ) ;
#62010 = ORIENTED_EDGE ( 'NONE', *, *, #60203, .F. ) ;
#62012 = CARTESIAN_POINT ( 'NONE',  ( 15.33858816733796360, -280.1692949061843478, -219.6066496645920836 ) ) ;
#62011 = CARTESIAN_POINT ( 'NONE',  ( -37.00832681121497103, -280.0564418895975223, -197.3618792041206689 ) ) ;
#62013 = CARTESIAN_POINT ( 'NONE',  ( 39.31510157568975927, -276.6777088617315030, -274.0154680389487680 ) ) ;
#62014 = CARTESIAN_POINT ( 'NONE',  ( 37.29412289443150286, -280.1295961886257828, -253.0551699148767568 ) ) ;
#62015 = CARTESIAN_POINT ( 'NONE',  ( -113.1081836994901408, -270.5045731412160990, -283.7362657651427185 ) ) ;
#62016 = CARTESIAN_POINT ( 'NONE',  ( 31.64909690800963560, -276.9282843539091346, -304.1436361792107164 ) ) ;
#62017 = EDGE_CURVE ( 'NONE', #10408, #3537, #38224, .T. ) ;
#62018 = CARTESIAN_POINT ( 'NONE',  ( -76.09742436145226918, -275.0647115253971720, -204.5680114361689732 ) ) ;
#62019 = CARTESIAN_POINT ( 'NONE',  ( 21.27581636871892101, -295.4090924074130839, -223.5744983911110353 ) ) ;
#62020 = ORIENTED_EDGE ( 'NONE', *, *, #77692, .T. ) ;
#62021 = B_SPLINE_CURVE_WITH_KNOTS ( 'NONE', 3,
 ( #22201, #66233, #15096, #30231, #59121, #79512, #86577, #23116 ),
 .UNSPECIFIED., .F., .F.,
 ( 4, 2, 2, 4 ),
 ( 0.000000000000000000, 0.0002353609534302958644, 0.0004707219068605917288, 0.0009414438137211129844 ),
 .UNSPECIFIED. ) ;
#62022 = DIRECTION ( 'NONE',  ( -0.000000000000000000, 1.000000000000000000, -0.000000000000000000 ) ) ;
#62023 = CARTESIAN_POINT ( 'NONE',  ( 18.00054895498326957, -287.9492933628943661, -222.2834564266263442 ) ) ;
#62024 = CARTESIAN_POINT ( 'NONE',  ( 37.96794746350486349, -289.1840281974967297, -260.2402982059978171 ) ) ;
#62025 = CARTESIAN_POINT ( 'NONE',  ( -53.43903441008619382, -288.6127324944325778, -341.6686806729079535 ) ) ;
#62026 = CARTESIAN_POINT ( 'NONE',  ( -46.49195521434227629, -285.4466288686685402, -193.9687117173135107 ) ) ;
#62027 = CARTESIAN_POINT ( 'NONE',  ( 152.9190334681021000, 20.54289017631687386, -11.30277777986246690 ) ) ;
#62028 = CARTESIAN_POINT ( 'NONE',  ( 32.10050812918746743, -280.2829370145910843, -295.4964954922735387 ) ) ;
#62029 = CARTESIAN_POINT ( 'NONE',  ( 36.35323700740005393, -289.5285428368790690, -279.3010128509669130 ) ) ;
#62030 = CARTESIAN_POINT ( 'NONE',  ( -43.00533730372855956, -281.6046660885201618, -343.8870566229210795 ) ) ;
#62031 = CARTESIAN_POINT ( 'NONE',  ( -110.4585283288373603, -279.9710658600658917, -262.4444270426106982 ) ) ;
#62032 = CARTESIAN_POINT ( 'NONE',  ( -68.05759070136770106, -277.9590193362187165, -336.6660712836229550 ) ) ;
#62033 = CARTESIAN_POINT ( 'NONE',  ( -106.1635557968894830, -288.9115243562584965, -304.1204208501723087 ) ) ;
#62034 = CARTESIAN_POINT ( 'NONE',  ( -114.0464436410450304, -285.2878630260869386, -275.7167332093262075 ) ) ;
#62035 = CARTESIAN_POINT ( 'NONE',  ( -7.372890411164062741, -286.9269605338669180, -199.4426914957515180 ) ) ;
#62036 = CARTESIAN_POINT ( 'NONE',  ( -3.619494781854760479, -282.7608040994583689, -335.1193343622798011 ) ) ;
#62037 = ORIENTED_EDGE ( 'NONE', *, *, #51756, .T. ) ;
#62038 = CARTESIAN_POINT ( 'NONE',  ( 159.4851178187871312, 17.02694846567680642, -9.999999999999998224 ) ) ;
#62039 = CARTESIAN_POINT ( 'NONE',  ( -112.9566010682902260, -292.4731156138514052, -265.5974813395214369 ) ) ;
#62040 = CARTESIAN_POINT ( 'NONE',  ( 15.11232305184130986, -291.4583789379362884, -214.5938944494969576 ) ) ;
#62041 = CARTESIAN_POINT ( 'NONE',  ( -35.37202290742290245, -273.1361887275465961, -197.1397696029900146 ) ) ;
#62042 = CARTESIAN_POINT ( 'NONE',  ( -98.19888279386984209, -295.2724616619329936, -317.3687355040290186 ) ) ;
#62043 = AXIS2_PLACEMENT_3D ( 'NONE', #82803, #76184, #9911 ) ;
#62044 = CARTESIAN_POINT ( 'NONE',  ( -27.99944512366560190, -290.6526229892918423, -197.2111179662545055 ) ) ;
#62045 = CARTESIAN_POINT ( 'NONE',  ( -0.2695385665357618032, -292.7921766650520112, -334.4791762848074086 ) ) ;
#62046 = CARTESIAN_POINT ( 'NONE',  ( -96.07689904917971546, -291.1424740988965709, -314.3969356862227755 ) ) ;
#62047 = CARTESIAN_POINT ( 'NONE',  ( 11.63197158325052172, -282.8906705383787994, 57.50000000000000000 ) ) ;
#62048 = CARTESIAN_POINT ( 'NONE',  ( -86.06528975434426343, -291.7272892425266377, -327.4469619221611651 ) ) ;
#62049 = CARTESIAN_POINT ( 'NONE',  ( 35.64796997533456846, -291.3218501120428527, -252.4018170869155711 ) ) ;
#62050 = CARTESIAN_POINT ( 'NONE',  ( -42.29319392709419390, -297.1147268780757713, -345.2101703396592143 ) ) ;
#62051 = CARTESIAN_POINT ( 'NONE',  ( 15.18995221619665159, -287.7579702751744435, -219.3333417226234019 ) ) ;
#62052 = CARTESIAN_POINT ( 'NONE',  ( 35.68489131738341769, -277.2943622563719259, -251.7728488861518770 ) ) ;
#62053 = CARTESIAN_POINT ( 'NONE',  ( -54.05961776822132947, -276.0569862513044654, -345.1718827872111319 ) ) ;
#62054 = CARTESIAN_POINT ( 'NONE',  ( -57.33782044864310024, -296.9977701891475022, -196.1148932415864010 ) ) ;
#62055 = CARTESIAN_POINT ( 'NONE',  ( 27.64593417192388358, -274.2701701604668756, -305.8882705148748187 ) ) ;
#62056 = CARTESIAN_POINT ( 'NONE',  ( -102.0517628199790607, -277.1262178491890040, -233.5654391325326458 ) ) ;
#62057 = CARTESIAN_POINT ( 'NONE',  ( -83.45188516503738185, -274.6085259240046526, -213.2561152291569897 ) ) ;
#62058 = CARTESIAN_POINT ( 'NONE',  ( -96.44692722915402783, -276.2997146413598557, -318.4753461207172904 ) ) ;
#62059 = CARTESIAN_POINT ( 'NONE',  ( 197.1844320129423807, 70.43964897667966341, 15.08154681515735440 ) ) ;
#62060 = CARTESIAN_POINT ( 'NONE',  ( -109.6848670926615199, -273.3465166235943684, -259.5097327623465731 ) ) ;
#62061 = DIRECTION ( 'NONE',  ( -0.000000000000000000, 1.000000000000000000, -0.000000000000000000 ) ) ;
#62063 = CARTESIAN_POINT ( 'NONE',  ( -0.5444365648930986623, -274.3891671933071734, -207.2992319510063339 ) ) ;
#62062 = CARTESIAN_POINT ( 'NONE',  ( -7.592971423522123509, -286.6842587832781533, -339.6095800180198125 ) ) ;
#62064 = CARTESIAN_POINT ( 'NONE',  ( 10.22794607770020825, -288.4168270954785953, -330.9775148117028039 ) ) ;
#62065 = CARTESIAN_POINT ( 'NONE',  ( -28.98369397163828509, -288.6158184824765272, -346.9384032508500013 ) ) ;
#62066 = CARTESIAN_POINT ( 'NONE',  ( -110.9921122315878961, -298.3283609184059628, -286.2992359406437686 ) ) ;
#62067 = CARTESIAN_POINT ( 'NONE',  ( 13.58431560165681873, -292.3372727882368167, -325.2643101730104149 ) ) ;
#62068 = CARTESIAN_POINT ( 'NONE',  ( 33.02916626481745510, -280.3549935369239847, -239.5050005480852917 ) ) ;
#62069 = CARTESIAN_POINT ( 'NONE',  ( 153.9755810662746569, 128.3195885613610869, -13.16651113973756715 ) ) ;
#62070 = CARTESIAN_POINT ( 'NONE',  ( 0.7186967764620975085, -278.5594444973312420, -205.7211978478155743 ) ) ;
#62071 = CARTESIAN_POINT ( 'NONE',  ( 199.9020372526622680, 288.4596041913513886, -5.812224296395849699 ) ) ;
#62072 = CARTESIAN_POINT ( 'NONE',  ( -80.65412912895703812, -288.4489736295436160, -329.6794475771482098 ) ) ;
#62073 = EDGE_CURVE ( 'NONE', #23700, #88648, #27648, .T. ) ;
#62074 = DIRECTION ( 'NONE',  ( 1.000000000000000000, 0.000000000000000000, 0.000000000000000000 ) ) ;
#62075 = CARTESIAN_POINT ( 'NONE',  ( 123.4306832106270946, -134.2391364535880882, 5.024999999999987921 ) ) ;
#62076 = CARTESIAN_POINT ( 'NONE',  ( -94.05253960020942827, -289.2327514533021713, -221.2807620594313107 ) ) ;
#62077 = CARTESIAN_POINT ( 'NONE',  ( -68.59406182953972575, -275.1539859244670083, -203.6090115705580388 ) ) ;
#62078 = CARTESIAN_POINT ( 'NONE',  ( 8.867009346162118888, -283.8574427595171983, -331.2163680439941231 ) ) ;
#62080 = CARTESIAN_POINT ( 'NONE',  ( -99.03103644794438765, -284.0116487594899013, -309.4868380060408981 ) ) ;
#62079 = CARTESIAN_POINT ( 'NONE',  ( -30.64117882779282453, -296.1557469306057442, -195.0081571552323680 ) ) ;
#62081 = CARTESIAN_POINT ( 'NONE',  ( -79.20506578675527010, -274.9005666449506293, -209.7778623687303536 ) ) ;
#62082 = CARTESIAN_POINT ( 'NONE',  ( -21.90991519230977502, -275.0578397395916568, -198.8456529409580185 ) ) ;
#62083 = EDGE_CURVE ( 'NONE', #59329, #36642, #61914, .T. ) ;
#62084 = CARTESIAN_POINT ( 'NONE',  ( 16.41112582024762645, -284.2891632781772842, -322.7386447316769136 ) ) ;
#62085 = CARTESIAN_POINT ( 'NONE',  ( -104.6581200486104564, -271.8624684733359231, -241.2027911472995072 ) ) ;
#62086 = VERTEX_POINT ( 'NONE', #4609 ) ;
#62087 = DIRECTION ( 'NONE',  ( -0.000000000000000000, -1.000000000000000000, -0.000000000000000000 ) ) ;
#62088 = CARTESIAN_POINT ( 'NONE',  ( 36.36906994952523320, -293.6669782561295960, -292.8065455158306349 ) ) ;
#62089 = CARTESIAN_POINT ( 'NONE',  ( -71.96299850839584167, -287.5719105631092702, -204.2308487871470675 ) ) ;
#62090 = DIRECTION ( 'NONE',  ( 0.000000000000000000, 0.000000000000000000, 1.000000000000000000 ) ) ;
#62091 = CARTESIAN_POINT ( 'NONE',  ( -37.37352853689063181, -280.5523547857346784, -350.3611179825600175 ) ) ;
#62092 = CARTESIAN_POINT ( 'NONE',  ( -70.24117767164770498, -276.6718362368798694, -339.8145869037289799 ) ) ;
#62093 = CARTESIAN_POINT ( 'NONE',  ( -93.02230521703508259, -288.2345469052291378, -322.4574771044648855 ) ) ;
#62094 = CARTESIAN_POINT ( 'NONE',  ( -6.950020853574732982, -284.1660580654667001, -337.5095568509012764 ) ) ;
#62095 =( BOUNDED_CURVE ( )  B_SPLINE_CURVE ( 3, ( #75752, #26020, #26504, #69588 ),
 .UNSPECIFIED., .F., .F. ) 
 B_SPLINE_CURVE_WITH_KNOTS ( ( 4, 4 ),
 ( 5.759586531581287971, 6.283185307179586232 ),
 .UNSPECIFIED. ) 
 CURVE ( )  GEOMETRIC_REPRESENTATION_ITEM ( )  RATIONAL_B_SPLINE_CURVE ( ( 1.000000000000000000, 0.9772838841927120601, 0.9772838841927120601, 1.000000000000000000 ) ) 
 REPRESENTATION_ITEM ( '' )  );
#62096 = CARTESIAN_POINT ( 'NONE',  ( -81.40494210337182324, -279.4209719899201332, -329.8287959066548751 ) ) ;
#62097 = CARTESIAN_POINT ( 'NONE',  ( -35.89203359648348624, -284.4596045891721019, -346.7711549717291746 ) ) ;
#62098 = CARTESIAN_POINT ( 'NONE',  ( -109.1115541506471089, -283.1446389177461356, -285.7902715749403910 ) ) ;
#62099 = CARTESIAN_POINT ( 'NONE',  ( 22.08545324069955029, -282.9252805419743595, -224.5864126013558462 ) ) ;
#62100 = CARTESIAN_POINT ( 'NONE',  ( 34.72100672315269065, -275.3756129215487363, -243.2324194187547732 ) ) ;
#62101 = CARTESIAN_POINT ( 'NONE',  ( -97.93022228132296902, -277.7502395641690214, -317.8798615246766417 ) ) ;
#62102 =( BOUNDED_CURVE ( )  B_SPLINE_CURVE ( 3, ( #38872, #73942, #8151, #1979 ),
 .UNSPECIFIED., .F., .T. ) 
 B_SPLINE_CURVE_WITH_KNOTS ( ( 4, 4 ),
 ( 3.141592653589793116, 4.712388980384689674 ),
 .UNSPECIFIED. ) 
 CURVE ( )  GEOMETRIC_REPRESENTATION_ITEM ( )  RATIONAL_B_SPLINE_CURVE ( ( 1.000000000000000000, 0.8047378541243649375, 0.8047378541243649375, 1.000000000000000000 ) ) 
 REPRESENTATION_ITEM ( '' )  );
#62103 = CARTESIAN_POINT ( 'NONE',  ( -17.81977085263746119, -296.7185993498702601, -342.1957090408149611 ) ) ;
#62104 = CARTESIAN_POINT ( 'NONE',  ( 120.8395553409046528, -299.5541904835127980, -198.3007743052732792 ) ) ;
#62105 = PLANE ( 'NONE',  #23920 ) ;
#62106 = AXIS2_PLACEMENT_3D ( 'NONE', #83989, #41349, #91551 ) ;
#62107 = CARTESIAN_POINT ( 'NONE',  ( -95.57745119697061398, -294.0290686025301170, -318.8467793659812628 ) ) ;
#62108 = CARTESIAN_POINT ( 'NONE',  ( 26.69348107032817552, -274.5784373497921820, -235.0777681290601606 ) ) ;
#62109 = CARTESIAN_POINT ( 'NONE',  ( -57.32248995891848864, -298.8799711926172336, -196.2637697770827288 ) ) ;
#62110 = AXIS2_PLACEMENT_3D ( 'NONE', #16315, #52746, #31004 ) ;
#62111 = CARTESIAN_POINT ( 'NONE',  ( 5.291014087692663459, -288.3975249725554022, -209.7969619150125880 ) ) ;
#62112 = CARTESIAN_POINT ( 'NONE',  ( -99.43294874909099690, -297.4783453547395879, -314.8052961785273851 ) ) ;
#62113 = CARTESIAN_POINT ( 'NONE',  ( -68.05282981142289600, -296.6515943598110994, -340.5382882952985142 ) ) ;
#62114 = CARTESIAN_POINT ( 'NONE',  ( -106.8055689469605056, -292.1872567177941278, -298.3352901802377346 ) ) ;
#62115 = CARTESIAN_POINT ( 'NONE',  ( -21.78912545874645090, -278.2516332011640543, -197.1085981219497683 ) ) ;
#62116 = CARTESIAN_POINT ( 'NONE',  ( -84.36596313540567849, -281.3198302490087599, -212.5879455084361496 ) ) ;
#62117 = CARTESIAN_POINT ( 'NONE',  ( -110.7876024639096215, -294.4751420900199150, -282.4860356768754741 ) ) ;
#62118 = CARTESIAN_POINT ( 'NONE',  ( -31.70417339903574572, -284.8421506815395787, -345.9289464635023705 ) ) ;
#62119 = CARTESIAN_POINT ( 'NONE',  ( 32.97033250405802107, -286.1985792965833184, -249.5696582420201821 ) ) ;
#62120 = CARTESIAN_POINT ( 'NONE',  ( 203.7290947897051581, 292.0717063975089332, -83.07512796522757981 ) ) ;
#62121 = ORIENTED_EDGE ( 'NONE', *, *, #4934, .F. ) ;
#62122 = CARTESIAN_POINT ( 'NONE',  ( -19.80666994010270443, -285.9505902719658934, -199.4766330582423279 ) ) ;
#62123 = ORIENTED_EDGE ( 'NONE', *, *, #35848, .F. ) ;
#62124 = CARTESIAN_POINT ( 'NONE',  ( 37.56658326136570736, -282.8390015065806438, -286.8608395150154706 ) ) ;
#62125 = CARTESIAN_POINT ( 'NONE',  ( -67.06999895155297509, -273.9846896992810343, -203.6517256073753970 ) ) ;
#62126 = CARTESIAN_POINT ( 'NONE',  ( -29.48830978224716759, -284.9444597675504838, -194.1618202281204049 ) ) ;
#62127 = CARTESIAN_POINT ( 'NONE',  ( 20.87979170948735330, -281.8158129399775476, -220.3103626705945146 ) ) ;
#62128 = DIRECTION ( 'NONE',  ( -0.000000000000000000, -0.9681751575201845705, 0.2502735790305593011 ) ) ;
#62129 = CARTESIAN_POINT ( 'NONE',  ( -69.68626442336800153, -281.1541948377401923, -201.2343622537274541 ) ) ;
#62130 = CARTESIAN_POINT ( 'NONE',  ( 24.57220920650583551, -281.2773509347484264, -224.6182264856387292 ) ) ;
#62131 = CARTESIAN_POINT ( 'NONE',  ( -21.39648532958014826, -280.3380690714490129, -340.3683826091709079 ) ) ;
#62132 = CARTESIAN_POINT ( 'NONE',  ( 204.3871895515903248, 295.4036489450776344, -54.00000000003383605 ) ) ;
#62133 = VERTEX_POINT ( 'NONE', #68552 ) ;
#62134 = CARTESIAN_POINT ( 'NONE',  ( -88.60735235691279854, -275.3316383907295517, -215.7753651459944422 ) ) ;
#62135 = CARTESIAN_POINT ( 'NONE',  ( 173.3098281514585040, 243.5254134702760211, -179.4893097426693771 ) ) ;
#62136 = CARTESIAN_POINT ( 'NONE',  ( 30.47740036453139822, -279.1594020060218782, -239.0535628851937702 ) ) ;
#62137 = CARTESIAN_POINT ( 'NONE',  ( 38.64185183667098755, -295.2754350200712565, -267.4527298032458589 ) ) ;
#62138 = CARTESIAN_POINT ( 'NONE',  ( -93.16559935020049465, -295.2307301742486061, -317.5778107881095593 ) ) ;
#62139 = CARTESIAN_POINT ( 'NONE',  ( -40.62351505635263038, -291.5196022840518708, -193.4795093570113806 ) ) ;
#62140 = CARTESIAN_POINT ( 'NONE',  ( 211.1232656141943949, 1.000000000000000000, -7.000000000000000888 ) ) ;
#62141 = EDGE_CURVE ( 'NONE', #77042, #3067, #75646, .T. ) ;
#62143 = CARTESIAN_POINT ( 'NONE',  ( 27.07551686922100842, -285.4635472034391910, -234.2445319275487918 ) ) ;
#62142 = CARTESIAN_POINT ( 'NONE',  ( -111.0286456077016908, -294.8716545358064991, -290.5809191632632178 ) ) ;
#62144 = CARTESIAN_POINT ( 'NONE',  ( 11.72985059892390503, -294.6020353073982392, -214.5893274861555255 ) ) ;
#62145 = EDGE_CURVE ( 'NONE', #46265, #51410, #48570, .T. ) ;
#62146 = CARTESIAN_POINT ( 'NONE',  ( -106.6331183573653618, -285.5417501068845922, -295.0062926344954235 ) ) ;
#62147 = EDGE_LOOP ( 'NONE', ( #60619, #69652, #43156, #46848, #28860, #69963 ) ) ;
#62148 = CARTESIAN_POINT ( 'NONE',  ( 37.55700646905299322, -294.7051800203935272, -287.2432111417434726 ) ) ;
#62149 = CARTESIAN_POINT ( 'NONE',  ( -45.64023667855260413, -283.6523760868956288, -343.0008779458037225 ) ) ;
#62150 = CARTESIAN_POINT ( 'NONE',  ( -113.2612344036847816, -295.2138434393336297, -280.9596399593287401 ) ) ;
#62151 = CARTESIAN_POINT ( 'NONE',  ( -95.54530537253452849, -292.0339637288088284, -220.1762832888179560 ) ) ;
#62152 = CARTESIAN_POINT ( 'NONE',  ( -109.4183958288736278, -291.3868878979236001, -243.2931504269986647 ) ) ;
#62153 = CARTESIAN_POINT ( 'NONE',  ( -94.94925562757360638, -290.0868885829125929, -315.2184576338083275 ) ) ;
#62154 = ORIENTED_EDGE ( 'NONE', *, *, #37168, .F. ) ;
#62155 = CARTESIAN_POINT ( 'NONE',  ( 221.8344101925596306, 35.72494958537217968, 10.00000000000000000 ) ) ;
#62156 = CARTESIAN_POINT ( 'NONE',  ( -76.42442664383926854, -297.4289509700955705, -335.3285831218125850 ) ) ;
#62157 = CARTESIAN_POINT ( 'NONE',  ( 7.645358440375352949, -297.2891121358272244, -193.8640699574521022 ) ) ;
#62158 = CARTESIAN_POINT ( 'NONE',  ( -43.75980346380193708, -279.0279412631193736, -197.3571999250343083 ) ) ;
#62159 = ORIENTED_EDGE ( 'NONE', *, *, #10818, .T. ) ;
#62160 = CARTESIAN_POINT ( 'NONE',  ( 37.88654482869483076, -274.8571148510014837, -254.1669164176647655 ) ) ;
#62161 = CARTESIAN_POINT ( 'NONE',  ( -80.11489271843522886, -295.9410960898944722, -210.3514375431061580 ) ) ;
#62162 = CARTESIAN_POINT ( 'NONE',  ( -10.79049564206102474, -278.5626062800440650, -339.6857097285516147 ) ) ;
#62163 = CARTESIAN_POINT ( 'NONE',  ( -16.26770224259139397, -272.4669118267210592, -199.1263901020467699 ) ) ;
#62164 = CARTESIAN_POINT ( 'NONE',  ( 4.052911788363070755, -295.6855722450789585, -330.9714851510532299 ) ) ;
#62165 = CARTESIAN_POINT ( 'NONE',  ( -58.00501875971919219, -298.8585124888522842, -200.0244039849526985 ) ) ;
#62166 = FACE_OUTER_BOUND ( 'NONE', #60506, .T. ) ;
#62167 = CARTESIAN_POINT ( 'NONE',  ( -103.8941601764363156, -297.6648574020217666, -307.5797208467027986 ) ) ;
#62168 = CARTESIAN_POINT ( 'NONE',  ( -20.98205275373969059, -296.2563299801637413, -195.2000046196192216 ) ) ;
#62169 = CARTESIAN_POINT ( 'NONE',  ( -37.55856933149814836, -292.7008172564774213, -197.2470453172807936 ) ) ;
#62170 = CARTESIAN_POINT ( 'NONE',  ( -110.5573194955301233, -289.2237879378496928, -262.9551746229625451 ) ) ;
#62171 = DIRECTION ( 'NONE',  ( -1.000000000000000000, 1.124465274301078034E-16, 0.000000000000000000 ) ) ;
#62172 = CARTESIAN_POINT ( 'NONE',  ( 39.31971637931158625, -276.1261469021078483, -276.8844700492973629 ) ) ;
#62173 = CARTESIAN_POINT ( 'NONE',  ( -64.57075795394921158, -273.8532170690698990, -202.6159731627336953 ) ) ;
#62174 = CARTESIAN_POINT ( 'NONE',  ( -40.95529554936418037, -281.9868107631513112, -195.0796935737309639 ) ) ;
#62175 = CARTESIAN_POINT ( 'NONE',  ( -78.90594608002184884, -282.2847860487191269, -334.5928214507551957 ) ) ;
#62176 = CARTESIAN_POINT ( 'NONE',  ( -67.67604294049554881, -276.7884704012433872, -341.0232749900562226 ) ) ;
#62177 = CARTESIAN_POINT ( 'NONE',  ( -106.6820819435996981, -284.0604918745594887, -246.8677466567403656 ) ) ;
#62178 = CARTESIAN_POINT ( 'NONE',  ( 23.60547888971174046, -280.1498402576630724, -314.3769318207641277 ) ) ;
#62179 = CARTESIAN_POINT ( 'NONE',  ( -59.63702038127579641, -272.3325145182950564, -200.1772273572711356 ) ) ;
#62180 = CARTESIAN_POINT ( 'NONE',  ( -83.89852987808885132, -279.6912897503808040, -329.2267780005162194 ) ) ;
#62181 = FACE_OUTER_BOUND ( 'NONE', #53484, .T. ) ;
#62182 = DIRECTION ( 'NONE',  ( 0.000000000000000000, -1.000000000000000000, 0.000000000000000000 ) ) ;
#62183 = CARTESIAN_POINT ( 'NONE',  ( -37.58166642864219398, -296.2890518265519972, -194.3748268903636358 ) ) ;
#62184 = AXIS2_PLACEMENT_3D ( 'NONE', #1087, #80153, #71682 ) ;
#62185 = CARTESIAN_POINT ( 'NONE',  ( -111.9020112372838298, -280.6794707972761671, -260.4358155944297550 ) ) ;
#62186 = VECTOR ( 'NONE', #28133, 1000.000000000000000 ) ;
#62187 = CARTESIAN_POINT ( 'NONE',  ( 156.5058941793770657, 215.0000000000001705, 17.26454883540702312 ) ) ;
#62188 = CARTESIAN_POINT ( 'NONE',  ( -68.56859125762616713, -285.3794172014340234, -339.1807501379173004 ) ) ;
#62189 = ORIENTED_EDGE ( 'NONE', *, *, #23558, .T. ) ;
#62190 = DIRECTION ( 'NONE',  ( -0.000000000000000000, -0.000000000000000000, -1.000000000000000000 ) ) ;
#62191 = CARTESIAN_POINT ( 'NONE',  ( -0.9852217125672030340, -286.5697797886974172, -336.0174713571342977 ) ) ;
#62192 = PLANE ( 'NONE',  #84529 ) ;
#62193 = CARTESIAN_POINT ( 'NONE',  ( -34.30001684065561562, -293.8079815565538411, -343.6951392033938077 ) ) ;
#62194 = CARTESIAN_POINT ( 'NONE',  ( -75.36864611930531055, -287.7044805633208853, -334.1319720925894217 ) ) ;
#62195 = CARTESIAN_POINT ( 'NONE',  ( 138.4517698930976621, 181.0451598467585939, -241.7086681466011271 ) ) ;
#62196 = CARTESIAN_POINT ( 'NONE',  ( -108.7819560547770976, -294.2553407669294643, -293.3612140365323171 ) ) ;
#62197 = CARTESIAN_POINT ( 'NONE',  ( -26.69848670156409298, -284.6649274932117919, -194.7473310146409915 ) ) ;
#62198 = CARTESIAN_POINT ( 'NONE',  ( 26.25870376865906408, -283.6620765842991432, -307.8978119973273806 ) ) ;
#62199 = CARTESIAN_POINT ( 'NONE',  ( 14.48677208943751360, -279.0087569188588077, -214.7213415024717449 ) ) ;
#62200 = CARTESIAN_POINT ( 'NONE',  ( -71.17275951027551173, -289.5117698735611498, -335.0626382165620498 ) ) ;
#62201 = CARTESIAN_POINT ( 'NONE',  ( -30.22331026722054048, -281.5691033478844361, -197.0662206807416794 ) ) ;
#62202 = CARTESIAN_POINT ( 'NONE',  ( -71.02509121847224094, -280.3986100589895045, -205.4006291246342641 ) ) ;
#62203 = CARTESIAN_POINT ( 'NONE',  ( 24.98251055041723490, -288.9610914447134746, -227.9812658396922984 ) ) ;
#62204 = ORIENTED_EDGE ( 'NONE', *, *, #79269, .T. ) ;
#62205 = CARTESIAN_POINT ( 'NONE',  ( -109.1666012014669604, -272.9053404859841407, -242.4621692476984549 ) ) ;
#62206 = CARTESIAN_POINT ( 'NONE',  ( -107.2599707565800173, -292.8747889406675426, -244.0746472647838061 ) ) ;
#62207 = DIRECTION ( 'NONE',  ( 0.000000000000000000, 0.000000000000000000, 1.000000000000000000 ) ) ;
#62208 = CARTESIAN_POINT ( 'NONE',  ( 36.57525178469696669, -289.6233781216987495, -234.7283546768995564 ) ) ;
#62209 = ORIENTED_EDGE ( 'NONE', *, *, #39485, .T. ) ;
#62210 = CARTESIAN_POINT ( 'NONE',  ( -3.572137588767112071, -274.6074148396185706, -337.5293354932284160 ) ) ;
#62211 = DIRECTION ( 'NONE',  ( 0.000000000000000000, 1.000000000000000000, 0.000000000000000000 ) ) ;
#62212 = CARTESIAN_POINT ( 'NONE',  ( -93.11793476103430578, -294.2367479262866823, -322.2980845871433644 ) ) ;
#62213 = CARTESIAN_POINT ( 'NONE',  ( -98.49564652132110609, -296.6144729756389324, -230.2922925035794890 ) ) ;
#62214 = CARTESIAN_POINT ( 'NONE',  ( 16.53092511624394589, -289.7893199401704010, -320.7194814161749719 ) ) ;
#62216 = EDGE_CURVE ( 'NONE', #44839, #64177, #62454, .T. ) ;
#62215 = CARTESIAN_POINT ( 'NONE',  ( -33.42042955250219194, -284.7622921157316682, -344.2832530809398008 ) ) ;
#62217 = CARTESIAN_POINT ( 'NONE',  ( -44.85729453125748734, -293.3841869319554689, -194.2683338550819769 ) ) ;
#62218 = CARTESIAN_POINT ( 'NONE',  ( -77.86092985218138551, -290.8991469505770056, -335.3189054361162675 ) ) ;
#62219 = CARTESIAN_POINT ( 'NONE',  ( -8.753996469251035251, -288.4263100696713309, -201.0093461868228530 ) ) ;
#62220 = CARTESIAN_POINT ( 'NONE',  ( -86.80634661059910684, -279.5529981287041323, -211.2810381927050685 ) ) ;
#62221 = CARTESIAN_POINT ( 'NONE',  ( -97.92297538639601839, -295.2443516461229365, -225.1817723909588267 ) ) ;
#62222 = CARTESIAN_POINT ( 'NONE',  ( -88.32312638259294602, -283.5763024639051650, -328.1375482307881271 ) ) ;
#62223 = CARTESIAN_POINT ( 'NONE',  ( 30.20020228012788976, -277.0026696384394427, -239.4317089190700756 ) ) ;
#62224 = CARTESIAN_POINT ( 'NONE',  ( 17.36665895637874613, -283.4090924074130839, -226.6919474004047572 ) ) ;
#62225 = CARTESIAN_POINT ( 'NONE',  ( -37.15419900124892649, -275.1893838209671799, -346.1385384650019432 ) ) ;
#62226 = DIRECTION ( 'NONE',  ( 0.000000000000000000, 0.000000000000000000, 1.000000000000000000 ) ) ;
#62227 = CARTESIAN_POINT ( 'NONE',  ( 29.36808933716896064, -281.4621798982450400, -300.2811593355019681 ) ) ;
#62228 = CARTESIAN_POINT ( 'NONE',  ( -98.47720799253986002, -279.1390823461998707, -316.5395301165770547 ) ) ;
#62229 = CARTESIAN_POINT ( 'NONE',  ( -87.58685523860694389, -284.4297309891798591, -212.2541756122675167 ) ) ;
#62230 = CARTESIAN_POINT ( 'NONE',  ( 34.28325986600994923, -295.0694365392945997, -251.7106723720840478 ) ) ;
#62231 = CARTESIAN_POINT ( 'NONE',  ( 36.50484994859345989, -276.9146598850203986, -251.5694320710709633 ) ) ;
#62232 = CARTESIAN_POINT ( 'NONE',  ( 36.80313869455389408, -276.6297516045722773, -251.4973656980204453 ) ) ;
#62233 = FACE_OUTER_BOUND ( 'NONE', #85988, .T. ) ;
#62234 = CARTESIAN_POINT ( 'NONE',  ( 26.76573876936310725, -275.8633748726827548, -305.3843496052797946 ) ) ;
#62235 = CARTESIAN_POINT ( 'NONE',  ( -76.59865566483408372, -297.5784857718181797, -334.1311727324882099 ) ) ;
#62236 = CARTESIAN_POINT ( 'NONE',  ( -111.2272806913039034, -282.7058103662303097, -258.4079084322780773 ) ) ;
#62237 = CARTESIAN_POINT ( 'NONE',  ( 37.74162592964486862, -293.0058193798369075, -253.3244163209103590 ) ) ;
#62238 = CARTESIAN_POINT ( 'NONE',  ( 37.76484639844176883, -288.9887539159295216, -257.4218512884738743 ) ) ;
#62239 = CARTESIAN_POINT ( 'NONE',  ( 25.11841529032293963, -291.9445315659485800, -231.8855585433479973 ) ) ;
#62240 = ORIENTED_EDGE ( 'NONE', *, *, #62639, .T. ) ;
#62241 = CARTESIAN_POINT ( 'NONE',  ( -7.404202894446433980, -291.0118138316977934, -200.0450368370763385 ) ) ;
#62242 = CARTESIAN_POINT ( 'NONE',  ( -38.89377451390601692, -291.6988662010831490, -197.3564705143335800 ) ) ;
#62243 = ORIENTED_EDGE ( 'NONE', *, *, #6158, .T. ) ;
#62244 = CARTESIAN_POINT ( 'NONE',  ( -96.14515598847482636, -290.9663796717601372, -319.6120225732753397 ) ) ;
#62245 = CARTESIAN_POINT ( 'NONE',  ( -68.53617384229421816, -279.9638232903423614, -204.3384529608535161 ) ) ;
#62246 = CARTESIAN_POINT ( 'NONE',  ( -73.12411131233280059, -296.5098503811270234, -202.4710213324340202 ) ) ;
#62247 = CARTESIAN_POINT ( 'NONE',  ( -26.64350433382007211, -286.8361129305421855, -194.1574349464007980 ) ) ;
#62248 = CARTESIAN_POINT ( 'NONE',  ( -33.73256646877940312, -286.4296850851458771, -193.4669150424163320 ) ) ;
#62249 = CARTESIAN_POINT ( 'NONE',  ( 9.925612838762564394, -282.7134201884878735, -326.0862959525955489 ) ) ;
#62250 = CARTESIAN_POINT ( 'NONE',  ( -107.9691066305277900, -262.3882541908849930, -317.6205384922552071 ) ) ;
#62251 = CARTESIAN_POINT ( 'NONE',  ( -64.72634346049389364, -182.0697847625480676, -361.3728755866533220 ) ) ;
#62252 = CARTESIAN_POINT ( 'NONE',  ( 178.4789072661037324, 251.8278643662533227, -164.2970973383132218 ) ) ;
#62253 = AXIS2_PLACEMENT_3D ( 'NONE', #17403, #24967, #89327 ) ;
#62254 = CARTESIAN_POINT ( 'NONE',  ( 30.42374033854767390, -275.1195021424367155, -298.0720726600726493 ) ) ;
#62255 = CARTESIAN_POINT ( 'NONE',  ( -6.157571474655167520, -275.5527995923927165, -336.7208263011962117 ) ) ;
#62256 = CARTESIAN_POINT ( 'NONE',  ( -113.7129358895308258, -296.1765255516202160, -261.0358163016437629 ) ) ;
#62257 = CARTESIAN_POINT ( 'NONE',  ( -87.60137065885514573, -230.3911852031648095, -345.0379683109082976 ) ) ;
#62258 = EDGE_CURVE ( 'NONE', #14370, #44128, #33711, .T. ) ;
#62259 = CARTESIAN_POINT ( 'NONE',  ( 33.26494053643585147, -273.8583473668449528, -240.7623666379177507 ) ) ;
#62260 = CARTESIAN_POINT ( 'NONE',  ( -107.2710463876148168, -274.6303226597171943, -246.1152823722235610 ) ) ;
#62261 = ORIENTED_EDGE ( 'NONE', *, *, #71290, .T. ) ;
#62262 = CARTESIAN_POINT ( 'NONE',  ( -71.27843577842449463, -274.6942235811085311, -201.5876457377155475 ) ) ;
#62263 = VECTOR ( 'NONE', #828, 1000.000000000000000 ) ;
#62264 = CARTESIAN_POINT ( 'NONE',  ( 32.72720757791289259, -287.7703440749824040, -249.6207029913926760 ) ) ;
#62265 = CARTESIAN_POINT ( 'NONE',  ( -101.4878145052344962, -296.7964816164920308, -312.7590373905729848 ) ) ;
#62266 = CARTESIAN_POINT ( 'NONE',  ( -111.9074532997213964, -296.8064591108852710, -289.3741227362523887 ) ) ;
#62267 = CARTESIAN_POINT ( 'NONE',  ( 8.229822628023377717, -294.5755523371689151, -327.4544666561328086 ) ) ;
#62268 = ORIENTED_EDGE ( 'NONE', *, *, #64378, .F. ) ;
#62269 = CARTESIAN_POINT ( 'NONE',  ( 20.64162240762772882, -278.1366667372432744, -318.8095287819680266 ) ) ;
#62270 = ORIENTED_EDGE ( 'NONE', *, *, #70753, .F. ) ;
#62271 = CARTESIAN_POINT ( 'NONE',  ( 37.61896585007993110, -280.8422093359563974, -252.9704270377555702 ) ) ;
#62272 = CARTESIAN_POINT ( 'NONE',  ( 17.61972441668371658, -277.1824857078469222, -318.7809730813240208 ) ) ;
#62273 = CARTESIAN_POINT ( 'NONE',  ( -48.32506735422127520, -278.9500972431155219, -345.6029948150822975 ) ) ;
#62274 = CARTESIAN_POINT ( 'NONE',  ( -88.12270743237529302, -275.7788769931800061, -326.0360324193958377 ) ) ;
#62275 = CARTESIAN_POINT ( 'NONE',  ( -92.96470659711444284, -273.7179062915847680, -222.9701921779713416 ) ) ;
#62276 = CARTESIAN_POINT ( 'NONE',  ( -63.79764198944837261, -293.9785674031145959, -339.0843076935979070 ) ) ;
#62277 = CARTESIAN_POINT ( 'NONE',  ( 151.7270317713903296, 20.05858947365025102, -8.551724154019398227 ) ) ;
#62278 = CARTESIAN_POINT ( 'NONE',  ( 15.11478982441561669, -281.2608826231216312, -214.0046946443562774 ) ) ;
#62279 = CARTESIAN_POINT ( 'NONE',  ( -104.4429021786955190, -279.1050151316099459, -241.6134452446196121 ) ) ;
#62280 = CARTESIAN_POINT ( 'NONE',  ( -31.87882060011769525, -287.6695438861580669, -346.7249042943355448 ) ) ;
#62281 = CARTESIAN_POINT ( 'NONE',  ( -96.25820521449435319, -275.1895370121113729, -223.9515706693634058 ) ) ;
#62282 = CARTESIAN_POINT ( 'NONE',  ( 197.0537578383379582, 24.40161896276961073, 12.19962234278438906 ) ) ;
#62283 = CARTESIAN_POINT ( 'NONE',  ( -61.31755919635303798, -288.5688196649106203, -339.4824599019588618 ) ) ;
#62284 = CARTESIAN_POINT ( 'NONE',  ( -99.25722516425169317, -284.5084307304362028, -224.6689048950553911 ) ) ;
#62285 = CARTESIAN_POINT ( 'NONE',  ( 19.25495086030587188, -280.4604971436399978, -318.0755753502187986 ) ) ;
#62287 = CARTESIAN_POINT ( 'NONE',  ( -111.5329183808475761, -282.5533272256720352, -276.4420167760204663 ) ) ;
#62286 = CARTESIAN_POINT ( 'NONE',  ( 34.80478897936795590, -280.3174573717301996, -284.9247679092526937 ) ) ;
#62288 = CARTESIAN_POINT ( 'NONE',  ( 37.64345686072064723, -289.5118462650171978, -267.2091669108579595 ) ) ;
#62289 = CARTESIAN_POINT ( 'NONE',  ( -110.7892205932846110, -279.7533807707761753, -270.6548755915363245 ) ) ;
#62290 = CARTESIAN_POINT ( 'NONE',  ( -114.0438498160389287, -273.6021560138187851, -270.3744733279939965 ) ) ;
#62291 = CARTESIAN_POINT ( 'NONE',  ( -55.72390417005674124, -293.8158264148777334, -197.5951775443839438 ) ) ;
#62292 = CARTESIAN_POINT ( 'NONE',  ( -72.39344909896090030, -275.7493423561646750, -337.7948328303848484 ) ) ;
#62293 = CARTESIAN_POINT ( 'NONE',  ( 32.19770090373580018, -276.5022262521604262, -292.9036194482267206 ) ) ;
#62294 = CARTESIAN_POINT ( 'NONE',  ( -2.461704542035739962, -284.5919402306911365, -336.9450074551469925 ) ) ;
#62295 = CARTESIAN_POINT ( 'NONE',  ( 199.6702811234769683, 65.52214591209386185, 9.100946541886340668 ) ) ;
#62296 = CARTESIAN_POINT ( 'NONE',  ( -59.57969948219484024, -291.2581091499336026, -342.5745902756821124 ) ) ;
#62297 = CARTESIAN_POINT ( 'NONE',  ( -43.72117530519366824, -293.1325884930290613, -345.1021094493497117 ) ) ;
#62298 = CARTESIAN_POINT ( 'NONE',  ( -29.46929581545144217, -285.3466380642558988, -193.9269366848511140 ) ) ;
#62299 = CARTESIAN_POINT ( 'NONE',  ( -93.14823700134739681, -289.6327189066530536, -222.0695984494056745 ) ) ;
#62300 = CARTESIAN_POINT ( 'NONE',  ( 195.4781563537916043, 39.36132622696000283, 14.00000000000000000 ) ) ;
#62301 = CARTESIAN_POINT ( 'NONE',  ( 35.19111776844810180, -274.3961652592252562, -282.5102284564745787 ) ) ;
#62302 = CARTESIAN_POINT ( 'NONE',  ( -66.56076885441905233, -293.5785622425982524, -338.6041506293255452 ) ) ;
#62303 = CARTESIAN_POINT ( 'NONE',  ( 196.0790001906461271, 41.35036787528040492, 14.17104486492339888 ) ) ;
#62304 = CARTESIAN_POINT ( 'NONE',  ( 199.4392256788250677, 65.82574266882504332, 7.741079165001067963 ) ) ;
#62305 = CARTESIAN_POINT ( 'NONE',  ( -113.6965737442166358, -289.0214237832831827, -271.2016239971042069 ) ) ;
#62306 = CARTESIAN_POINT ( 'NONE',  ( -111.1908020677759765, -286.1447916747094951, -270.9356432036289561 ) ) ;
#62307 = CARTESIAN_POINT ( 'NONE',  ( 4.974180390718086819, -286.7285756609774694, -333.4748270157836600 ) ) ;
#62308 = CARTESIAN_POINT ( 'NONE',  ( -109.5542299297093933, -285.7920277897581514, -284.5288792083869680 ) ) ;
#62309 = CARTESIAN_POINT ( 'NONE',  ( 140.6539576904058606, 275.0000000000000568, -11.50000000000000000 ) ) ;
#62310 = CARTESIAN_POINT ( 'NONE',  ( -10.70067695605413149, -287.2115324048096454, -202.2090452305314727 ) ) ;
#62311 = CARTESIAN_POINT ( 'NONE',  ( 10.06405564870831704, -294.6812964441883764, -211.7184013412460502 ) ) ;
#62312 = CARTESIAN_POINT ( 'NONE',  ( -112.9444886269548505, -276.6167081423948275, -271.5606673702270086 ) ) ;
#62313 = CIRCLE ( 'NONE', #24445, 1.000000000000000888 ) ;
#62314 = CARTESIAN_POINT ( 'NONE',  ( 12.69409406138459673, -276.7094762035383724, -328.8603794417296058 ) ) ;
#62315 = CIRCLE ( 'NONE', #25996, 20.00000000000000355 ) ;
#62316 = CARTESIAN_POINT ( 'NONE',  ( 32.01253885703746960, -291.2425904643599210, -240.3727247253076769 ) ) ;
#62317 = CARTESIAN_POINT ( 'NONE',  ( -53.76047810733812327, -279.8471846651020201, -195.0774075345661913 ) ) ;
#62318 = CARTESIAN_POINT ( 'NONE',  ( -83.35431795387779630, -297.6657019384484784, -329.2035771400176145 ) ) ;
#62319 = CARTESIAN_POINT ( 'NONE',  ( -48.18343439339133027, -256.8217696174888829, -487.2503612923645733 ) ) ;
#62320 = DIRECTION ( 'NONE',  ( -1.000000000000000000, -0.000000000000000000, -0.000000000000000000 ) ) ;
#62321 = CARTESIAN_POINT ( 'NONE',  ( -60.11565295431227440, -284.4354952349557379, -200.4855818491412549 ) ) ;
#62322 = CARTESIAN_POINT ( 'NONE',  ( -111.5857481016875994, -276.7243928445810184, -267.8431239756961872 ) ) ;
#62323 = CARTESIAN_POINT ( 'NONE',  ( 35.73472859122758649, -279.3346401917989397, -253.4275152831069704 ) ) ;
#62324 = DIRECTION ( 'NONE',  ( 0.000000000000000000, 0.000000000000000000, 1.000000000000000000 ) ) ;
#62325 = CARTESIAN_POINT ( 'NONE',  ( 37.81265487832424554, -273.8643681791504036, -257.0753435488216496 ) ) ;
#62326 = CARTESIAN_POINT ( 'NONE',  ( -105.3656794337780980, -277.5432412610031747, -297.1310807648108607 ) ) ;
#62327 = CIRCLE ( 'NONE', #53249, 5.654241149514405151 ) ;
#62328 = CARTESIAN_POINT ( 'NONE',  ( 35.59117400344509008, -294.9342921106934341, -259.8015903632006030 ) ) ;
#62329 = CARTESIAN_POINT ( 'NONE',  ( -33.91527017283922874, -279.0146453053664004, -193.7468106495906568 ) ) ;
#62330 = CARTESIAN_POINT ( 'NONE',  ( -45.10379467290600530, -296.0939746842353202, -343.2345443711770372 ) ) ;
#62331 = CARTESIAN_POINT ( 'NONE',  ( -101.1477144667957759, -298.4264383768374387, -228.1224375188270983 ) ) ;
#62332 = CARTESIAN_POINT ( 'NONE',  ( -88.12421900725803425, -297.1507672713754005, -217.8488087742622383 ) ) ;
#62333 = CARTESIAN_POINT ( 'NONE',  ( -50.05206480986360873, -293.8902599599312566, -196.3932482834451605 ) ) ;
#62334 = CARTESIAN_POINT ( 'NONE',  ( -65.87933393469943155, -285.8556564122085888, -198.8305073732281585 ) ) ;
#62335 = CARTESIAN_POINT ( 'NONE',  ( 38.08996893649335647, -273.5947266555241981, -262.7287153336583287 ) ) ;
#62336 = CARTESIAN_POINT ( 'NONE',  ( 24.14092809487967628, -288.0027541231248165, -316.7172009849429060 ) ) ;
#62337 = CARTESIAN_POINT ( 'NONE',  ( -49.43261822015174545, -281.8771459112280695, -196.7020621924338002 ) ) ;
#62338 = CARTESIAN_POINT ( 'NONE',  ( 17.99546967229176175, -287.2930537704831409, -318.4079180155812310 ) ) ;
#62339 = CARTESIAN_POINT ( 'NONE',  ( -110.9112672685687642, -288.3639759336571160, -285.0043701770196094 ) ) ;
#62340 = CARTESIAN_POINT ( 'NONE',  ( 197.9738562182569694, 291.4636489450775798, -54.00000000000003553 ) ) ;
#62341 = CARTESIAN_POINT ( 'NONE',  ( 5.875982438000423969, -287.9562129263955512, -329.3327402905377994 ) ) ;
#62342 = CARTESIAN_POINT ( 'NONE',  ( 175.2296996224750103, 140.2072866198470251, -24.00000000000002132 ) ) ;
#62343 = CARTESIAN_POINT ( 'NONE',  ( 24.07408639797774441, -283.1082028506222059, -316.4145801655532750 ) ) ;
#62344 = CARTESIAN_POINT ( 'NONE',  ( -69.51358087324699397, -290.6977654384454013, -200.6489710628453338 ) ) ;
#62345 = CARTESIAN_POINT ( 'NONE',  ( 38.73191045385964770, -283.2183039940754838, -275.5855336575278898 ) ) ;
#62346 = CARTESIAN_POINT ( 'NONE',  ( -45.23923029067531587, -281.2694123057322031, -194.2103242226465625 ) ) ;
#62347 = CARTESIAN_POINT ( 'NONE',  ( 13.92316989062081056, -282.1419199862598362, -322.4025980071550634 ) ) ;
#62348 = CARTESIAN_POINT ( 'NONE',  ( 21.40665245858204102, -276.9115181653517652, -223.7183545380449061 ) ) ;
#62349 = CARTESIAN_POINT ( 'NONE',  ( -94.65157633605407739, -295.8542301174773002, -321.8062239351966127 ) ) ;
#62350 = CARTESIAN_POINT ( 'NONE',  ( -91.80985505795345603, -287.8533485217014913, -321.4764849362650807 ) ) ;
#62351 = CARTESIAN_POINT ( 'NONE',  ( -91.40468242996172421, -272.0558860269956085, -220.7005550978051076 ) ) ;
#62352 = ORIENTED_EDGE ( 'NONE', *, *, #41624, .T. ) ;
#62353 = VERTEX_POINT ( 'NONE', #41979 ) ;
#62354 = CARTESIAN_POINT ( 'NONE',  ( -96.24110771372400563, -285.8435248029016975, -315.9030550999602269 ) ) ;
#62355 = CARTESIAN_POINT ( 'NONE',  ( -50.40130165100462278, -296.2946767704760873, -345.9856021812352083 ) ) ;
#62356 = CARTESIAN_POINT ( 'NONE',  ( -4.774309824762142718, -283.2628284514468078, -335.8077203189584452 ) ) ;
#62357 = ADVANCED_FACE ( 'NONE', ( #6959 ), #78462, .F. ) ;
#62358 = CARTESIAN_POINT ( 'NONE',  ( 21.54240632842849124, -275.2757235098295610, -319.6103029564845883 ) ) ;
#62359 = CARTESIAN_POINT ( 'NONE',  ( -97.38917831966689675, -291.8478637371387663, -222.3234957470463655 ) ) ;
#62360 = CARTESIAN_POINT ( 'NONE',  ( -112.9769329981831305, -282.6250433140344853, -275.6082475782509391 ) ) ;
#62361 = CARTESIAN_POINT ( 'NONE',  ( 33.30330949930436191, -293.4956629715330791, -239.7829083196810416 ) ) ;
#62362 = CARTESIAN_POINT ( 'NONE',  ( -97.36386924569266910, -290.3059262529394005, -311.9694601597855694 ) ) ;
#62363 = DIRECTION ( 'NONE',  ( 1.000000000000000000, -0.000000000000000000, 0.000000000000000000 ) ) ;
#62364 = DIRECTION ( 'NONE',  ( 0.000000000000000000, 0.000000000000000000, -1.000000000000000000 ) ) ;
#62365 = CARTESIAN_POINT ( 'NONE',  ( -101.7143074437604326, -254.4836201735207624, -324.1852191778334031 ) ) ;
#62366 = CARTESIAN_POINT ( 'NONE',  ( -92.91321726759508692, -285.3518244813142815, -322.6728513055225562 ) ) ;
#62367 = CARTESIAN_POINT ( 'NONE',  ( -20.25526795762938548, -280.3380690714491266, -345.3683826091709648 ) ) ;
#62368 = VERTEX_POINT ( 'NONE', #57164 ) ;
#62369 = CARTESIAN_POINT ( 'NONE',  ( 18.72190567208880196, -281.1408569231107322, -317.6151018503476848 ) ) ;
#62370 = CARTESIAN_POINT ( 'NONE',  ( -20.13496104240586249, -276.5037457805761960, -345.4469640604518190 ) ) ;
#62371 = CARTESIAN_POINT ( 'NONE',  ( -101.0413650427625925, -281.0817090332643602, -230.9890489329771981 ) ) ;
#62372 = CARTESIAN_POINT ( 'NONE',  ( 169.5298778015222467, 230.0351857080673597, -191.1287857711722893 ) ) ;
#62373 = CARTESIAN_POINT ( 'NONE',  ( 1.093412870664322689, -279.1290506314940671, -204.2603646273037157 ) ) ;
#62374 = CARTESIAN_POINT ( 'NONE',  ( -111.9642018374680390, -282.5293493250019310, -273.6868261862858844 ) ) ;
#62375 = CARTESIAN_POINT ( 'NONE',  ( -35.52496992298293321, -299.8347340750885905, -194.3739090059161754 ) ) ;
#62376 = CARTESIAN_POINT ( 'NONE',  ( 34.96774734480509039, -293.9066831759812999, -259.9049117941014515 ) ) ;
#62377 = ORIENTED_EDGE ( 'NONE', *, *, #26867, .T. ) ;
#62378 = CARTESIAN_POINT ( 'NONE',  ( -102.8415333438375825, -289.6879897458907180, -236.9166185282000470 ) ) ;
#62379 = CARTESIAN_POINT ( 'NONE',  ( -62.36497023060947242, -278.0205783917635927, -343.1301319342535976 ) ) ;
#62380 = CARTESIAN_POINT ( 'NONE',  ( 35.02050904442798895, -275.4251344293097077, -260.7324792587318143 ) ) ;
#62381 = CARTESIAN_POINT ( 'NONE',  ( 37.87649728430607610, -274.6602989537010444, -285.3182329698734065 ) ) ;
#62382 = DIRECTION ( 'NONE',  ( -0.3024135303179443235, -0.9531768234071985590, -1.474514954580288870E-14 ) ) ;
#62383 = CARTESIAN_POINT ( 'NONE',  ( -112.1851880641518591, -270.6236085282212684, -264.7831444951723938 ) ) ;
#62384 = EDGE_CURVE ( 'NONE', #1828, #17769, #21619, .T. ) ;
#62385 = CARTESIAN_POINT ( 'NONE',  ( 221.5917695054403111, 1.242640687119284992, -10.00000000000000000 ) ) ;
#62386 = AXIS2_PLACEMENT_3D ( 'NONE', #14444, #215, #42824 ) ;
#62387 = CARTESIAN_POINT ( 'NONE',  ( -43.53082812742030683, -249.2383276863598383, -481.7579445234451327 ) ) ;
#62388 = B_SPLINE_CURVE_WITH_KNOTS ( 'NONE', 3,
 ( #65758, #80379, #29747, #1779, #52433, #9330, #73304, #868, #8867, #30663, #59565, #88415, #87469, #22616, #38212, #60031, #23565, #67126, #51491, #8415, #37294, #66200, #16454, #59088 ),
 .UNSPECIFIED., .F., .F.,
 ( 4, 2, 2, 2, 2, 2, 2, 2, 2, 2, 2, 4 ),
 ( 0.000000000000000000, 0.06250000000000000000, 0.1250000000000000000, 0.2500000000000000000, 0.3750000000000000000, 0.5000000000000000000, 0.6250000000000000000, 0.7500000000000000000, 0.8125000000000000000, 0.8750000000000000000, 0.9375000000000000000, 1.000000000000000000 ),
 .UNSPECIFIED. ) ;
#62389 = TOROIDAL_SURFACE ( 'NONE', #86555, 160.1282194813176716, 1.000000000000000000 ) ;
#62390 = CARTESIAN_POINT ( 'NONE',  ( 14.15155330994995708, -283.3880706110204528, -322.6118245859823332 ) ) ;
#62391 = CARTESIAN_POINT ( 'NONE',  ( 31.48419404549470002, -283.7315166635507353, -302.6871839486440194 ) ) ;
#62392 = CARTESIAN_POINT ( 'NONE',  ( -110.3294487919163487, -283.9654290596298551, -265.4501027286298722 ) ) ;
#62393 = CARTESIAN_POINT ( 'NONE',  ( -54.15578548279486171, -275.6713989405343455, -342.2729103553705841 ) ) ;
#62394 = CARTESIAN_POINT ( 'NONE',  ( 34.95808848542053227, -283.1941045221067839, -253.5205107959050963 ) ) ;
#62395 = CARTESIAN_POINT ( 'NONE',  ( -29.66022299610497015, -275.4331448678845504, -343.7044069217980109 ) ) ;
#62397 = CARTESIAN_POINT ( 'NONE',  ( 159.4851178187871312, 15.00000000000000000, 7.000000000000000000 ) ) ;
#62396 =( GEOMETRIC_REPRESENTATION_CONTEXT ( 3 ) GLOBAL_UNCERTAINTY_ASSIGNED_CONTEXT ( ( #25414 ) ) GLOBAL_UNIT_ASSIGNED_CONTEXT ( ( #24432, #51915, #52845 ) ) REPRESENTATION_CONTEXT ( 'NONE', 'WORKASPACE' ) );
#62398 = CARTESIAN_POINT ( 'NONE',  ( 19.22865231693831589, -275.9737913726957004, -223.7347166756766228 ) ) ;
#62399 = CARTESIAN_POINT ( 'NONE',  ( 175.2296996224750103, 250.5000000000000568, 0.000000000000000000 ) ) ;
#62400 = CONICAL_SURFACE ( 'NONE', #27660, 24.00000000000001066, 0.7853981633974361776 ) ;
#62401 = CARTESIAN_POINT ( 'NONE',  ( -62.00549743442884676, -280.5424472260224888, -197.5323689875521325 ) ) ;
#62402 = ORIENTED_EDGE ( 'NONE', *, *, #17632, .T. ) ;
#62403 = LINE ( 'NONE', #91721, #48920 ) ;
#62404 = CARTESIAN_POINT ( 'NONE',  ( -49.17555213449553264, -287.7634478231784669, -195.4733212497631314 ) ) ;
#62405 = CARTESIAN_POINT ( 'NONE',  ( -69.80489281814210756, -294.6881784786021399, -335.9259168298979716 ) ) ;
#62406 = CARTESIAN_POINT ( 'NONE',  ( -99.79234140298613909, -289.3049936502433752, -315.2527150401634231 ) ) ;
#62407 = CARTESIAN_POINT ( 'NONE',  ( 34.70178695010155678, -285.5706038365906920, -253.3442598677782485 ) ) ;
#62409 = CARTESIAN_POINT ( 'NONE',  ( -94.20416234706810599, -289.4552210628647799, -222.9637676311234316 ) ) ;
#62408 = CARTESIAN_POINT ( 'NONE',  ( 36.24421497864828012, -286.1360139554283819, -271.0596974885449981 ) ) ;
#62410 = CARTESIAN_POINT ( 'NONE',  ( -99.35836934679360866, -285.2165302608587467, -309.7126131320366085 ) ) ;
#62411 = CARTESIAN_POINT ( 'NONE',  ( -37.15812013368570632, -275.0496619246393948, -345.3736166798979639 ) ) ;
#62412 = CARTESIAN_POINT ( 'NONE',  ( -21.13405276700971669, -284.6566193647917089, -195.9047375949826062 ) ) ;
#62413 = CARTESIAN_POINT ( 'NONE',  ( -62.20663637494677545, -299.7289374520364049, -199.6028280573134737 ) ) ;
#62414 = CARTESIAN_POINT ( 'NONE',  ( 17.04307828501119104, -284.8245188364803084, -218.3984126723973134 ) ) ;
#62415 = CARTESIAN_POINT ( 'NONE',  ( -49.19174876028269239, -280.8386729497715351, -198.0908973176059646 ) ) ;
#62416 = CARTESIAN_POINT ( 'NONE',  ( -10.20096042202992237, -290.6988631622684238, -340.4568288000978669 ) ) ;
#62417 = DIRECTION ( 'NONE',  ( 0.000000000000000000, 0.000000000000000000, -1.000000000000000000 ) ) ;
#62418 = DIRECTION ( 'NONE',  ( -0.4646852846009910110, 0.2294442726657860421, -0.8552326654286331875 ) ) ;
#62419 = CARTESIAN_POINT ( 'NONE',  ( -67.62615583989033041, -297.3665570891805032, -339.5865897590450686 ) ) ;
#62420 = AXIS2_PLACEMENT_3D ( 'NONE', #84778, #4786, #62090 ) ;
#62421 = CARTESIAN_POINT ( 'NONE',  ( -108.3297018451442426, -276.8668976356065627, -246.0004692778863102 ) ) ;
#62422 = CARTESIAN_POINT ( 'NONE',  ( 23.85284377214213336, -292.1285575222582906, -223.8702619586156857 ) ) ;
#62423 = CARTESIAN_POINT ( 'NONE',  ( -109.2520098646687359, -295.1685481382422722, -253.7675116425085946 ) ) ;
#62424 = CARTESIAN_POINT ( 'NONE',  ( 29.42767931392143410, -279.8240132139270600, -239.5292703110461048 ) ) ;
#62425 = CARTESIAN_POINT ( 'NONE',  ( 8.231418428188186809, -272.7610376279750426, -211.5019210804418321 ) ) ;
#62426 = CARTESIAN_POINT ( 'NONE',  ( 29.94826031768689134, -295.2622187699211054, -299.9128472022380834 ) ) ;
#62427 = CARTESIAN_POINT ( 'NONE',  ( 31.95455697924148097, -289.6233781216988064, -236.9535640164627353 ) ) ;
#62428 = CARTESIAN_POINT ( 'NONE',  ( -99.45551301604132277, -294.4385924375687864, -314.7737509732767762 ) ) ;
#62429 = CARTESIAN_POINT ( 'NONE',  ( -16.80261486949788718, -293.0304192470185853, -343.5738033895680132 ) ) ;
#62430 = CARTESIAN_POINT ( 'NONE',  ( -98.80157278307707713, -292.5353156550247036, -229.7955823903595274 ) ) ;
#62431 = CARTESIAN_POINT ( 'NONE',  ( 0.000000000000000000, 15.00000000000000000, 10.00000000000000000 ) ) ;
#62432 = CARTESIAN_POINT ( 'NONE',  ( -90.88431813285613714, -292.0704497226151375, -220.4848967948219354 ) ) ;
#62433 = DIRECTION ( 'NONE',  ( 0.000000000000000000, 1.000000000000000000, -0.000000000000000000 ) ) ;
#62435 = CARTESIAN_POINT ( 'NONE',  ( -6.041630355387678009, -292.4753562337936614, -204.3980705274468335 ) ) ;
#62434 = CARTESIAN_POINT ( 'NONE',  ( -44.29314567706702377, -281.1596327508506192, -345.4472234807956852 ) ) ;
#62436 = CARTESIAN_POINT ( 'NONE',  ( -3.657608455576050410, -280.4844072356609104, -201.1051240153441029 ) ) ;
#62437 = CARTESIAN_POINT ( 'NONE',  ( -94.38633936651712020, -283.5163525430716049, -322.0687089692151517 ) ) ;
#62438 = CARTESIAN_POINT ( 'NONE',  ( -5.023155395706768722, -286.6255172733480094, -337.8558592423685241 ) ) ;
#62439 = CARTESIAN_POINT ( 'NONE',  ( -59.33632811234290472, -281.4793595096010108, -341.3172225293729980 ) ) ;
#62440 = CARTESIAN_POINT ( 'NONE',  ( 3.467677775316871269, -279.0697180669168915, -205.8215476114294518 ) ) ;
#62441 = CARTESIAN_POINT ( 'NONE',  ( 25.30059580559607824, -285.8844116762513181, -226.0955590603487053 ) ) ;
#62442 = CARTESIAN_POINT ( 'NONE',  ( 196.8872833010042598, 42.02416330566288138, 12.48796469961283684 ) ) ;
#62443 = CARTESIAN_POINT ( 'NONE',  ( 34.85440377562154879, -295.3527501364723094, -285.7241969558337473 ) ) ;
#62444 = CARTESIAN_POINT ( 'NONE',  ( -53.98508847651596909, -278.6869110234774780, -344.9914994142048954 ) ) ;
#62445 = CARTESIAN_POINT ( 'NONE',  ( -96.11254663185624736, -277.6114152121239158, -313.7188419019598200 ) ) ;
#62446 = CARTESIAN_POINT ( 'NONE',  ( -95.66230492618028336, -291.3979140027301469, -220.0646567606551969 ) ) ;
#62447 = CIRCLE ( 'NONE', #9555, 7.500000000000012434 ) ;
#62448 = CARTESIAN_POINT ( 'NONE',  ( 8.318817480842051637, -280.5125548425954776, -330.5643681182293108 ) ) ;
#62449 = CARTESIAN_POINT ( 'NONE',  ( 31.05239761278816246, -292.2623130835193592, -244.1760871081505684 ) ) ;
#62450 = VECTOR ( 'NONE', #3586, 1000.000000000000000 ) ;
#62451 = CARTESIAN_POINT ( 'NONE',  ( -104.1870360930141430, -294.1010451502096998, -304.4859149042151785 ) ) ;
#62452 = EDGE_LOOP ( 'NONE', ( #17660, #43571, #75751, #4040 ) ) ;
#62453 = CARTESIAN_POINT ( 'NONE',  ( 17.06571399127465583, -89.54582641780471874, 21.50000000000000000 ) ) ;
#62454 = CIRCLE ( 'NONE', #56378, 0.5000000000000004441 ) ;
#62455 = CARTESIAN_POINT ( 'NONE',  ( 35.26734991781270168, -293.1726653885826863, -278.9239710856059560 ) ) ;
#62456 = CARTESIAN_POINT ( 'NONE',  ( 133.0872704186301405, -299.5541904835127980, -195.3611179825600175 ) ) ;
#62457 = CARTESIAN_POINT ( 'NONE',  ( -109.1418805571601069, -288.0523547857347353, -270.3284710469131937 ) ) ;
#62458 = CARTESIAN_POINT ( 'NONE',  ( -94.95860783121142390, -272.4391540804525675, -219.5236242650188103 ) ) ;
#62459 = CARTESIAN_POINT ( 'NONE',  ( 7.829418448290626387, -278.8009198773373782, -209.4692856207271063 ) ) ;
#62460 = VECTOR ( 'NONE', #59286, 999.9999999999998863 ) ;
#62461 = CARTESIAN_POINT ( 'NONE',  ( -32.35539466067025671, -287.4289301519967239, -194.0038480387398749 ) ) ;
#62462 = CARTESIAN_POINT ( 'NONE',  ( 24.23720895448933632, -287.9275498323750071, -309.5661936832856895 ) ) ;
#62463 = AXIS2_PLACEMENT_3D ( 'NONE', #59519, #8822, #45261 ) ;
#62464 = CARTESIAN_POINT ( 'NONE',  ( -111.0452528469028124, -280.1043867483486451, -267.9042783526909943 ) ) ;
#62465 = CARTESIAN_POINT ( 'NONE',  ( -102.9241848702152282, -294.0964316652198249, -306.0091823762008403 ) ) ;
#62466 = CARTESIAN_POINT ( 'NONE',  ( -97.21513662511344478, -297.7114223709497765, -313.8930348137300257 ) ) ;
#62467 = CARTESIAN_POINT ( 'NONE',  ( -95.59749364166030716, -276.7223577774606724, -315.0085482345307355 ) ) ;
#62468 = VERTEX_POINT ( 'NONE', #33970 ) ;
#62469 = CARTESIAN_POINT ( 'NONE',  ( 53.56078642086819031, -298.8278332737911001, -193.3871885607800323 ) ) ;
#62470 = CARTESIAN_POINT ( 'NONE',  ( -59.08687513482454534, -291.2557567528447748, -341.6080858073236186 ) ) ;
#62471 = CARTESIAN_POINT ( 'NONE',  ( 18.81219702445331166, -294.4441009831222118, -218.8520872178545744 ) ) ;
#62472 = CARTESIAN_POINT ( 'NONE',  ( 201.9720043525299218, 292.2277401595099491, -53.99999999997594102 ) ) ;
#62473 = CIRCLE ( 'NONE', #70035, 22.83127060016883192 ) ;
#62474 = CARTESIAN_POINT ( 'NONE',  ( -23.75810946330653906, -289.5255355364519687, -342.2417055962533823 ) ) ;
#62475 = CARTESIAN_POINT ( 'NONE',  ( -48.18343439339133027, -253.7899642232936515, -458.8318842538573676 ) ) ;
#62476 = EDGE_CURVE ( 'NONE', #84950, #27314, #58519, .T. ) ;
#62477 = CARTESIAN_POINT ( 'NONE',  ( -112.5037681141233037, -297.0000969593267541, -286.6084661711859667 ) ) ;
#62478 = CARTESIAN_POINT ( 'NONE',  ( -112.7746364397447110, -288.7886372312765957, -262.7373097285047834 ) ) ;
#62479 = CARTESIAN_POINT ( 'NONE',  ( -31.91564562775961633, -298.4516268701335093, -193.3819643928579524 ) ) ;
#62480 = LINE ( 'NONE', #47289, #48800 ) ;
#62481 = VECTOR ( 'NONE', #53427, 1000.000000000000000 ) ;
#62482 = CARTESIAN_POINT ( 'NONE',  ( 195.6954295768035479, 25.61923908820089224, 14.35989702634663345 ) ) ;
#62483 = CARTESIAN_POINT ( 'NONE',  ( -8.477295177102565304, -290.2012511749268810, -341.0120317553232212 ) ) ;
#62484 = CARTESIAN_POINT ( 'NONE',  ( -117.3417001280813707, -275.0519495502701943, -270.3929463913696054 ) ) ;
#62485 = CARTESIAN_POINT ( 'NONE',  ( 23.31738787103862975, -281.5332207163203293, -317.6453586990783720 ) ) ;
#62486 = CARTESIAN_POINT ( 'NONE',  ( -78.06764539347322795, -287.5039227357324876, -207.5188477820374260 ) ) ;
#62487 = CARTESIAN_POINT ( 'NONE',  ( -33.73682970312665219, -284.6714157335118216, -194.0354263511844977 ) ) ;
#62488 = CARTESIAN_POINT ( 'NONE',  ( -62.62575788680646838, -271.7221775669246995, -199.9285626617074172 ) ) ;
#62489 = CARTESIAN_POINT ( 'NONE',  ( -31.24569009509668049, -276.0498759169886966, -196.1582407838954794 ) ) ;
#62490 = CARTESIAN_POINT ( 'NONE',  ( -93.51414036032699073, -287.9483848098208796, -319.2845846413326854 ) ) ;
#62491 = CARTESIAN_POINT ( 'NONE',  ( -96.08147876313722691, -279.7596982539052419, -318.2347852238114001 ) ) ;
#62492 = AXIS2_PLACEMENT_3D ( 'NONE', #56405, #35561, #87120 ) ;
#62493 = ORIENTED_EDGE ( 'NONE', *, *, #13958, .F. ) ;
#62495 = CARTESIAN_POINT ( 'NONE',  ( 35.66730939899011332, -280.9492747752598234, -274.0458426340898654 ) ) ;
#62494 = CARTESIAN_POINT ( 'NONE',  ( -3.149092476846345523, -280.5170641353806786, -205.8499202825576049 ) ) ;
#62496 = CARTESIAN_POINT ( 'NONE',  ( -37.11402287224021990, -278.1289949830828618, -347.0646758699858765 ) ) ;
#62497 = CARTESIAN_POINT ( 'NONE',  ( 38.88137406026387310, -280.4492902885523904, -278.4917145783999217 ) ) ;
#62498 = CARTESIAN_POINT ( 'NONE',  ( 119.9181164563876649, 148.9434379163483015, -261.0995976656233779 ) ) ;
#62499 = CARTESIAN_POINT ( 'NONE',  ( 38.49328721732177883, -276.3429173315491312, -258.3653461316740731 ) ) ;
#62500 = EDGE_CURVE ( 'NONE', #52231, #70265, #36686, .T. ) ;
#62501 = CARTESIAN_POINT ( 'NONE',  ( -110.3792060108426796, -274.3542079634458446, -248.0844052571740690 ) ) ;
#62502 = CARTESIAN_POINT ( 'NONE',  ( -54.42813229853333468, -291.7662352645558599, -345.3683826091709648 ) ) ;
#62503 = ORIENTED_EDGE ( 'NONE', *, *, #25613, .F. ) ;
#62504 = CARTESIAN_POINT ( 'NONE',  ( 175.2296996224750103, 149.6461846693799487, 0.000000000000000000 ) ) ;
#62505 = CARTESIAN_POINT ( 'NONE',  ( 30.77749032570432064, -288.9944198009672505, -297.5905662195247601 ) ) ;
#62506 = CARTESIAN_POINT ( 'NONE',  ( 34.12714280562018843, -289.6443356662788347, -296.3247671150632527 ) ) ;
#62507 = CARTESIAN_POINT ( 'NONE',  ( -110.2249809973208841, -289.8181481158409838, -276.6304047091149414 ) ) ;
#62508 = CARTESIAN_POINT ( 'NONE',  ( -73.57848248213724673, -285.0924594981007658, -202.4314823492213691 ) ) ;
#62509 = CARTESIAN_POINT ( 'NONE',  ( 26.54924896572594406, -23.55631650609774752, -345.1007383875407299 ) ) ;
#62510 = CARTESIAN_POINT ( 'NONE',  ( 35.35864716923569517, -279.7863996783452762, -257.6686036887648470 ) ) ;
#62511 = CARTESIAN_POINT ( 'NONE',  ( 35.19803604602822134, -289.2079317681412363, -254.5860693470918363 ) ) ;
#62512 = CARTESIAN_POINT ( 'NONE',  ( 12.37027135513538312, -280.8245057082112908, -324.7617396909143963 ) ) ;
#62513 = CARTESIAN_POINT ( 'NONE',  ( -83.76210701367267575, -280.7149475510340721, -213.3181424732781863 ) ) ;
#62514 = CARTESIAN_POINT ( 'NONE',  ( -3.833662056930598361, -277.0898906721354820, -335.2856882657222855 ) ) ;
#62515 = CARTESIAN_POINT ( 'NONE',  ( -96.09642893474666892, -288.6820020519545551, -319.5331786034835204 ) ) ;
#62516 = CARTESIAN_POINT ( 'NONE',  ( -114.1793417686187126, -285.3595991801640821, -269.9928149620623685 ) ) ;
#62517 = CARTESIAN_POINT ( 'NONE',  ( -105.7265730229388652, -284.5884055529612624, -305.7340591338137301 ) ) ;
#62518 = CARTESIAN_POINT ( 'NONE',  ( 35.14004538967056845, -281.8388114359333372, -279.4561300441198455 ) ) ;
#62519 = ORIENTED_EDGE ( 'NONE', *, *, #61608, .T. ) ;
#62520 = DIRECTION ( 'NONE',  ( 0.000000000000000000, 0.000000000000000000, 1.000000000000000000 ) ) ;
#62521 = CARTESIAN_POINT ( 'NONE',  ( -99.03918675619182466, -293.0044606163714320, -226.3869707419946451 ) ) ;
#62522 = AXIS2_PLACEMENT_3D ( 'NONE', #93263, #71510, #28417 ) ;
#62523 = CARTESIAN_POINT ( 'NONE',  ( -33.54696690536734849, -290.7838132249228806, -193.9484340011192103 ) ) ;
#62524 = CARTESIAN_POINT ( 'NONE',  ( 35.61374299019288969, -274.5194967565503248, -263.4102978018960926 ) ) ;
#62525 = CARTESIAN_POINT ( 'NONE',  ( -114.1325566424810916, -295.8385838841359146, -275.3245156865346530 ) ) ;
#62526 = CARTESIAN_POINT ( 'NONE',  ( -72.94509993043601526, -290.0515824854518314, -205.7816483703690835 ) ) ;
#62527 = CARTESIAN_POINT ( 'NONE',  ( 2.091012644759666639, -292.7566170396970620, -333.0559432045100152 ) ) ;
#62528 = CIRCLE ( 'NONE', #45864, 0.5000000000000004441 ) ;
#62529 = CARTESIAN_POINT ( 'NONE',  ( -31.82628276922260824, -290.1862258789201974, -343.6015698292261504 ) ) ;
#62530 = DIRECTION ( 'NONE',  ( 0.000000000000000000, 0.000000000000000000, -1.000000000000000000 ) ) ;
#62531 = AXIS2_PLACEMENT_3D ( 'NONE', #43176, #80081, #64986 ) ;
#62532 = CARTESIAN_POINT ( 'NONE',  ( -79.39749743985044006, -291.6197162172724688, -332.5230426707244078 ) ) ;
#62533 = CARTESIAN_POINT ( 'NONE',  ( -25.28968528822433726, -290.2052931969116116, -196.1669311322207534 ) ) ;
#62534 = CARTESIAN_POINT ( 'NONE',  ( 36.67595890380260215, -295.7086654504139460, -282.5382331042629858 ) ) ;
#62535 = CARTESIAN_POINT ( 'NONE',  ( 19.69089987937389807, -287.8457026778626187, -224.3989954509325457 ) ) ;
#62536 = CARTESIAN_POINT ( 'NONE',  ( 36.80222480147381248, -295.7116295172220362, -282.7967236884273916 ) ) ;
#62537 = AXIS2_PLACEMENT_3D ( 'NONE', #3349, #16175, #37469 ) ;
#62538 = CARTESIAN_POINT ( 'NONE',  ( -2.093673719876190553, -276.4963916838688078, -203.7579390827001191 ) ) ;
#62539 = CARTESIAN_POINT ( 'NONE',  ( 12.43490360822420016, -275.1713669133288249, -328.5873872945156222 ) ) ;
#62540 = CARTESIAN_POINT ( 'NONE',  ( -31.91341839994286289, -297.3156647644431132, -193.5233109628402417 ) ) ;
#62541 = CARTESIAN_POINT ( 'NONE',  ( 10.29943968133824406, -274.6240121980960112, -327.0029382979065531 ) ) ;
#62542 = CARTESIAN_POINT ( 'NONE',  ( -6.144032942095575045, -278.5451416597068715, -202.7600743682178290 ) ) ;
#62543 = CARTESIAN_POINT ( 'NONE',  ( -33.79891809001208713, -299.4125882376109189, -196.8671507568475931 ) ) ;
#62544 = AXIS2_PLACEMENT_3D ( 'NONE', #59752, #81033, #30380 ) ;
#62545 = CARTESIAN_POINT ( 'NONE',  ( -63.76373908956360737, -296.8286521384384855, -339.0973470259114606 ) ) ;
#62546 = CARTESIAN_POINT ( 'NONE',  ( 175.2296996224750103, 140.2072866198470251, 24.00000000000002132 ) ) ;
#62547 = CARTESIAN_POINT ( 'NONE',  ( -100.0404418221979768, -297.8737701061027678, -232.5601944838269048 ) ) ;
#62548 = DIRECTION ( 'NONE',  ( 1.000000000000000000, 4.095251346825558428E-15, 0.000000000000000000 ) ) ;
#62550 = CARTESIAN_POINT ( 'NONE',  ( -105.4154717941531203, -272.7393905257599158, -243.8595651865568925 ) ) ;
#62549 = CARTESIAN_POINT ( 'NONE',  ( 24.48738717028066958, -286.1550089500391891, -313.5270067797571869 ) ) ;
#62551 = AXIS2_PLACEMENT_3D ( 'NONE', #74658, #9782, #39104 ) ;
#62552 = CARTESIAN_POINT ( 'NONE',  ( 28.69854607509536848, -287.0346374543865977, -230.6642725504785574 ) ) ;
#62553 = CARTESIAN_POINT ( 'NONE',  ( -107.7137651166459733, -289.8191206141484599, -301.6934681854449423 ) ) ;
#62554 = CARTESIAN_POINT ( 'NONE',  ( -110.0420831950332854, -298.7880005354153354, -250.3422926058365192 ) ) ;
#62555 = CARTESIAN_POINT ( 'NONE',  ( 35.55568063452456329, -291.7702765593687104, -287.3290290903524919 ) ) ;
#62556 = CARTESIAN_POINT ( 'NONE',  ( 37.82883484982344413, -280.5489738526259771, -254.3748957718820520 ) ) ;
#62557 = CARTESIAN_POINT ( 'NONE',  ( 153.2628468892384603, 20.37991841447902175, -11.93555113919331134 ) ) ;
#62558 = CARTESIAN_POINT ( 'NONE',  ( -48.49081814431468018, -277.9101904052724876, -196.1428057292681615 ) ) ;
#62559 = TOROIDAL_SURFACE ( 'NONE', #71697, 154.4364916446740210, 1.000000000000000000 ) ;
#62560 = CARTESIAN_POINT ( 'NONE',  ( 204.1749232501770450, 287.7883336863533259, -5.086027127806754145 ) ) ;
#62561 = CARTESIAN_POINT ( 'NONE',  ( -23.72648930226850794, -287.6693453420479045, -342.5362998687483014 ) ) ;
#62562 = CARTESIAN_POINT ( 'NONE',  ( 0.000000000000000000, 15.00000000000000000, 9.000000000000001776 ) ) ;
#62563 = CARTESIAN_POINT ( 'NONE',  ( -67.14663747770097757, -287.4425783543860007, -339.2400677067841457 ) ) ;
#62564 = CARTESIAN_POINT ( 'NONE',  ( -84.60261042645456087, -298.9889732991502456, -213.6124007350129546 ) ) ;
#62565 = CARTESIAN_POINT ( 'NONE',  ( 37.57148526252345277, -283.1671408037443030, -285.4150526582834573 ) ) ;
#62567 = CARTESIAN_POINT ( 'NONE',  ( -105.2139348631828568, -284.1909844448757099, -297.3754695694228189 ) ) ;
#62566 = CARTESIAN_POINT ( 'NONE',  ( -112.4289050837386412, -270.7395577891506377, -261.9215771874306711 ) ) ;
#62568 = CARTESIAN_POINT ( 'NONE',  ( 0.9033207881293309205, -275.9986143485042476, -207.4906695028003583 ) ) ;
#62569 = ADVANCED_FACE ( 'NONE', ( #63809 ), #20697, .F. ) ;
#62570 = CARTESIAN_POINT ( 'NONE',  ( 37.53427269006324707, -283.6182716941420381, -275.4978649170241169 ) ) ;
#62571 = CARTESIAN_POINT ( 'NONE',  ( -68.40108027298184368, -272.5546139077140424, -203.9429883882090166 ) ) ;
#62572 = ORIENTED_EDGE ( 'NONE', *, *, #3543, .F. ) ;
#62573 = CARTESIAN_POINT ( 'NONE',  ( 165.2494399300530290, 8.542400036368780647, 13.00000000000000178 ) ) ;
#62574 = CARTESIAN_POINT ( 'NONE',  ( 35.45330800551266748, -293.0672954734139353, -245.1021611932829956 ) ) ;
#62575 = CARTESIAN_POINT ( 'NONE',  ( -111.7329616175136096, -286.4527453021829047, -276.5082323215308406 ) ) ;
#62576 = DIRECTION ( 'NONE',  ( 1.000000000000000000, 0.000000000000000000, 0.000000000000000000 ) ) ;
#62577 = CARTESIAN_POINT ( 'NONE',  ( -111.2869819898779866, -275.6237833571633473, -305.9350535429201159 ) ) ;
#62578 = CARTESIAN_POINT ( 'NONE',  ( -82.45974247071691821, -276.8482542599046496, -332.5585542255541895 ) ) ;
#62579 = CARTESIAN_POINT ( 'NONE',  ( -67.75351038329525011, -287.8445335521758466, -340.2292953879033348 ) ) ;
#62580 = CARTESIAN_POINT ( 'NONE',  ( -104.7396718578417278, -285.6749583615194297, -300.1641573799864773 ) ) ;
#62581 = CARTESIAN_POINT ( 'NONE',  ( -24.12695981134176648, -278.6413819671305987, -343.2373515770221957 ) ) ;
#62582 = CARTESIAN_POINT ( 'NONE',  ( -110.9191536318844555, -285.7171071123252091, -290.9757882353332548 ) ) ;
#62583 = CARTESIAN_POINT ( 'NONE',  ( -91.97079509739259606, -282.6491644875575275, -319.3983216736398276 ) ) ;
#62584 = CARTESIAN_POINT ( 'NONE',  ( -60.37133141458019026, -281.7538362498117408, -198.9296222287348428 ) ) ;
#62585 = CARTESIAN_POINT ( 'NONE',  ( -52.54769881529375652, -274.0293594243011057, -194.8230518923121508 ) ) ;
#62586 = CARTESIAN_POINT ( 'NONE',  ( -14.59171986027598678, -276.5986751120722147, -343.9794226222867337 ) ) ;
#62587 = CARTESIAN_POINT ( 'NONE',  ( -95.89119188554884943, -297.8365671294604340, -316.3314477254314170 ) ) ;
#62588 = DIRECTION ( 'NONE',  ( 1.000000000000000000, 0.000000000000000000, 0.000000000000000000 ) ) ;
#62589 = CARTESIAN_POINT ( 'NONE',  ( 153.4180177809303416, 19.62189878706044865, -10.83803683443614396 ) ) ;
#62590 = CARTESIAN_POINT ( 'NONE',  ( -112.3751245658655051, -294.8264108244034105, -259.7655397737052567 ) ) ;
#62591 = CARTESIAN_POINT ( 'NONE',  ( 33.30009199879525283, -275.3058294070042962, -289.0085212044393757 ) ) ;
#62592 = AXIS2_PLACEMENT_3D ( 'NONE', #9259, #36765, #30590 ) ;
#62593 = CARTESIAN_POINT ( 'NONE',  ( -113.1536202231119432, -273.8998112871589683, -259.0187801401784213 ) ) ;
#62594 = CARTESIAN_POINT ( 'NONE',  ( -9.127565342238625590, -288.1863295667753846, -201.9227462911193243 ) ) ;
#62595 = CARTESIAN_POINT ( 'NONE',  ( 38.53451918419519728, -294.9640340606317750, -261.7844428741461229 ) ) ;
#62596 = CARTESIAN_POINT ( 'NONE',  ( 37.93219107720220507, -294.5786189762277445, -256.1537247561038839 ) ) ;
#62597 = CARTESIAN_POINT ( 'NONE',  ( -87.16824830403565727, -293.3566860744488736, -214.4581739620171561 ) ) ;
#62598 = APPLICATION_CONTEXT ( 'automotive_design' ) ;
#62599 = CARTESIAN_POINT ( 'NONE',  ( -75.41719429619169546, -277.5434202745984749, -205.8788604737563332 ) ) ;
#62600 = VECTOR ( 'NONE', #66728, 1000.000000000000000 ) ;
#62601 = CARTESIAN_POINT ( 'NONE',  ( -111.0511528584513172, -280.6115305763220817, -259.5992293123894683 ) ) ;
#62602 = CARTESIAN_POINT ( 'NONE',  ( -105.2603020961959288, -294.2280418209199979, -300.9565055639724847 ) ) ;
#62603 = CARTESIAN_POINT ( 'NONE',  ( -69.91720982494362602, -285.3369331020471691, -338.7795976412631376 ) ) ;
#62604 = CARTESIAN_POINT ( 'NONE',  ( -79.47575467268617899, -284.3887432512145210, -210.3075770829054534 ) ) ;
#62605 = CARTESIAN_POINT ( 'NONE',  ( 187.0186979179691775, 261.8542818151678944, -152.7852267909635202 ) ) ;
#62606 = ORIENTED_EDGE ( 'NONE', *, *, #31797, .F. ) ;
#62607 = CARTESIAN_POINT ( 'NONE',  ( -59.98115673316993224, -285.4172298914189696, -200.9381931568972846 ) ) ;
#62608 = EDGE_LOOP ( 'NONE', ( #43608, #17052, #8460, #68301 ) ) ;
#62609 = CARTESIAN_POINT ( 'NONE',  ( 38.36492379129992969, -282.7866394139171007, -282.6906722658144417 ) ) ;
#62610 = CIRCLE ( 'NONE', #30834, 4.999999999999990230 ) ;
#62611 = CARTESIAN_POINT ( 'NONE',  ( -94.63194022947706685, -273.5241533536450333, -225.0851212955402332 ) ) ;
#62612 = CARTESIAN_POINT ( 'NONE',  ( 19.99977743061145929, -285.6547891532740095, -219.4894533955281872 ) ) ;
#62613 = CIRCLE ( 'NONE', #35370, 7.500000000000012434 ) ;
#62614 = CARTESIAN_POINT ( 'NONE',  ( -48.09770585449252422, -280.8598901677814865, -194.3000127185015060 ) ) ;
#62615 = SHAPE_REPRESENTATION_RELATIONSHIP ( 'NONE' , 'NONE' ,  #42162, #88142 ) ;
#62616 = CARTESIAN_POINT ( 'NONE',  ( -42.40356559317686447, -281.5095189573240759, -194.2225254615520385 ) ) ;
#62617 = CARTESIAN_POINT ( 'NONE',  ( -31.09032952305880215, -280.7804486691148895, -193.6649509313287751 ) ) ;
#62618 = CARTESIAN_POINT ( 'NONE',  ( 34.45848030099739390, -279.0523547857346784, -270.3937649182068412 ) ) ;
#62619 = CARTESIAN_POINT ( 'NONE',  ( -83.11721010220915673, -220.0893266087223878, -352.5837759202555048 ) ) ;
#62620 = EDGE_LOOP ( 'NONE', ( #13140, #74835, #7065, #1101, #56432, #13355 ) ) ;
#62621 = CARTESIAN_POINT ( 'NONE',  ( -49.19021291046425404, -275.9011149219318213, -196.4192727083408556 ) ) ;
#62622 = CARTESIAN_POINT ( 'NONE',  ( -48.81378135290628251, -154.5565111508429936, -364.8478127054240190 ) ) ;
#62623 = AXIS2_PLACEMENT_3D ( 'NONE', #19422, #27465, #19886 ) ;
#62624 = CARTESIAN_POINT ( 'NONE',  ( -7.315182385718625113, -278.4679806360489920, -202.0078707700635903 ) ) ;
#62625 = CARTESIAN_POINT ( 'NONE',  ( 37.36517219576794702, -295.4891771257205164, -284.3188385113026015 ) ) ;
#62626 = CARTESIAN_POINT ( 'NONE',  ( -80.22126148798015777, -294.9989459526885867, -329.5661505850004573 ) ) ;
#62627 = CARTESIAN_POINT ( 'NONE',  ( -104.5531709379612977, -290.5456401981590489, -232.9158900536068586 ) ) ;
#62628 = DIRECTION ( 'NONE',  ( 0.000000000000000000, 0.000000000000000000, 1.000000000000000000 ) ) ;
#62630 = CARTESIAN_POINT ( 'NONE',  ( 22.65371560706949694, -285.3568532875524397, -227.2983022257669461 ) ) ;
#62629 = CARTESIAN_POINT ( 'NONE',  ( -95.14772181160688547, -294.4466649134712384, -320.3318109051483589 ) ) ;
#62631 = CARTESIAN_POINT ( 'NONE',  ( 11.11541274538510216, -296.2331216507247404, -326.5996607234354769 ) ) ;
#62632 = CARTESIAN_POINT ( 'NONE',  ( -98.52684749151755739, -286.4286993546303961, -229.6472233002308769 ) ) ;
#62633 = ORIENTED_EDGE ( 'NONE', *, *, #78401, .T. ) ;
#62634 = CARTESIAN_POINT ( 'NONE',  ( -19.45327542267640908, -293.2179284200299776, -195.6551127116425448 ) ) ;
#62635 = CARTESIAN_POINT ( 'NONE',  ( 17.65531220614429486, -282.7301594279460915, -318.4580729391352634 ) ) ;
#62636 = CARTESIAN_POINT ( 'NONE',  ( -79.27250989781455814, -294.3995770898573028, -334.4689639136826145 ) ) ;
#62637 = AXIS2_PLACEMENT_3D ( 'NONE', #42045, #78530, #14143 ) ;
#62638 = CARTESIAN_POINT ( 'NONE',  ( -114.2075722186280871, -291.3799484244527775, -268.3691218432566075 ) ) ;
#62639 = EDGE_CURVE ( 'NONE', #10045, #87518, #6024, .T. ) ;
#62640 = CARTESIAN_POINT ( 'NONE',  ( -72.15003753239496120, -292.0965833998297967, -201.7323437223217013 ) ) ;
#62641 = CARTESIAN_POINT ( 'NONE',  ( 30.97384639226432057, -287.3737827200436072, -244.4893441569351182 ) ) ;
#62642 = VERTEX_POINT ( 'NONE', #93574 ) ;
#62643 = DIRECTION ( 'NONE',  ( -0.000000000000000000, 1.000000000000000000, 0.000000000000000000 ) ) ;
#62644 = CARTESIAN_POINT ( 'NONE',  ( -68.99001483723060346, -297.3242864768307072, -339.2134581261443032 ) ) ;
#62645 = CARTESIAN_POINT ( 'NONE',  ( -101.8912794902445569, -295.7787691208724254, -229.2922724131478276 ) ) ;
#62646 = EDGE_CURVE ( 'NONE', #20445, #69103, #42765, .T. ) ;
#62647 = CARTESIAN_POINT ( 'NONE',  ( -54.53644206323097876, -278.8846278663562543, -199.1206287893511444 ) ) ;
#62648 = VERTEX_POINT ( 'NONE', #19751 ) ;
#62649 = CARTESIAN_POINT ( 'NONE',  ( 36.43266955204646962, -275.3345160659930002, -292.2449241545749601 ) ) ;
#62650 = CARTESIAN_POINT ( 'NONE',  ( -73.16716868967206722, -296.0478441130085798, -205.9620220606466034 ) ) ;
#62651 = CARTESIAN_POINT ( 'NONE',  ( -72.21381685430633013, -279.3789402764474517, -335.9101851615010901 ) ) ;
#62652 = CARTESIAN_POINT ( 'NONE',  ( 32.28491054200005550, -273.3541066910371455, -244.6123206241607875 ) ) ;
#62653 = CARTESIAN_POINT ( 'NONE',  ( -80.37524890574610481, -296.8551360638479082, -329.8190374161329146 ) ) ;
#62654 = CARTESIAN_POINT ( 'NONE',  ( -92.98797878370415049, -298.3085114748986939, -222.6163635496660049 ) ) ;
#62655 = DIRECTION ( 'NONE',  ( 0.000000000000000000, 0.000000000000000000, -1.000000000000000000 ) ) ;
#62656 = CARTESIAN_POINT ( 'NONE',  ( -99.34554376769511919, -297.5583388518279548, -314.7440213026769129 ) ) ;
#62657 = CARTESIAN_POINT ( 'NONE',  ( -9.919518414749692425, -296.3945003126609663, -195.2037656782123349 ) ) ;
#62658 = CARTESIAN_POINT ( 'NONE',  ( -89.89535780959727163, -291.9367979451988617, -219.5476775119697095 ) ) ;
#62659 = CARTESIAN_POINT ( 'NONE',  ( -96.25083141440101997, -288.5125514085958116, -314.4853188322464348 ) ) ;
#62660 = CARTESIAN_POINT ( 'NONE',  ( 208.4306832106270804, -148.7221692137691491, 0.000000000000000000 ) ) ;
#62661 = CARTESIAN_POINT ( 'NONE',  ( 37.53343359844520677, -276.2666722501370486, -288.1165084887675221 ) ) ;
#62662 = CARTESIAN_POINT ( 'NONE',  ( -79.74377151227155025, -297.7942008654942470, -210.9123852036024687 ) ) ;
#62663 = CARTESIAN_POINT ( 'NONE',  ( -47.91351124033828768, -281.8983630975148458, -195.6984784909776067 ) ) ;
#62664 = CARTESIAN_POINT ( 'NONE',  ( 30.29373307774961788, -279.7709726107038932, -234.4885631716222179 ) ) ;
#62665 = PRODUCT_RELATED_PRODUCT_CATEGORY ( 'part', '', ( #20991 ) ) ;
#62666 = CARTESIAN_POINT ( 'NONE',  ( -98.72707103111632421, -277.2828936139156895, -316.6984857735657215 ) ) ;
#62667 = CARTESIAN_POINT ( 'NONE',  ( -42.95548625142242827, -282.3218397372677373, -343.3570973513015474 ) ) ;
#62668 = CARTESIAN_POINT ( 'NONE',  ( 35.55955866712312741, -279.3172539801713583, -252.0462361592038576 ) ) ;
#62669 = CARTESIAN_POINT ( 'NONE',  ( 21.16092167436010740, -273.5039061060537620, -225.6993780569914350 ) ) ;
#62670 = CARTESIAN_POINT ( 'NONE',  ( -33.64081299148737259, -279.0057597512598022, -345.2824594583906332 ) ) ;
#62671 = DIRECTION ( 'NONE',  ( 0.000000000000000000, 0.000000000000000000, -1.000000000000000000 ) ) ;
#62672 = FACE_OUTER_BOUND ( 'NONE', #63806, .T. ) ;
#62673 = CARTESIAN_POINT ( 'NONE',  ( -36.53121673348384491, -296.3020323788277324, -194.3746836460879592 ) ) ;
#62674 = AXIS2_PLACEMENT_3D ( 'NONE', #66941, #51323, #88700 ) ;
#62675 = CARTESIAN_POINT ( 'NONE',  ( 35.81363602509566135, -277.7742414619397664, -287.6887341515205776 ) ) ;
#62676 = CARTESIAN_POINT ( 'NONE',  ( -77.61735700266031301, -271.5113161136116560, -207.0928628242538991 ) ) ;
#62677 = CARTESIAN_POINT ( 'NONE',  ( 209.8744251295252354, 28.03846817292548366, 10.50000000000000000 ) ) ;
#62678 = CARTESIAN_POINT ( 'NONE',  ( -112.4694489270531790, -286.3694479938332620, -278.4317782485246653 ) ) ;
#62679 = CIRCLE ( 'NONE', #70244, 0.9999999999999977796 ) ;
#62680 = CARTESIAN_POINT ( 'NONE',  ( 208.3418117619748102, 38.42745601219717599, 14.33494424848941406 ) ) ;
#62681 = CARTESIAN_POINT ( 'NONE',  ( 36.93778946276158592, -285.6898161624158661, -281.0953053140264615 ) ) ;
#62682 =( BOUNDED_SURFACE ( )  B_SPLINE_SURFACE ( 3, 2, ( 
 ( #23013, #16847, #2652 ),
 ( #23496, #800, #16386 ),
 ( #74141, #44325, #52819 ),
 ( #51892, #29680, #22551 ),
 ( #52364, #15454, #2188 ),
 ( #79858, #87404, #51425 ) ),
 .UNSPECIFIED., .F., .F., .F. ) 
 B_SPLINE_SURFACE_WITH_KNOTS ( ( 4, 2, 4 ),
 ( 3, 3 ),
 ( 3.871320309816757010, 4.291854645100723786, 4.712388980384689674 ),
 ( 0.000000000000000000, 1.000000000000000000 ),
 .UNSPECIFIED. ) 
 GEOMETRIC_REPRESENTATION_ITEM ( )  RATIONAL_B_SPLINE_SURFACE ( (
 ( 1.000000000000000000, 0.7827533893364934103, 1.000000000000000000),
 ( 1.000000000000000000, 0.7737378266060769283, 1.000000000000000000),
 ( 1.000000000000000000, 0.7623946665110049592, 1.000000000000000000),
 ( 1.000000000000000000, 0.7365781863221951831, 1.000000000000000000),
 ( 1.000000000000000000, 0.7221049971011784807, 1.000000000000000000),
 ( 1.000000000000000000, 0.7071067811865479058, 1.000000000000000000) ) ) 
 REPRESENTATION_ITEM ( '' )  SURFACE ( )  );
#62683 = DIRECTION ( 'NONE',  ( 0.8660254037844359321, 0.5000000000000046629, -0.000000000000000000 ) ) ;
#62684 = CARTESIAN_POINT ( 'NONE',  ( -41.07468136076666809, -293.8950627699028928, -343.6758364479319425 ) ) ;
#62685 = CARTESIAN_POINT ( 'NONE',  ( 27.45694720369125008, -285.2033015570177668, -234.0343339559310607 ) ) ;
#62686 = CARTESIAN_POINT ( 'NONE',  ( 156.3051094419662945, 18.69637893469953838, -10.18000837680961723 ) ) ;
#62687 = CARTESIAN_POINT ( 'NONE',  ( 24.56995022601385870, -292.1264055027472750, -312.7833029782705694 ) ) ;
#62688 = CARTESIAN_POINT ( 'NONE',  ( -35.14859000133749589, -284.5590708853400201, -194.0729462703540946 ) ) ;
#62689 = CARTESIAN_POINT ( 'NONE',  ( -109.9225461035518236, -280.3266001598420303, -257.0021803742650945 ) ) ;
#62690 = CARTESIAN_POINT ( 'NONE',  ( 31.06030618894929063, -288.3111701923981514, -235.8767120970426845 ) ) ;
#62691 = CARTESIAN_POINT ( 'NONE',  ( 31.46516030874382253, -280.2118006691208052, -302.7276789914651545 ) ) ;
#62692 = CARTESIAN_POINT ( 'NONE',  ( -73.54496383499513001, -289.5469024689942330, -333.7657786667729738 ) ) ;
#62694 =( BOUNDED_SURFACE ( )  B_SPLINE_SURFACE ( 3, 2, ( 
 ( #4664, #18885, #62929 ),
 ( #78518, #91763, #76638 ),
 ( #92700, #77103, #83725 ),
 ( #48674, #26451, #70491 ),
 ( #27870, #70948, #84191 ),
 ( #6080, #11763, #34954 ),
 ( #63866, #12234, #26915 ),
 ( #47740, #56763, #78056 ),
 ( #41081, #55340, #40615 ),
 ( #13655, #70005, #6551 ),
 ( #55802, #13198, #77575 ),
 ( #42034, #35430, #33537 ),
 ( #69531, #20289, #56275 ),
 ( #5619, #19806, #34494 ),
 ( #90803, #84654, #19339 ),
 ( #85604, #62442, #20751 ) ),
 .UNSPECIFIED., .F., .F., .F. ) 
 B_SPLINE_SURFACE_WITH_KNOTS ( ( 4, 2, 2, 2, 2, 2, 2, 4 ),
 ( 3, 3 ),
 ( -6.938893903907228378E-18, 0.0006169105258908286335, 0.001233821051781664206, 0.001850731577672499670, 0.002467642103563335351, 0.003084552629454171031, 0.003701463155345006278, 0.004935284207126677640 ),
 ( 0.000000000000000000, 1.000000000000000000 ),
 .UNSPECIFIED. ) 
 GEOMETRIC_REPRESENTATION_ITEM ( )  RATIONAL_B_SPLINE_SURFACE ( (
 ( 1.000000000000000000, 0.8966167345234229424, 1.000000000000000000),
 ( 1.000000000000000000, 0.9004139148586555175, 1.000000000000000000),
 ( 1.000000000000000000, 0.9032061010818291935, 1.000000000000000000),
 ( 1.000000000000000000, 0.9067734849417629084, 1.000000000000000000),
 ( 1.000000000000000000, 0.9075308745986051528, 1.000000000000000000),
 ( 1.000000000000000000, 0.9069696504590781805, 1.000000000000000000),
 ( 1.000000000000000000, 0.9056888044683030214, 1.000000000000000000),
 ( 1.000000000000000000, 0.9012558131641384973, 1.000000000000000000),
 ( 1.000000000000000000, 0.8981641526222049476, 1.000000000000000000),
 ( 1.000000000000000000, 0.8905754533014459406, 1.000000000000000000),
 ( 1.000000000000000000, 0.8860218362703521366, 1.000000000000000000),
 ( 1.000000000000000000, 0.8759703649549664961, 1.000000000000000000),
 ( 1.000000000000000000, 0.8704567387598657335, 1.000000000000000000),
 ( 1.000000000000000000, 0.8526573370808110397, 1.000000000000000000),
 ( 1.000000000000000000, 0.8394012181876917555, 1.000000000000000000),
 ( 1.000000000000000000, 0.8255171224912107864, 1.000000000000000000) ) ) 
 REPRESENTATION_ITEM ( '' )  SURFACE ( )  );
#62693 = AXIS2_PLACEMENT_3D ( 'NONE', #29240, #20738, #28316 ) ;
#62695 = AXIS2_PLACEMENT_3D ( 'NONE', #16141, #59716, #29427 ) ;
#62696 = CARTESIAN_POINT ( 'NONE',  ( -57.29023269278543751, -281.2149060249485615, -199.5272915704423156 ) ) ;
#62697 = CARTESIAN_POINT ( 'NONE',  ( -54.54064568547437375, -280.6284318222396337, -199.1976369487024385 ) ) ;
#62698 = CARTESIAN_POINT ( 'NONE',  ( 27.50150523380058587, -290.0430886122621246, -308.7507717873627939 ) ) ;
#62699 = ORIENTED_EDGE ( 'NONE', *, *, #45671, .T. ) ;
#62700 = CARTESIAN_POINT ( 'NONE',  ( -13.06248678323646573, -274.3591155245477466, -197.2891000868189053 ) ) ;
#62701 = CARTESIAN_POINT ( 'NONE',  ( -111.2479949310128262, -292.3957408418274326, -280.9266832379707921 ) ) ;
#62702 = DIRECTION ( 'NONE',  ( -0.000000000000000000, -1.000000000000000000, -0.000000000000000000 ) ) ;
#62703 = CARTESIAN_POINT ( 'NONE',  ( -111.2869819898779866, -299.4805209788416391, -234.7871824221999191 ) ) ;
#62704 = ORIENTED_EDGE ( 'NONE', *, *, #40665, .T. ) ;
#62705 = CARTESIAN_POINT ( 'NONE',  ( -18.97273904071714057, -272.2877638656696035, -197.4197426308134595 ) ) ;
#62706 = CARTESIAN_POINT ( 'NONE',  ( 170.7304434856092143, 249.5000000000000568, -24.91818181818180733 ) ) ;
#62707 = CARTESIAN_POINT ( 'NONE',  ( -83.71466702864759668, -294.0761168756562824, -330.8924283418914456 ) ) ;
#62708 = CARTESIAN_POINT ( 'NONE',  ( -55.30272947268393580, -297.3225784875120894, -199.4893472628256461 ) ) ;
#62709 = CARTESIAN_POINT ( 'NONE',  ( 34.38029981252815759, -289.2935358471168001, -287.2922277852051138 ) ) ;
#62710 = AXIS2_PLACEMENT_3D ( 'NONE', #3874, #48812, #12371 ) ;
#62711 = CARTESIAN_POINT ( 'NONE',  ( 3.974218134601690711, -284.2478213355571484, -331.8313396177780987 ) ) ;
#62712 = CARTESIAN_POINT ( 'NONE',  ( -93.14993036369341439, -291.2594594860639745, -322.6297629567361014 ) ) ;
#62713 = CARTESIAN_POINT ( 'NONE',  ( -113.7579194640037059, -291.8204649465798184, -274.0839789721583770 ) ) ;
#62714 = CARTESIAN_POINT ( 'NONE',  ( -80.47989825371161032, -287.4680793517698021, -208.9451122559017904 ) ) ;
#62715 = CARTESIAN_POINT ( 'NONE',  ( -88.93301792798932581, -279.5172365102952767, -213.2005027640632306 ) ) ;
#62716 = CARTESIAN_POINT ( 'NONE',  ( -110.5790831249054520, -294.3943480175670402, -289.0037384466583035 ) ) ;
#62717 = CARTESIAN_POINT ( 'NONE',  ( -81.56329177113407525, -283.4686931348633152, -333.4612994687695391 ) ) ;
#62718 = CARTESIAN_POINT ( 'NONE',  ( 23.49143409190629939, -277.9970424886916476, -312.9957969183646469 ) ) ;
#62719 = CARTESIAN_POINT ( 'NONE',  ( -107.3417001280813565, -275.0519495502701943, -270.3929463913696054 ) ) ;
#62720 = CARTESIAN_POINT ( 'NONE',  ( 19.10917282090019143, -274.4918965704873131, -321.2458266666068880 ) ) ;
#62721 = DIRECTION ( 'NONE',  ( 0.000000000000000000, 0.000000000000000000, 1.000000000000000000 ) ) ;
#62722 = CARTESIAN_POINT ( 'NONE',  ( 9.320655171656451188, -280.2209639846767004, -214.0758333842832144 ) ) ;
#62723 = CARTESIAN_POINT ( 'NONE',  ( -77.59313309167708894, -278.7843671105878229, -335.5981379391097335 ) ) ;
#62724 = CARTESIAN_POINT ( 'NONE',  ( -108.8050327343470087, -283.9689681205925922, -242.1842718366530676 ) ) ;
#62725 = CARTESIAN_POINT ( 'NONE',  ( -68.24444091488061304, -293.4007669457184875, -203.0939779160814851 ) ) ;
#62726 = CARTESIAN_POINT ( 'NONE',  ( 34.96430544092648773, -276.8444801812556761, -246.1474319583253418 ) ) ;
#62727 = CARTESIAN_POINT ( 'NONE',  ( -63.40493579939095525, -275.0346729481839247, -198.4305541125026195 ) ) ;
#62728 = DIRECTION ( 'NONE',  ( 0.000000000000000000, 0.000000000000000000, 1.000000000000000000 ) ) ;
#62729 = CARTESIAN_POINT ( 'NONE',  ( 33.24165078580307409, -275.6314439061106896, -288.9888010991709280 ) ) ;
#62730 = CARTESIAN_POINT ( 'NONE',  ( -72.97569013081923117, -297.5255909534118359, -336.1803567255897178 ) ) ;
#62731 = CARTESIAN_POINT ( 'NONE',  ( -75.63696003311819993, -283.5396852724134646, -206.0688051045194413 ) ) ;
#62732 = CARTESIAN_POINT ( 'NONE',  ( 36.26800391072323038, -292.9359667235247002, -247.8365588781600763 ) ) ;
#62733 = CARTESIAN_POINT ( 'NONE',  ( 21.29930785552477346, -274.2096568668476380, -316.5669624958304667 ) ) ;
#62734 = CARTESIAN_POINT ( 'NONE',  ( 36.93519571926441358, -288.9366319340879272, -253.2920122128685136 ) ) ;
#62735 = CARTESIAN_POINT ( 'NONE',  ( 35.14149622896399450, -292.6209535354996092, -281.6641588051585927 ) ) ;
#62736 = EDGE_LOOP ( 'NONE', ( #84262, #1766, #59810, #49462 ) ) ;
#62737 = CARTESIAN_POINT ( 'NONE',  ( 22.65678290153533325, -291.4889667470666268, -223.0243669818048886 ) ) ;
#62738 = CARTESIAN_POINT ( 'NONE',  ( -108.9603028792401602, -290.0301916667252726, -284.6680987808184682 ) ) ;
#62739 = ORIENTED_EDGE ( 'NONE', *, *, #25508, .F. ) ;
#62740 = CARTESIAN_POINT ( 'NONE',  ( 16.07399888556184919, -287.8682476288912540, -215.3315295040999615 ) ) ;
#62741 = CARTESIAN_POINT ( 'NONE',  ( -107.2485864805327509, -279.1646796863290092, -249.2633757501773175 ) ) ;
#62742 = CARTESIAN_POINT ( 'NONE',  ( -97.17494649910651106, -294.8269232195877407, -318.3555977338385787 ) ) ;
#62743 = CARTESIAN_POINT ( 'NONE',  ( -111.6249229510898573, -285.4551051145208476, -250.2783564824773066 ) ) ;
#62744 = CARTESIAN_POINT ( 'NONE',  ( -110.6641110825146797, -284.5901271072877421, -293.8474538485443190 ) ) ;
#62745 = CARTESIAN_POINT ( 'NONE',  ( 31.37593805074868314, -282.2160350820819872, -295.2082902698688827 ) ) ;
#62746 = CARTESIAN_POINT ( 'NONE',  ( -31.25978362021906420, -124.2753969880052836, -364.3350065174659562 ) ) ;
#62747 = CARTESIAN_POINT ( 'NONE',  ( -104.9959759434921978, -254.8895421021158825, -325.9787696571796687 ) ) ;
#62748 = CARTESIAN_POINT ( 'NONE',  ( 195.4265002117133463, 282.6816008209588631, -110.3567886302177499 ) ) ;
#62749 = CARTESIAN_POINT ( 'NONE',  ( 35.74888117987044467, -274.6937516812146214, -266.1398222809258414 ) ) ;
#62750 = CARTESIAN_POINT ( 'NONE',  ( 33.88359738285667788, -274.7011203020184666, -287.7685829641801547 ) ) ;
#62751 = CARTESIAN_POINT ( 'NONE',  ( -114.2763662760873586, -296.0693713248206222, -269.5968878146475731 ) ) ;
#62752 = CARTESIAN_POINT ( 'NONE',  ( 202.3167528527534955, 289.8673209260633712, -82.47206762618345977 ) ) ;
#62753 = CARTESIAN_POINT ( 'NONE',  ( 33.71994285826205129, -274.6005483994430847, -298.8506728662013643 ) ) ;
#62754 = CARTESIAN_POINT ( 'NONE',  ( -106.3693248146888521, -274.6659015276296145, -243.5145553628732102 ) ) ;
#62755 = ORIENTED_EDGE ( 'NONE', *, *, #82892, .F. ) ;
#62756 = CARTESIAN_POINT ( 'NONE',  ( -57.34001031339916210, -298.7415740595552052, -196.1919871017267951 ) ) ;
#62757 = CARTESIAN_POINT ( 'NONE',  ( 32.37422570182891945, -288.3359240842070790, -292.3853954988765622 ) ) ;
#62758 = CARTESIAN_POINT ( 'NONE',  ( -105.8091646611200360, -296.9035871611078505, -305.3547210544289214 ) ) ;
#62759 = CARTESIAN_POINT ( 'NONE',  ( -97.30233451235987729, -297.6911090821166113, -222.1506499510646506 ) ) ;
#62760 = CARTESIAN_POINT ( 'NONE',  ( -14.84841750065774768, -292.5185435159973508, -200.9129197256225723 ) ) ;
#62761 = ORIENTED_EDGE ( 'NONE', *, *, #51451, .F. ) ;
#62762 = AXIS2_PLACEMENT_3D ( 'NONE', #51581, #16088, #8956 ) ;
#62763 = CARTESIAN_POINT ( 'NONE',  ( 36.19617741455193993, -277.6942479999422062, -287.7805319183706843 ) ) ;
#62764 = ORIENTED_EDGE ( 'NONE', *, *, #2175, .F. ) ;
#62765 = CARTESIAN_POINT ( 'NONE',  ( 39.35086845197975691, -280.9828769092899847, -264.2148322999018433 ) ) ;
#62766 = UNCERTAINTY_MEASURE_WITH_UNIT (LENGTH_MEASURE( 1.000000000000000082E-05 ), #61663, 'distance_accuracy_value', 'NONE');
#62767 = CARTESIAN_POINT ( 'NONE',  ( -70.54881181584757144, -278.4425051179617867, -335.6351264557151808 ) ) ;
#62768 = CARTESIAN_POINT ( 'NONE',  ( 5.321112988311692327, -278.2435700739887920, -333.2408316342586545 ) ) ;
#62769 = CARTESIAN_POINT ( 'NONE',  ( -110.2427694978118922, -276.3277043791433130, -289.4864999557813690 ) ) ;
#62770 = CARTESIAN_POINT ( 'NONE',  ( -108.8806052080202988, -297.4024165208856516, -255.2650157287278319 ) ) ;
#62771 = CARTESIAN_POINT ( 'NONE',  ( -105.5145319565518349, -294.7586711984803287, -298.0710424915932322 ) ) ;
#62772 = CARTESIAN_POINT ( 'NONE',  ( 197.2116943569230045, 249.5000000000000568, -11.92446933126075415 ) ) ;
#62773 = CARTESIAN_POINT ( 'NONE',  ( -35.34391528292362494, -280.5689106807918165, -193.4354714373812953 ) ) ;
#62774 = CARTESIAN_POINT ( 'NONE',  ( -105.5150493298128254, -279.0691350487915088, -244.1159908687126290 ) ) ;
#62775 = CARTESIAN_POINT ( 'NONE',  ( 22.88879431316950885, -286.8718589048248191, -317.5583218750372225 ) ) ;
#62776 = CARTESIAN_POINT ( 'NONE',  ( -54.20913244213483750, -299.8361736911336948, -197.1114207096712221 ) ) ;
#62777 = CARTESIAN_POINT ( 'NONE',  ( 197.4836817735085219, 24.47698789593438917, 11.66666666666666785 ) ) ;
#62778 = CARTESIAN_POINT ( 'NONE',  ( -58.74611564681632103, -288.5332085280372780, -340.3744068218875896 ) ) ;
#62779 = CARTESIAN_POINT ( 'NONE',  ( -77.35104461874557558, -277.7477789645155895, -208.0326559401519830 ) ) ;
#62781 = CARTESIAN_POINT ( 'NONE',  ( -6.682297549938000181, -280.7263384966041713, -338.2080947406936957 ) ) ;
#62780 = CARTESIAN_POINT ( 'NONE',  ( -95.24331146226769818, -277.7623556466783157, -224.9230235373411517 ) ) ;
#62782 = CARTESIAN_POINT ( 'NONE',  ( 31.47966560129664870, -289.1608091326579029, -240.4223764225739899 ) ) ;
#62783 = CARTESIAN_POINT ( 'NONE',  ( -85.75755594294830075, -280.5689940042762487, -215.1974033733533531 ) ) ;
#62784 = CARTESIAN_POINT ( 'NONE',  ( 154.7659666677267580, 19.56018909072084710, -12.94946946941271726 ) ) ;
#62785 = CARTESIAN_POINT ( 'NONE',  ( -85.25542858120036271, -293.3909305001070038, -212.5937928289431227 ) ) ;
#62786 = CARTESIAN_POINT ( 'NONE',  ( -38.55160254141188148, -275.3069930335477693, -346.3381549943728714 ) ) ;
#62787 = CARTESIAN_POINT ( 'NONE',  ( 18.39149936935317342, -276.8752284241597295, -317.6654850352001631 ) ) ;
#62788 = CARTESIAN_POINT ( 'NONE',  ( 35.20864552864138375, -283.2995422316824943, -250.6533828290385486 ) ) ;
#62789 = CARTESIAN_POINT ( 'NONE',  ( 198.7884250876676049, 66.56295291868792674, 9.416620882813951710 ) ) ;
#62790 = CARTESIAN_POINT ( 'NONE',  ( -101.0732837613175406, -291.9289619992819098, -311.0479882234540128 ) ) ;
#62791 = CARTESIAN_POINT ( 'NONE',  ( -70.24715478444055350, -293.4855905774421103, -337.7711784007989877 ) ) ;
#62792 = CARTESIAN_POINT ( 'NONE',  ( -112.2000957169564970, -283.9665355044935495, -253.0296601308724007 ) ) ;
#62793 = DIRECTION ( 'NONE',  ( 1.000000000000000000, 0.000000000000000000, 0.000000000000000000 ) ) ;
#62794 = CARTESIAN_POINT ( 'NONE',  ( -69.69305461488974629, -272.3018110807155949, -204.3714722606277121 ) ) ;
#62795 = CARTESIAN_POINT ( 'NONE',  ( -17.07296494307979273, -290.4560539446659959, -198.8930388139336003 ) ) ;
#62796 = CARTESIAN_POINT ( 'NONE',  ( 164.2231345125756263, 300.2961574867697436, 7.500000000000000000 ) ) ;
#62797 = CARTESIAN_POINT ( 'NONE',  ( -68.03198670781949886, -290.1363786050943645, -200.4840591525245941 ) ) ;
#62798 = CARTESIAN_POINT ( 'NONE',  ( -54.96693575645529961, -287.4220216155817411, -198.6438069025912228 ) ) ;
#62799 = CARTESIAN_POINT ( 'NONE',  ( 26.30144571015113897, -285.2393676315655284, -228.8457714103878402 ) ) ;
#62800 = CARTESIAN_POINT ( 'NONE',  ( -70.26218259763309959, -287.0348579102766848, -204.5320406879389452 ) ) ;
#62801 = CARTESIAN_POINT ( 'NONE',  ( 207.6275970751953537, 36.17632364500597220, 14.41714557868297852 ) ) ;
#62802 = CARTESIAN_POINT ( 'NONE',  ( -77.14547226032442495, -286.3067877318702017, -208.9148378088368645 ) ) ;
#62803 = CARTESIAN_POINT ( 'NONE',  ( -7.857508652533764071, -294.4164281579045905, -200.9995072473832352 ) ) ;
#62804 = CARTESIAN_POINT ( 'NONE',  ( 11.75014631036292911, -274.4564036757578833, -327.8006932644084941 ) ) ;
#62805 = CARTESIAN_POINT ( 'NONE',  ( 38.47054325684204912, -275.7174719157262643, -256.9348643759292941 ) ) ;
#62806 = CARTESIAN_POINT ( 'NONE',  ( 35.32614071337355455, -291.3669729121327236, -249.6088678844010929 ) ) ;
#62807 = CARTESIAN_POINT ( 'NONE',  ( -113.2364877241909937, -278.7147260720351483, -257.3618404741212089 ) ) ;
#62808 = CARTESIAN_POINT ( 'NONE',  ( -38.33954787723131830, -297.0446126150878285, -344.9992523805914857 ) ) ;
#62809 = PLANE ( 'NONE',  #78748 ) ;
#62810 = DIRECTION ( 'NONE',  ( 1.000000000000000000, -0.000000000000000000, 0.000000000000000000 ) ) ;
#62811 = CARTESIAN_POINT ( 'NONE',  ( -70.18790354320688607, -284.2948550937799723, -204.6023442560804142 ) ) ;
#62812 = ADVANCED_FACE ( 'NONE', ( #42929 ), #74532, .T. ) ;
#62813 = CARTESIAN_POINT ( 'NONE',  ( 13.81624004741667555, -278.7687763021331762, -215.4460870757502562 ) ) ;
#62814 = ADVANCED_FACE ( 'NONE', ( #62874 ), #20228, .T. ) ;
#62815 = DIRECTION ( 'NONE',  ( 1.000000000000000000, 0.000000000000000000, 0.000000000000000000 ) ) ;
#62816 = CARTESIAN_POINT ( 'NONE',  ( 39.01341242131886133, -274.0424115457452103, -271.1836658468581049 ) ) ;
#62817 = CARTESIAN_POINT ( 'NONE',  ( -94.53797134275173164, -277.2585268291529133, -315.9056058551217347 ) ) ;
#62818 = CARTESIAN_POINT ( 'NONE',  ( -41.05497484025016774, -296.6198202216361324, -343.9735285365790673 ) ) ;
#62819 = CARTESIAN_POINT ( 'NONE',  ( -25.42999032630619638, -279.1209059799435295, -194.6009458692703902 ) ) ;
#62820 = CARTESIAN_POINT ( 'NONE',  ( 8.384397823678876094, -295.3499996650740513, -327.6323537776866033 ) ) ;
#62821 = CARTESIAN_POINT ( 'NONE',  ( -2.179125175011518589, -295.9116762547243979, -338.3088302090457660 ) ) ;
#62822 = CARTESIAN_POINT ( 'NONE',  ( -93.61221286560099486, -297.0449156233469239, -223.8375931050186409 ) ) ;
#62823 = CARTESIAN_POINT ( 'NONE',  ( -104.2038043571010206, -293.0027907708559951, -236.2687374149244022 ) ) ;
#62824 = CARTESIAN_POINT ( 'NONE',  ( -20.98603584737271532, -286.4231434376322341, -195.1182296114924384 ) ) ;
#62825 = CARTESIAN_POINT ( 'NONE',  ( 21.66387114508282963, -274.3393167556122307, -317.9068664561677906 ) ) ;
#62826 = CARTESIAN_POINT ( 'NONE',  ( -12.22573453462774395, -288.5676737866609187, -343.2056437545292624 ) ) ;
#62827 = CARTESIAN_POINT ( 'NONE',  ( -111.9225191934285988, -280.4921856338110615, -273.4511385940818968 ) ) ;
#62828 = CARTESIAN_POINT ( 'NONE',  ( 32.06740669977688185, -286.3015490078142875, -246.9990903011818659 ) ) ;
#62829 = CARTESIAN_POINT ( 'NONE',  ( -99.99871612781289798, -289.1094240273531568, -229.0478395601604404 ) ) ;
#62830 = CARTESIAN_POINT ( 'NONE',  ( -26.16130516772507875, -127.9538472306148122, -363.7897947155308884 ) ) ;
#62831 = CARTESIAN_POINT ( 'NONE',  ( 0.2056653697569757466, -286.0740381543447484, -207.6269091088429946 ) ) ;
#62832 = CARTESIAN_POINT ( 'NONE',  ( 204.1778867865513405, 300.1383591958309012, -5.086762277128879184 ) ) ;
#62833 = CARTESIAN_POINT ( 'NONE',  ( -44.38564892990635258, -284.0803058584349969, -346.8551583791946769 ) ) ;
#62834 = PRODUCT_DEFINITION_FORMATION_WITH_SPECIFIED_SOURCE ( 'ANY', '', #20991, .NOT_KNOWN. ) ;
#62835 = CARTESIAN_POINT ( 'NONE',  ( -111.4026152547819208, -289.8651708756594303, -250.1171835078003198 ) ) ;
#62836 = CARTESIAN_POINT ( 'NONE',  ( 38.61264438122857712, -283.0750154587286147, -264.2473659342782639 ) ) ;
#62837 = CARTESIAN_POINT ( 'NONE',  ( -11.69057627065549099, -281.6943463124954405, -198.2269445011420714 ) ) ;
#62838 = CARTESIAN_POINT ( 'NONE',  ( 22.58355914970624312, -281.9665356810629078, -312.0500050509663197 ) ) ;
#62839 = CARTESIAN_POINT ( 'NONE',  ( -5.707960850863856628, -276.4682931829216272, -202.3588592535764406 ) ) ;
#62840 = CARTESIAN_POINT ( 'NONE',  ( -53.28924607200669072, -295.2510921782077276, -345.7461050271429599 ) ) ;
#62841 = CARTESIAN_POINT ( 'NONE',  ( -109.3184322967126860, -288.3144670917659482, -290.3305333247381554 ) ) ;
#62842 = AXIS2_PLACEMENT_3D ( 'NONE', #39718, #47771, #12272 ) ;
#62843 = CARTESIAN_POINT ( 'NONE',  ( -57.97868720783193908, -296.6995173421065601, -200.0166737305509912 ) ) ;
#62844 = ORIENTED_EDGE ( 'NONE', *, *, #83939, .F. ) ;
#62845 = CARTESIAN_POINT ( 'NONE',  ( -110.1229130787474730, -286.2693629044856607, -286.0487638383943931 ) ) ;
#62846 = CARTESIAN_POINT ( 'NONE',  ( -36.39604677438176594, -293.1434138434801184, -193.6630793353920694 ) ) ;
#62847 = CARTESIAN_POINT ( 'NONE',  ( 21.89940733642946569, -282.8021244053456371, -313.2122613418093238 ) ) ;
#62848 = CARTESIAN_POINT ( 'NONE',  ( 4.744212798486212357, -273.6639007324630484, -206.0983854134546505 ) ) ;
#62849 = CARTESIAN_POINT ( 'NONE',  ( -98.27258978801756939, -291.8305918761275279, -223.4277683630740512 ) ) ;
#62850 = CARTESIAN_POINT ( 'NONE',  ( -111.9253693218802965, -282.5186955458379998, -283.9756500099579739 ) ) ;
#62851 = CARTESIAN_POINT ( 'NONE',  ( -19.39582449095343009, -292.6100554395524114, -195.4485141377206787 ) ) ;
#62852 = CARTESIAN_POINT ( 'NONE',  ( 35.01650413628489389, -287.7510985722426540, -260.1747298294476423 ) ) ;
#62853 = CARTESIAN_POINT ( 'NONE',  ( 197.9737958995921190, 68.21405198623872934, 9.113933396921945373 ) ) ;
#62854 = CARTESIAN_POINT ( 'NONE',  ( -113.5000000000000568, -192.7866584945343504, -490.8867980474134356 ) ) ;
#62855 = CARTESIAN_POINT ( 'NONE',  ( -12.30567835471983251, -92.54755969097151080, -356.2634384826176301 ) ) ;
#62856 = CARTESIAN_POINT ( 'NONE',  ( 4.184766045387054767, -284.0238960492750948, -334.4412343949247770 ) ) ;
#62857 = CARTESIAN_POINT ( 'NONE',  ( 31.98288692825983404, -290.6237833571634042, -237.0123917617631264 ) ) ;
#62858 = ORIENTED_EDGE ( 'NONE', *, *, #83602, .T. ) ;
#62859 = CARTESIAN_POINT ( 'NONE',  ( 33.61926898762357752, -280.7150310081751172, -288.8167052985417627 ) ) ;
#62860 = CARTESIAN_POINT ( 'NONE',  ( -69.01055622719624694, -277.1240449524029827, -340.5383856355435341 ) ) ;
#62861 = CARTESIAN_POINT ( 'NONE',  ( -30.10994822484974875, -282.1438988381503918, -195.8264118833148189 ) ) ;
#62862 = CARTESIAN_POINT ( 'NONE',  ( -53.92001451859699301, -170.5180466806795323, -362.3035249365248660 ) ) ;
#62863 = CARTESIAN_POINT ( 'NONE',  ( -14.38733816761156703, -278.9186603131959146, -197.4242062396855601 ) ) ;
#62864 = CARTESIAN_POINT ( 'NONE',  ( -111.6287668534059065, -282.6729816095882484, -262.5535001505285777 ) ) ;
#62865 = CARTESIAN_POINT ( 'NONE',  ( -111.8579010354192462, -274.5902383679150489, -256.3823256773028447 ) ) ;
#62866 = CARTESIAN_POINT ( 'NONE',  ( 29.54891209043159961, -294.4395243840719445, -299.7487759107259535 ) ) ;
#62867 = ORIENTED_EDGE ( 'NONE', *, *, #34695, .T. ) ;
#62868 = CARTESIAN_POINT ( 'NONE',  ( -92.91852436723902997, -289.9176272215531753, -222.2730728309688573 ) ) ;
#62869 = CARTESIAN_POINT ( 'NONE',  ( 37.80783614613704913, -276.4085221086491515, -286.7278832686163241 ) ) ;
#62870 = CARTESIAN_POINT ( 'NONE',  ( -89.24217123920264783, -273.2962396433483150, -219.0255445617472105 ) ) ;
#62871 = ORIENTED_EDGE ( 'NONE', *, *, #75705, .F. ) ;
#62872 = CARTESIAN_POINT ( 'NONE',  ( -36.92753951724665740, -272.9775901728838789, -193.6583469963941013 ) ) ;
#62873 = DIRECTION ( 'NONE',  ( 1.000000000000000000, -0.000000000000000000, -0.000000000000000000 ) ) ;
#62874 = FACE_OUTER_BOUND ( 'NONE', #52783, .T. ) ;
#62875 = CARTESIAN_POINT ( 'NONE',  ( -33.46619183329740821, -284.0819322068512065, -343.5803452570306149 ) ) ;
#62876 = CARTESIAN_POINT ( 'NONE',  ( 6.360771649835185393, -284.2281038567240898, -332.5871013470535900 ) ) ;
#62877 = CARTESIAN_POINT ( 'NONE',  ( -109.4224865770883923, -283.7821404709110311, -257.3380776408615134 ) ) ;
#62878 = CARTESIAN_POINT ( 'NONE',  ( 22.13790592575305993, -273.3465870296930689, -226.6733979653421898 ) ) ;
#62879 = CARTESIAN_POINT ( 'NONE',  ( 31.15220526329482453, -283.0349479325320772, -241.7350738599390070 ) ) ;
#62880 = CARTESIAN_POINT ( 'NONE',  ( 35.05825435652167243, -273.8523995244961498, -256.6150514733861314 ) ) ;
#62881 = CARTESIAN_POINT ( 'NONE',  ( 154.2407877675970269, 20.33090418404277955, 11.64082518123277943 ) ) ;
#62882 = CARTESIAN_POINT ( 'NONE',  ( 33.89014266350144311, -276.8601136540028165, -287.7417820347186534 ) ) ;
#62883 = FACE_OUTER_BOUND ( 'NONE', #31414, .T. ) ;
#62884 = CARTESIAN_POINT ( 'NONE',  ( -111.6686336327715026, -279.1099792667473025, -289.8978050649414513 ) ) ;
#62885 = ORIENTED_EDGE ( 'NONE', *, *, #19944, .F. ) ;
#62886 = CARTESIAN_POINT ( 'NONE',  ( 175.2296996224750103, 247.0000000000001137, -9.550761578869391144 ) ) ;
#62887 = CARTESIAN_POINT ( 'NONE',  ( -112.9736449498444273, -286.3452761073405100, -275.6554550595270712 ) ) ;
#62888 = CARTESIAN_POINT ( 'NONE',  ( -38.35476239077845406, -294.2623382046859319, -343.5155808153809858 ) ) ;
#62889 = CARTESIAN_POINT ( 'NONE',  ( -31.84236128172311098, -288.3331975713170436, -347.1147782188801330 ) ) ;
#62890 = CARTESIAN_POINT ( 'NONE',  ( -9.086074484738658086, -284.6666156356701549, -201.9398650835979367 ) ) ;
#62892 = CARTESIAN_POINT ( 'NONE',  ( -89.38937110670140385, -288.0374358351659794, -322.9825390787607375 ) ) ;
#62891 = CARTESIAN_POINT ( 'NONE',  ( -110.9086457292433323, -283.0838799473302743, -273.6464854542089711 ) ) ;
#62893 = CARTESIAN_POINT ( 'NONE',  ( -105.9414742505485805, -286.1038143642189766, -244.2612809240529259 ) ) ;
#62894 = CARTESIAN_POINT ( 'NONE',  ( 33.30816297238585122, -273.8799286643911159, -295.6854099585915492 ) ) ;
#62895 = CARTESIAN_POINT ( 'NONE',  ( -2.569593827681122544, -284.9040818245816240, -202.5428220803055694 ) ) ;
#62896 = CARTESIAN_POINT ( 'NONE',  ( -110.3339370816083402, -298.7736498775735754, -253.1235428115089405 ) ) ;
#62897 = CARTESIAN_POINT ( 'NONE',  ( 15.38143230689477114, -286.3095632045445882, -324.0086489772669438 ) ) ;
#62898 = CARTESIAN_POINT ( 'NONE',  ( 7.276217091799201953, -281.6183160108930110, -212.2224417748704468 ) ) ;
#62899 = CARTESIAN_POINT ( 'NONE',  ( 18.28507042199051469, -290.2562433912549977, -320.9341382708565220 ) ) ;
#62900 = FACE_OUTER_BOUND ( 'NONE', #27692, .T. ) ;
#62901 = CARTESIAN_POINT ( 'NONE',  ( 197.2116943569230330, 250.5000000000000568, -12.92446933126074882 ) ) ;
#62902 = CARTESIAN_POINT ( 'NONE',  ( -34.87666172331756087, -296.9415597403174729, -345.8809020549210800 ) ) ;
#62903 = CIRCLE ( 'NONE', #15975, 0.5000000000000004441 ) ;
#62904 = CARTESIAN_POINT ( 'NONE',  ( -5.908577103291047905, -278.4651481934769777, -202.2518735649484540 ) ) ;
#62905 = CARTESIAN_POINT ( 'NONE',  ( -40.61528673981563742, -291.2091670697136010, -193.5792037521810016 ) ) ;
#62906 = CARTESIAN_POINT ( 'NONE',  ( -99.41713041296493714, -294.4045521173682687, -310.3681965872725073 ) ) ;
#62907 = CARTESIAN_POINT ( 'NONE',  ( -51.90883385042970133, -278.5467815078978333, -198.2740339955405204 ) ) ;
#62908 = CARTESIAN_POINT ( 'NONE',  ( -62.49369408153998506, -271.8021710862097962, -200.2990640778067757 ) ) ;
#62909 = CARTESIAN_POINT ( 'NONE',  ( 35.39342291899473025, -294.7293772289272624, -259.8328059852659635 ) ) ;
#62910 = CARTESIAN_POINT ( 'NONE',  ( 31.95455697924148097, -295.6233781216988064, -236.9535640164627353 ) ) ;
#62911 = CARTESIAN_POINT ( 'NONE',  ( -95.03407431894771662, -295.7135370613038390, -220.3393383413759352 ) ) ;
#62912 = CARTESIAN_POINT ( 'NONE',  ( 8.260931808884707905, -290.9059231811346535, -209.5140718200036360 ) ) ;
#62913 = CARTESIAN_POINT ( 'NONE',  ( -108.3250105716817018, -292.2318142205533036, -250.9512092582315574 ) ) ;
#62914 = DIRECTION ( 'NONE',  ( 0.000000000000000000, 0.000000000000000000, 1.000000000000000000 ) ) ;
#62915 = CARTESIAN_POINT ( 'NONE',  ( -108.5870575165715906, -291.5746558785640445, -253.6721269581376248 ) ) ;
#62917 = ADVANCED_FACE ( 'NONE', ( #64292 ), #4033, .F. ) ;
#62916 = DIRECTION ( 'NONE',  ( 0.000000000000000000, 0.000000000000000000, 1.000000000000000000 ) ) ;
#62918 = CARTESIAN_POINT ( 'NONE',  ( -108.0067872313346555, -292.1352898968351042, -240.7899465098449241 ) ) ;
#62920 = CARTESIAN_POINT ( 'NONE',  ( 28.73851934338674852, -293.1316699626568720, -239.2191702651877563 ) ) ;
#62919 = CARTESIAN_POINT ( 'NONE',  ( 36.38088179767473918, -279.3721047181546169, -254.6984028828678674 ) ) ;
#62921 = CARTESIAN_POINT ( 'NONE',  ( -33.91527208777033309, -280.0941422505261471, -193.4373921830085976 ) ) ;
#62922 = CARTESIAN_POINT ( 'NONE',  ( -71.73310343550872403, -283.1609349047666342, -339.2303830446265351 ) ) ;
#62923 = CARTESIAN_POINT ( 'NONE',  ( -7.510504608907572432, -286.6601309750301425, -339.0468780394057831 ) ) ;
#62924 = CARTESIAN_POINT ( 'NONE',  ( -38.93494977148413483, -281.2118977029681446, -344.5919244412208400 ) ) ;
#62925 = ADVANCED_FACE ( 'NONE', ( #18125 ), #82092, .T. ) ;
#62926 = CARTESIAN_POINT ( 'NONE',  ( 156.4851178187871312, 1.734723475976806897E-15, -8.757359312880714342 ) ) ;
#62927 = CARTESIAN_POINT ( 'NONE',  ( 22.34521453128182245, -279.3895684952228180, -222.7989874003200725 ) ) ;
#62928 = CARTESIAN_POINT ( 'NONE',  ( 9.632308049755831547, -285.6018915366936994, -209.7398752982981307 ) ) ;
#62929 = CARTESIAN_POINT ( 'NONE',  ( 195.4781563537916043, 39.36132622696000283, 15.00000000000000000 ) ) ;
#62930 = CARTESIAN_POINT ( 'NONE',  ( 2.657163409574414548, -294.1981345100086287, -208.2801804540858086 ) ) ;
#62931 = CARTESIAN_POINT ( 'NONE',  ( 37.05700466529671644, -276.7572307047765321, -252.8847590872648823 ) ) ;
#62932 = CARTESIAN_POINT ( 'NONE',  ( -41.86213296151034768, -276.7773636218395268, -343.2548073034763547 ) ) ;
#62933 = CARTESIAN_POINT ( 'NONE',  ( -114.3688950888626010, -290.7438982589487750, -268.3568302062585644 ) ) ;
#62934 = CARTESIAN_POINT ( 'NONE',  ( -8.609536595199514863, -280.7590582649959288, -340.3006158934864516 ) ) ;
#62935 = CARTESIAN_POINT ( 'NONE',  ( 27.36034946782058697, -293.0780598728592850, -304.7776605350622958 ) ) ;
#62936 = CARTESIAN_POINT ( 'NONE',  ( -99.97253308030437324, -293.9939406138062168, -311.7149894650987676 ) ) ;
#62937 = ORIENTED_EDGE ( 'NONE', *, *, #53136, .F. ) ;
#62938 = DIRECTION ( 'NONE',  ( 0.000000000000000000, 0.000000000000000000, 1.000000000000000000 ) ) ;
#62939 = CARTESIAN_POINT ( 'NONE',  ( -6.009558495371358333, -291.9830887588749420, -204.3451621647675438 ) ) ;
#62940 = DIRECTION ( 'NONE',  ( -1.000000000000000000, 1.124465274301078034E-16, 0.000000000000000000 ) ) ;
#62941 = CARTESIAN_POINT ( 'NONE',  ( 27.36219212280433055, -290.6237833571632905, -239.2376011013261916 ) ) ;
#62942 = CARTESIAN_POINT ( 'NONE',  ( -84.05156032424358159, -294.7348872477481905, -331.3461990942407169 ) ) ;
#62943 = CARTESIAN_POINT ( 'NONE',  ( -5.442139754822084896, -278.6069473959025231, -201.6390434204160726 ) ) ;
#62944 = CARTESIAN_POINT ( 'NONE',  ( 17.98322886151547095, -288.1393186530651178, -217.4410906866914104 ) ) ;
#62945 = CARTESIAN_POINT ( 'NONE',  ( -33.23653420753078791, -285.9384604510279928, -197.4268167114228731 ) ) ;
#62946 = CARTESIAN_POINT ( 'NONE',  ( -104.8993250691448651, -279.6786411173748661, -299.9282527001880112 ) ) ;
#62947 = CARTESIAN_POINT ( 'NONE',  ( -66.72326839700113510, -293.4591052919566323, -338.9801404968505949 ) ) ;
#62948 = CARTESIAN_POINT ( 'NONE',  ( -105.7066689261908152, -298.6873665103134954, -242.0026086325144945 ) ) ;
#62949 = CARTESIAN_POINT ( 'NONE',  ( -66.97698224585701610, -276.2443920269375326, -337.5093164660243588 ) ) ;
#62950 = ORIENTED_EDGE ( 'NONE', *, *, #49823, .T. ) ;
#62951 = DIRECTION ( 'NONE',  ( 1.110223024625156343E-15, 0.000000000000000000, 1.000000000000000000 ) ) ;
#62952 = CARTESIAN_POINT ( 'NONE',  ( -112.5853914706824384, -296.0155619273755292, -286.6132318385991198 ) ) ;
#62953 = CARTESIAN_POINT ( 'NONE',  ( -111.7766795392387280, -292.4611241211823085, -271.2260081213711373 ) ) ;
#62954 = CARTESIAN_POINT ( 'NONE',  ( 200.6103193995254230, 215.0000000000000568, -2.464576988612307229 ) ) ;
#62955 = CARTESIAN_POINT ( 'NONE',  ( 5.911606060737495838, -289.0997892723691507, -329.3567472422961373 ) ) ;
#62956 = CARTESIAN_POINT ( 'NONE',  ( -48.18343439339819412, -255.4970356414862067, -444.4998647227852757 ) ) ;
#62957 = ORIENTED_EDGE ( 'NONE', *, *, #90893, .F. ) ;
#62958 = CARTESIAN_POINT ( 'NONE',  ( 8.415927329374962795, -279.7199359037391559, -208.6585210858092694 ) ) ;
#62959 = CARTESIAN_POINT ( 'NONE',  ( -113.6746020047743855, -297.3201015453374794, -261.0551587327499874 ) ) ;
#62960 = CARTESIAN_POINT ( 'NONE',  ( -113.1544149194921545, -288.6811845646618622, -271.1911935244992833 ) ) ;
#62961 = CARTESIAN_POINT ( 'NONE',  ( -107.7554091008276629, -297.2839048980356438, -239.1221747997875298 ) ) ;
#62962 = CARTESIAN_POINT ( 'NONE',  ( 34.08914667304610191, -294.0861079428870539, -285.5776803526617869 ) ) ;
#62963 = CARTESIAN_POINT ( 'NONE',  ( 200.4551663813218454, 64.49084098419280053, -2.617322427804798401 ) ) ;
#62964 = CARTESIAN_POINT ( 'NONE',  ( 184.7149167944524493, 8.542400036368780647, 10.00000000000000000 ) ) ;
#62965 = DIRECTION ( 'NONE',  ( -1.000000000000000000, 1.124465274301078034E-16, 0.000000000000000000 ) ) ;
#62966 = CARTESIAN_POINT ( 'NONE',  ( -5.894384702698338252, -290.1663095515484656, -339.8864666494469020 ) ) ;
#62967 = CARTESIAN_POINT ( 'NONE',  ( -72.08107566293803359, -282.1233781216987495, -198.2974183793908196 ) ) ;
#62968 = CARTESIAN_POINT ( 'NONE',  ( 37.44728912312089619, -281.1253883190915417, -288.3035628995652360 ) ) ;
#62969 = CARTESIAN_POINT ( 'NONE',  ( -106.2965543353912778, -286.9345090002192364, -241.1545224080606431 ) ) ;
#62970 = CARTESIAN_POINT ( 'NONE',  ( 28.20252731901684484, -285.6095947461273568, -230.9835893174585806 ) ) ;
#62971 = CARTESIAN_POINT ( 'NONE',  ( -77.52780789517017013, -271.5113161129791024, -207.2334285922567290 ) ) ;
#62972 = CARTESIAN_POINT ( 'NONE',  ( -63.84176572078402501, -275.6240890019755057, -200.7839986880234733 ) ) ;
#62973 = CARTESIAN_POINT ( 'NONE',  ( -97.74104977539028027, -288.0353022217424837, -313.8724126285737839 ) ) ;
#62974 = CARTESIAN_POINT ( 'NONE',  ( -86.27901104557732026, -279.5828220867237519, -328.2695663050141661 ) ) ;
#62975 = AXIS2_PLACEMENT_3D ( 'NONE', #62964, #22629, #8878 ) ;
#62976 = ORIENTED_EDGE ( 'NONE', *, *, #87763, .T. ) ;
#62978 = CARTESIAN_POINT ( 'NONE',  ( 21.41584665055057712, -280.2915751626857173, -226.8493195680522376 ) ) ;
#62977 = CARTESIAN_POINT ( 'NONE',  ( 20.51592719969110235, -280.9254442952920385, -225.8268154904255596 ) ) ;
#62979 = CARTESIAN_POINT ( 'NONE',  ( 21.50232542350060427, -277.2963200325701223, -319.5431590923438989 ) ) ;
#62980 = CARTESIAN_POINT ( 'NONE',  ( -95.59381759742383622, -278.0217602610235872, -220.5946240181123699 ) ) ;
#62981 = CARTESIAN_POINT ( 'NONE',  ( 187.5019281953806853, 269.8710585761918423, -138.0480249882951966 ) ) ;
#62982 = CARTESIAN_POINT ( 'NONE',  ( -102.5255871153598122, -274.0254342178769775, -229.8163144950540584 ) ) ;
#62983 = CONTEXT_DEPENDENT_SHAPE_REPRESENTATION ( #44458, #35361 ) ;
#62984 = CARTESIAN_POINT ( 'NONE',  ( -33.39078516767594351, -299.5259680346137543, -193.9494065657861199 ) ) ;
#62985 = CARTESIAN_POINT ( 'NONE',  ( -110.4683760289727132, -287.2662352645559167, -253.7030783399848985 ) ) ;
#62986 = VERTEX_POINT ( 'NONE', #52240 ) ;
#62987 = CARTESIAN_POINT ( 'NONE',  ( 155.2898987420118431, 20.78850644404472092, -13.36622507082863187 ) ) ;
#62988 = CARTESIAN_POINT ( 'NONE',  ( 35.58047339840869938, -288.5330178477315144, -262.8389719184933710 ) ) ;
#62989 = CARTESIAN_POINT ( 'NONE',  ( 30.50679229513355395, -288.8661463523419570, -236.1477275161182945 ) ) ;
#62990 = CARTESIAN_POINT ( 'NONE',  ( -45.38188668910025569, -288.5052955228564429, -343.0195522360081100 ) ) ;
#62991 = CARTESIAN_POINT ( 'NONE',  ( -96.22726432595374035, -283.3923128855403206, -319.8993522678615022 ) ) ;
#62992 = CARTESIAN_POINT ( 'NONE',  ( -43.80102293886467635, -278.3691711371228621, -196.7935492732414389 ) ) ;
#62993 = CARTESIAN_POINT ( 'NONE',  ( 7.657163490996349964, -288.5337548566711234, -211.2541008828198414 ) ) ;
#62994 = CARTESIAN_POINT ( 'NONE',  ( 23.14287389781567228, -280.6133122705425080, -312.4600972807643302 ) ) ;
#62995 = CARTESIAN_POINT ( 'NONE',  ( -105.7205482372036442, -279.5095117948940810, -297.2976472374737114 ) ) ;
#62996 = CARTESIAN_POINT ( 'NONE',  ( -7.476765155910844562, -277.1420140158919025, -337.0400059527298140 ) ) ;
#62997 = EDGE_CURVE ( 'NONE', #58890, #6488, #76021, .T. ) ;
#62998 = CARTESIAN_POINT ( 'NONE',  ( -94.40521616531121651, -290.0439362521408952, -219.2556989306164326 ) ) ;
#62999 = CARTESIAN_POINT ( 'NONE',  ( -112.8415326572952040, -285.5373813710221498, -255.8035268155682331 ) ) ;
#63000 = CARTESIAN_POINT ( 'NONE',  ( -66.54707913852071499, -283.9168772016176376, -341.5551538606963504 ) ) ;
#63001 = CARTESIAN_POINT ( 'NONE',  ( 35.68732266494509275, -281.6953566651343408, -268.5814587123384172 ) ) ;
#63002 = ORIENTED_EDGE ( 'NONE', *, *, #74417, .F. ) ;
#63003 = PLANE ( 'NONE',  #60965 ) ;
#63004 = CARTESIAN_POINT ( 'NONE',  ( -96.31347582957280906, -291.7642537253607316, -317.9487351927022019 ) ) ;
#63005 = CARTESIAN_POINT ( 'NONE',  ( -83.95255868565138258, -290.1120748682668591, -209.6253705470738851 ) ) ;
#63006 = CARTESIAN_POINT ( 'NONE',  ( 33.81229415644681779, -274.8395173125319388, -287.7493502481726750 ) ) ;
#63007 = CARTESIAN_POINT ( 'NONE',  ( -88.54375269322400754, -295.0963862060222596, -327.8055429196993487 ) ) ;
#63008 = CARTESIAN_POINT ( 'NONE',  ( -95.65122973878563073, -289.6605476513375379, -225.2977569117147141 ) ) ;
#63009 = CARTESIAN_POINT ( 'NONE',  ( -37.01325550997965053, -293.2878102028650460, -344.3863221695962693 ) ) ;
#63010 = CARTESIAN_POINT ( 'NONE',  ( -48.10412734459646344, -290.3970666987169125, -343.0161400735657935 ) ) ;
#63011 = CARTESIAN_POINT ( 'NONE',  ( 144.7857639756989272, -299.5541904835127980, -195.3611179825600175 ) ) ;
#63012 = CARTESIAN_POINT ( 'NONE',  ( -106.5321357785026350, -292.9302466554339617, -241.4183423629412459 ) ) ;
#63013 = CARTESIAN_POINT ( 'NONE',  ( 34.54137347435882077, -291.2693564594903251, -248.3872208175358196 ) ) ;
#63014 = CARTESIAN_POINT ( 'NONE',  ( 13.53410190626144782, -296.3404442286606582, -325.5364432101684997 ) ) ;
#63015 = CARTESIAN_POINT ( 'NONE',  ( -42.70327816994743841, -286.9241369061987257, -197.3096816253706436 ) ) ;
#63016 = CARTESIAN_POINT ( 'NONE',  ( -2.787045161349277045, -296.5965519407339457, -337.1144268880131563 ) ) ;
#63017 = CARTESIAN_POINT ( 'NONE',  ( 28.49789851870281154, -277.0452721716859514, -233.5993599668678087 ) ) ;
#63018 = CARTESIAN_POINT ( 'NONE',  ( 7.881302469686009893, -297.8020023944824857, -193.5285642472007055 ) ) ;
#63019 = CARTESIAN_POINT ( 'NONE',  ( 34.87716369859120391, -274.0035260184302501, -286.6177373220539266 ) ) ;
#63020 = CARTESIAN_POINT ( 'NONE',  ( 12.28363644438488400, -278.8292342793239982, -214.8756228918846034 ) ) ;
#63021 = CARTESIAN_POINT ( 'NONE',  ( -108.3280588312201473, -274.0045668547690525, -251.5095116243433608 ) ) ;
#63022 = CARTESIAN_POINT ( 'NONE',  ( -10.53717619024843799, -272.9696853844420161, -198.7497827230926930 ) ) ;
#63023 = CARTESIAN_POINT ( 'NONE',  ( -42.41235240578507160, -296.5426295729634489, -343.7754449430537989 ) ) ;
#63024 = ADVANCED_FACE ( 'NONE', ( #81122 ), #17200, .F. ) ;
#63025 = LINE ( 'NONE', #76269, #24799 ) ;
#63026 = CARTESIAN_POINT ( 'NONE',  ( -109.0409304586767547, -297.1625973445115960, -284.9775745624945671 ) ) ;
#63027 = CARTESIAN_POINT ( 'NONE',  ( 140.6539576904058606, 130.0000000000000568, 12.50000000000000000 ) ) ;
#63029 = CARTESIAN_POINT ( 'NONE',  ( -49.95391831840064611, -297.8867250657352770, -198.4588791278499684 ) ) ;
#63028 = CARTESIAN_POINT ( 'NONE',  ( -77.28637229139522447, -287.6046118384602437, -334.3190240826729109 ) ) ;
#63030 = CARTESIAN_POINT ( 'NONE',  ( 9.810754700973625120, -286.6813891697905774, -209.4871005071713057 ) ) ;
#63031 = CARTESIAN_POINT ( 'NONE',  ( -109.8470693738500188, -289.8906024269907675, -296.3787106952124759 ) ) ;
#63032 = CARTESIAN_POINT ( 'NONE',  ( -103.8148314366280403, -299.0019721543181959, -234.7576870238316360 ) ) ;
#63033 = CARTESIAN_POINT ( 'NONE',  ( 36.11935118030471159, -291.7355669314308102, -284.6265436685044392 ) ) ;
#63034 = CARTESIAN_POINT ( 'NONE',  ( 39.54891352599890553, -280.7440604015646386, -269.9413761089698482 ) ) ;
#63035 = CARTESIAN_POINT ( 'NONE',  ( 21.31550574532286291, -290.4094976428776249, -223.6242672951989618 ) ) ;
#63036 = CARTESIAN_POINT ( 'NONE',  ( -91.87266939285095191, -277.2745298032613164, -218.7952315409555695 ) ) ;
#63037 = CARTESIAN_POINT ( 'NONE',  ( 21.48256938208964328, -286.9599158639961161, -314.2778893322750946 ) ) ;
#63038 = DIRECTION ( 'NONE',  ( 0.000000000000000000, 0.000000000000000000, -1.000000000000000000 ) ) ;
#63039 = CARTESIAN_POINT ( 'NONE',  ( -17.98113100053491564, -286.8025241097366234, -342.8731896050754244 ) ) ;
#63040 = CARTESIAN_POINT ( 'NONE',  ( -92.45575991057086185, -298.8464650905340250, -221.2807672255001421 ) ) ;
#63041 = CARTESIAN_POINT ( 'NONE',  ( 35.91899233989964557, -283.2540110621814051, -292.2568177500588149 ) ) ;
#63043 = CARTESIAN_POINT ( 'NONE',  ( 25.13628627644695257, -281.0312801971525687, -232.5073484677236308 ) ) ;
#63042 = CARTESIAN_POINT ( 'NONE',  ( -104.3209367327989412, -271.0930668772665513, -235.2753132652601664 ) ) ;
#63044 = CARTESIAN_POINT ( 'NONE',  ( -101.5508621032647767, -297.2781296578212391, -227.8378898526343050 ) ) ;
#63045 = CARTESIAN_POINT ( 'NONE',  ( 23.52960700504146629, -276.4066530978067817, -228.9856649250569092 ) ) ;
#63046 = CARTESIAN_POINT ( 'NONE',  ( 36.09891721298755840, -285.8591459495142431, -288.1861810035260874 ) ) ;
#63047 = EDGE_CURVE ( 'NONE', #56700, #30213, #35207, .T. ) ;
#63048 = CARTESIAN_POINT ( 'NONE',  ( 36.18987807317616046, -283.7419359971148083, -285.1295863958147265 ) ) ;
#63049 = CARTESIAN_POINT ( 'NONE',  ( -81.24518144970640776, -272.3600777484548985, -211.5887380426867423 ) ) ;
#63050 = B_SPLINE_CURVE_WITH_KNOTS ( 'NONE', 3,
 ( #58811, #15247, #80563, #79200 ),
 .UNSPECIFIED., .F., .F.,
 ( 4, 4 ),
 ( 3.469446951953614189E-18, 9.632970524405874116E-05 ),
 .UNSPECIFIED. ) ;
#63051 = VERTEX_POINT ( 'NONE', #60756 ) ;
#63052 = CARTESIAN_POINT ( 'NONE',  ( 82.64890176555634582, -299.5541904835127980, -195.3611179825600175 ) ) ;
#63053 = CARTESIAN_POINT ( 'NONE',  ( -109.9716505721188895, -286.7549320166768894, -253.0799303444032944 ) ) ;
#63054 = CARTESIAN_POINT ( 'NONE',  ( 152.4536156746142410, 249.5000000000000568, 14.50000000000000000 ) ) ;
#63055 = CARTESIAN_POINT ( 'NONE',  ( 44.71564893372296723, -279.0523547857346784, -270.3937649182068412 ) ) ;
#63056 = CARTESIAN_POINT ( 'NONE',  ( -17.40965896147221770, -275.9984474728133819, -344.5694231441364082 ) ) ;
#63057 = CARTESIAN_POINT ( 'NONE',  ( 6.015484892702065878, -283.9719618248271331, -329.9502298889095755 ) ) ;
#63058 = CARTESIAN_POINT ( 'NONE',  ( 22.11372566371886350, -276.5463265229942067, -226.6404962973884949 ) ) ;
#63059 = CARTESIAN_POINT ( 'NONE',  ( -113.2365138387976913, -286.0891424024634944, -261.4963819996870598 ) ) ;
#63060 = CARTESIAN_POINT ( 'NONE',  ( -59.08029767950522171, -282.1345941859328832, -340.5185030085810922 ) ) ;
#63061 = CARTESIAN_POINT ( 'NONE',  ( 23.72760538252448370, -282.9602990357549857, -226.8233117126235925 ) ) ;
#63062 = CARTESIAN_POINT ( 'NONE',  ( -63.55908921140584766, -273.8863641589410918, -197.9618879165280987 ) ) ;
#63063 = CARTESIAN_POINT ( 'NONE',  ( 24.36638555847289922, -275.9981441450905209, -316.4166514766521914 ) ) ;
#63064 = CARTESIAN_POINT ( 'NONE',  ( -47.97502623523742926, -297.1084677946071224, -344.0900425622648413 ) ) ;
#63065 = FACE_OUTER_BOUND ( 'NONE', #21635, .T. ) ;
#63066 = CARTESIAN_POINT ( 'NONE',  ( -147.8070425842520308, 32.24468615100210656, 21.50000000000000000 ) ) ;
#63067 = CARTESIAN_POINT ( 'NONE',  ( -110.4241862647871670, -294.9483128571727661, -250.1861018454835062 ) ) ;
#63068 = CARTESIAN_POINT ( 'NONE',  ( 34.68738188461561833, -274.8975026681275722, -258.0474996951396633 ) ) ;
#63069 = CARTESIAN_POINT ( 'NONE',  ( -113.7859253652709555, -273.8287563820230162, -264.6711018824900066 ) ) ;
#63070 = CARTESIAN_POINT ( 'NONE',  ( -67.98745683035579646, -287.4043267569894056, -202.9904150614670755 ) ) ;
#63071 = CARTESIAN_POINT ( 'NONE',  ( -30.63245572179668486, -296.4888931318121195, -346.3722605337579807 ) ) ;
#63072 = CARTESIAN_POINT ( 'NONE',  ( 36.31809992813148114, -294.4916979435695907, -249.2837921777557426 ) ) ;
#63073 = CARTESIAN_POINT ( 'NONE',  ( -98.03088127986349321, -291.9549833860205013, -314.1429831729067246 ) ) ;
#63074 = CARTESIAN_POINT ( 'NONE',  ( -36.97439094717415742, -278.0566052597273483, -195.5286817324358140 ) ) ;
#63075 = CARTESIAN_POINT ( 'NONE',  ( -90.51906250471800774, -281.2123537666566335, -218.1969437695659622 ) ) ;
#63076 = CARTESIAN_POINT ( 'NONE',  ( -74.03306107362777766, -293.6235409237839349, -335.1303871671878483 ) ) ;
#63077 = CARTESIAN_POINT ( 'NONE',  ( -24.71571648141593869, -284.7532668527419446, -345.1197231323229744 ) ) ;
#63078 = CARTESIAN_POINT ( 'NONE',  ( -95.19254975189075196, -284.1044808988198156, -225.3129113376041914 ) ) ;
#63079 = CARTESIAN_POINT ( 'NONE',  ( 203.7351382603598040, 291.4157354431145563, -82.94369648350118496 ) ) ;
#63080 = VERTEX_POINT ( 'NONE', #24768 ) ;
#63081 = CARTESIAN_POINT ( 'NONE',  ( -108.1147665232138735, -283.9816324131753618, -288.3405662467736192 ) ) ;
#63082 = VERTEX_POINT ( 'NONE', #39405 ) ;
#63083 = TOROIDAL_SURFACE ( 'NONE', #2573, 1.000000000000000000, 0.5000000000000000000 ) ;
#63084 = CARTESIAN_POINT ( 'NONE',  ( 1.947632823567920779, -283.6188862224968830, -336.2234048076468298 ) ) ;
#63085 = CARTESIAN_POINT ( 'NONE',  ( -104.4008067951902063, -273.2751936714635690, -241.3337623239234233 ) ) ;
#63086 = CARTESIAN_POINT ( 'NONE',  ( -12.81623908733407013, -285.1589429710763852, -197.7903905596899392 ) ) ;
#63087 = CARTESIAN_POINT ( 'NONE',  ( 37.75198460200883943, -282.2927762242015319, -254.3684718586702331 ) ) ;
#63088 =( NAMED_UNIT ( * ) SI_UNIT ( $, .STERADIAN. ) SOLID_ANGLE_UNIT ( ) );
#63089 = CARTESIAN_POINT ( 'NONE',  ( -101.5034207699642792, -279.5242982955755338, -311.7610266103919230 ) ) ;
#63090 = CARTESIAN_POINT ( 'NONE',  ( -17.02691315267212246, -280.9591996657974846, -196.1949382478952373 ) ) ;
#63091 = CARTESIAN_POINT ( 'NONE',  ( -53.28691492658257545, -277.3380690714490129, -200.3538533559491555 ) ) ;
#63092 = CARTESIAN_POINT ( 'NONE',  ( 204.3871269384557934, 295.4037104000961449, -68.67796409040960270 ) ) ;
#63093 = EDGE_LOOP ( 'NONE', ( #74009, #38010, #69805, #59700 ) ) ;
#63094 = CARTESIAN_POINT ( 'NONE',  ( -24.30138684413341110, -276.2190463901577573, -196.6198480844160770 ) ) ;
#63095 = CARTESIAN_POINT ( 'NONE',  ( 202.8071025886960115, 295.9636416993531611, -68.64508862776258979 ) ) ;
#63096 = CARTESIAN_POINT ( 'NONE',  ( -99.34612708073704823, -277.1379002975523917, -228.7086077216202398 ) ) ;
#63097 = CARTESIAN_POINT ( 'NONE',  ( 38.42891235670971639, -295.2397248284237321, -264.6350114898483525 ) ) ;
#63098 = CARTESIAN_POINT ( 'NONE',  ( -90.48703787331659498, -295.1780869321464706, -320.6283069397197210 ) ) ;
#63099 = CARTESIAN_POINT ( 'NONE',  ( -37.78837661708388396, -291.5543535914056861, -193.4239528171910081 ) ) ;
#63100 = DIRECTION ( 'NONE',  ( -0.000000000000000000, -0.000000000000000000, -1.000000000000000000 ) ) ;
#63102 = CARTESIAN_POINT ( 'NONE',  ( 0.5972259697621423724, -284.9664356176119213, -207.0000439995350803 ) ) ;
#63101 = CARTESIAN_POINT ( 'NONE',  ( -101.1463353411968171, -294.5687360818945990, -312.4993777970919950 ) ) ;
#63103 = CARTESIAN_POINT ( 'NONE',  ( 2.890354310803937121, -294.4583801239031686, -207.9123580034386407 ) ) ;
#63104 = CARTESIAN_POINT ( 'NONE',  ( 30.93717668364962847, -286.5999599355418468, -297.6872333717078050 ) ) ;
#63105 = CARTESIAN_POINT ( 'NONE',  ( -94.65916787433052093, -285.2214069291394480, -316.3806026674670306 ) ) ;
#63106 = ORIENTED_EDGE ( 'NONE', *, *, #60023, .F. ) ;
#63107 = CARTESIAN_POINT ( 'NONE',  ( -61.62554693549186169, -292.6855577214944333, -197.4826398874059521 ) ) ;
#63108 = CARTESIAN_POINT ( 'NONE',  ( 33.71146714199196737, -282.2694403430483590, -287.4271767031661966 ) ) ;
#63109 = CARTESIAN_POINT ( 'NONE',  ( -113.5497597816783042, -295.2494269696082370, -278.1290238641061592 ) ) ;
#63110 = CARTESIAN_POINT ( 'NONE',  ( -105.8647498219482799, -291.8048447638614675, -235.4766814274685771 ) ) ;
#63111 = CARTESIAN_POINT ( 'NONE',  ( -91.55071776032434627, -290.2911720534075357, -325.0337612924163295 ) ) ;
#63112 = CARTESIAN_POINT ( 'NONE',  ( 14.08488714284487209, -288.4717125818122554, -322.1714077536313994 ) ) ;
#63113 = ORIENTED_EDGE ( 'NONE', *, *, #44097, .F. ) ;
#63114 = CARTESIAN_POINT ( 'NONE',  ( 165.4421947725420523, 249.5000000000000568, 22.46007009812167254 ) ) ;
#63115 = CARTESIAN_POINT ( 'NONE',  ( -67.70899896146165986, -297.3068286217032892, -339.7738880202303449 ) ) ;
#63116 = CARTESIAN_POINT ( 'NONE',  ( -113.2832330124605846, -295.3538313999151228, -261.0776996753071444 ) ) ;
#63117 = ADVANCED_FACE ( 'NONE', ( #16265, #2531 ), #66922, .F. ) ;
#63118 = CARTESIAN_POINT ( 'NONE',  ( 9.436009348219009496, -279.7721314182165315, -213.9456066480778134 ) ) ;
#63119 = CARTESIAN_POINT ( 'NONE',  ( 39.31865375809432805, -275.1416111320269238, -276.8969457918657326 ) ) ;
#63120 = CARTESIAN_POINT ( 'NONE',  ( -94.98162655975804114, -295.6743921351554150, -224.4443820820378335 ) ) ;
#63121 = CARTESIAN_POINT ( 'NONE',  ( -48.77509254653654125, -279.0595779434141264, -343.7628323835089645 ) ) ;
#63122 = CARTESIAN_POINT ( 'NONE',  ( 34.05443350719821183, -273.4252093852364283, -249.8435697581917907 ) ) ;
#63123 = CARTESIAN_POINT ( 'NONE',  ( -100.5003757326617375, -297.2450203460318789, -307.8524960164338040 ) ) ;
#63124 = CARTESIAN_POINT ( 'NONE',  ( -84.28326906784921846, -298.4686000627070825, -213.9857250814623342 ) ) ;
#63125 = DIRECTION ( 'NONE',  ( -1.000000000000000000, 0.000000000000000000, 0.000000000000000000 ) ) ;
#63126 = CARTESIAN_POINT ( 'NONE',  ( -83.68236812177651984, -297.2758586651191308, -330.9171585209741693 ) ) ;
#63127 = CARTESIAN_POINT ( 'NONE',  ( -35.84733324182673186, -296.0706611987501446, -195.1949506821764828 ) ) ;
#63128 = CARTESIAN_POINT ( 'NONE',  ( -36.21286596702780258, -292.7180537408303280, -197.2554067769167148 ) ) ;
#63129 = CARTESIAN_POINT ( 'NONE',  ( -76.35955921404796243, -274.3475378469351540, -204.1047283533753216 ) ) ;
#63130 = CARTESIAN_POINT ( 'NONE',  ( -102.9265355052720707, -289.5779091805952703, -236.8716692833707214 ) ) ;
#63131 = DIRECTION ( 'NONE',  ( 0.000000000000000000, 0.000000000000000000, 1.000000000000000000 ) ) ;
#63132 = CARTESIAN_POINT ( 'NONE',  ( -64.88391296044297007, -274.1942506620181916, -198.5071671305449854 ) ) ;
#63133 = CARTESIAN_POINT ( 'NONE',  ( -104.7833613082437836, -297.2607361762896971, -242.3663001772050052 ) ) ;
#63134 = CARTESIAN_POINT ( 'NONE',  ( 11.89794985329147714, -282.7123680097561191, -213.3184701681800846 ) ) ;
#63135 = CARTESIAN_POINT ( 'NONE',  ( 34.12086354064076232, -280.5850996415467762, -297.6814449517692651 ) ) ;
#63136 = CARTESIAN_POINT ( 'NONE',  ( -5.334775114619859870, -275.9905264373508089, -340.2815694842814764 ) ) ;
#63137 = CARTESIAN_POINT ( 'NONE',  ( 38.39009685180050724, -279.8395848113973443, -261.4638217592255955 ) ) ;
#63138 = CARTESIAN_POINT ( 'NONE',  ( 31.50423271860621455, -279.1578583481900182, -240.1905039001952105 ) ) ;
#63139 = EDGE_CURVE ( 'NONE', #4038, #85072, #68736, .T. ) ;
#63140 = CARTESIAN_POINT ( 'NONE',  ( -48.95063505970350803, -272.4762336020547195, -197.6417438854277577 ) ) ;
#63141 = CARTESIAN_POINT ( 'NONE',  ( -110.7929881235739202, -280.7477983140753963, -255.1360513273831998 ) ) ;
#63142 = FACE_OUTER_BOUND ( 'NONE', #89467, .T. ) ;
#63143 = DIRECTION ( 'NONE',  ( -0.9693563597868444237, -0.2456588035076248677, 0.000000000000000000 ) ) ;
#63144 = CARTESIAN_POINT ( 'NONE',  ( -113.0653769905977981, -271.0595318834638761, -261.8543455666935529 ) ) ;
#63145 = CARTESIAN_POINT ( 'NONE',  ( -68.32876473972254416, -291.6562548435997542, -199.8570225637258204 ) ) ;
#63146 = CARTESIAN_POINT ( 'NONE',  ( -38.49076503620204193, -279.0666862774626793, -345.5190056618538392 ) ) ;
#63147 = CARTESIAN_POINT ( 'NONE',  ( 8.574916681755698988, -272.6810440905719588, -211.0596429048015921 ) ) ;
#63148 = FACE_OUTER_BOUND ( 'NONE', #88219, .T. ) ;
#63149 = CARTESIAN_POINT ( 'NONE',  ( 0.1750251051061615104, -284.4769181089097856, -335.9642490314248562 ) ) ;
#63150 = DIRECTION ( 'NONE',  ( -0.000000000000000000, 1.000000000000000000, -9.656854691831248164E-17 ) ) ;
#63151 = CARTESIAN_POINT ( 'NONE',  ( 5.515036019150874047, -284.6318351268753872, -208.7496893978193384 ) ) ;
#63152 = DIRECTION ( 'NONE',  ( -0.5987926743825080500, -0.8009040723493942027, 0.000000000000000000 ) ) ;
#63153 = CARTESIAN_POINT ( 'NONE',  ( -35.65680163459835939, -293.8255016288889578, -343.7514147180479540 ) ) ;
#63154 = CARTESIAN_POINT ( 'NONE',  ( 36.91660228816733280, -285.6650103968020744, -268.3014338869509743 ) ) ;
#63155 = CARTESIAN_POINT ( 'NONE',  ( 156.6695768423672632, 18.03393767897209443, -8.087387968559699658 ) ) ;
#63156 = CARTESIAN_POINT ( 'NONE',  ( -42.55345161240357754, -293.1177497459933079, -345.1798208316198497 ) ) ;
#63157 = CARTESIAN_POINT ( 'NONE',  ( -12.90723809123782040, -284.8439475063588020, -198.0723580218308939 ) ) ;
#63158 = CARTESIAN_POINT ( 'NONE',  ( -81.78572700359976011, -281.0358703315853290, -211.3803096988781647 ) ) ;
#63159 = CARTESIAN_POINT ( 'NONE',  ( -12.84528491914726622, -287.5687060532595183, -197.7805809229789418 ) ) ;
#63160 = CARTESIAN_POINT ( 'NONE',  ( 23.43099795397060703, -280.4072464380158749, -315.9752954267714813 ) ) ;
#63161 = CARTESIAN_POINT ( 'NONE',  ( 31.39940023454654394, -287.8792892662658005, -294.9306340733404568 ) ) ;
#63162 = CARTESIAN_POINT ( 'NONE',  ( -87.94890572964960995, -280.7532821244134311, -216.8651642317157098 ) ) ;
#63163 = CARTESIAN_POINT ( 'NONE',  ( -5.497429458520055157, -281.2849928933199521, -204.4934919960515458 ) ) ;
#63164 = EDGE_CURVE ( 'NONE', #33465, #50260, #48776, .T. ) ;
#63165 = CARTESIAN_POINT ( 'NONE',  ( -5.492548306803323399, -288.4489274860670776, -202.0673530014701669 ) ) ;
#63166 = EDGE_LOOP ( 'NONE', ( #12629, #16846, #15204, #22185, #75421, #81121 ) ) ;
#63167 = CARTESIAN_POINT ( 'NONE',  ( -51.79853284000595437, -297.7055434284678199, -194.6760974100936892 ) ) ;
#63168 = CARTESIAN_POINT ( 'NONE',  ( -111.7603470849426941, -292.4490297384436417, -276.7962479067879258 ) ) ;
#63169 = CARTESIAN_POINT ( 'NONE',  ( 206.1919228894574303, 35.96217941443950394, 14.00000000000000000 ) ) ;
#63170 = CARTESIAN_POINT ( 'NONE',  ( 36.60358173371528068, -296.4805209788416391, -305.9350535429201159 ) ) ;
#63171 = ORIENTED_EDGE ( 'NONE', *, *, #76146, .F. ) ;
#63172 = CARTESIAN_POINT ( 'NONE',  ( 20.45784610560596306, -272.8899438396260280, -222.3065564363317037 ) ) ;
#63173 = FACE_OUTER_BOUND ( 'NONE', #24169, .T. ) ;
#63174 = CARTESIAN_POINT ( 'NONE',  ( -32.08822024938798023, -293.3868272624400788, -346.3929257053404172 ) ) ;
#63175 = CARTESIAN_POINT ( 'NONE',  ( -110.2898752900783705, -271.9727075963631933, -264.8975838380630989 ) ) ;
#63176 = CARTESIAN_POINT ( 'NONE',  ( -5.475261845078676970, -290.1452296353871816, -336.8083742534934686 ) ) ;
#63177 = CARTESIAN_POINT ( 'NONE',  ( 35.70725670043358235, -283.4672456671130476, -282.2701028520872342 ) ) ;
#63178 = CARTESIAN_POINT ( 'NONE',  ( -107.1853551753745535, -291.5773910833514151, -301.4826362517486018 ) ) ;
#63179 = CARTESIAN_POINT ( 'NONE',  ( -112.1612496465735376, -292.0691920121191743, -254.3200924198557686 ) ) ;
#63180 = CARTESIAN_POINT ( 'NONE',  ( -96.55125785631663859, -287.1838143138775195, -224.3051723028688968 ) ) ;
#63181 = CARTESIAN_POINT ( 'NONE',  ( -69.96430761824885280, -279.8009722192398385, -200.5988576831022669 ) ) ;
#63182 = CARTESIAN_POINT ( 'NONE',  ( -112.9264217661186223, -294.6059352114793910, -272.4059589295201249 ) ) ;
#63183 = CARTESIAN_POINT ( 'NONE',  ( 24.25382670642989069, -282.0004499634582089, -316.5670816507339396 ) ) ;
#63184 = CARTESIAN_POINT ( 'NONE',  ( -1.140638441075009890, -276.3982786762053934, -205.5364679814612145 ) ) ;
#63185 = EDGE_CURVE ( 'NONE', #75524, #64758, #32339, .T. ) ;
#63186 = CARTESIAN_POINT ( 'NONE',  ( -95.99890600148557951, -299.6948066931273615, -223.6242672951989618 ) ) ;
#63187 = CARTESIAN_POINT ( 'NONE',  ( 38.69317628720677504, -273.8024309066653927, -271.1833478625718499 ) ) ;
#63188 = LINE ( 'NONE', #12496, #90793 ) ;
#63189 = CARTESIAN_POINT ( 'NONE',  ( 32.28805627210257256, -281.3549154146036244, -292.6546803726682242 ) ) ;
#63190 = CARTESIAN_POINT ( 'NONE',  ( -107.2076195978872306, -279.3524840613571314, -301.9029006145521521 ) ) ;
#63191 = CARTESIAN_POINT ( 'NONE',  ( -93.73870262587062996, -284.3228560490567247, -218.2044578175995753 ) ) ;
#63192 = CARTESIAN_POINT ( 'NONE',  ( -36.21285092549082663, -293.8266023443379709, -196.3437403653989293 ) ) ;
#63193 = CARTESIAN_POINT ( 'NONE',  ( -78.42753274434281252, -275.1091337855381767, -206.1863973163608819 ) ) ;
#63194 = CARTESIAN_POINT ( 'NONE',  ( -60.73635742049441433, -275.0701293798153984, -197.4636245745144265 ) ) ;
#63195 = CARTESIAN_POINT ( 'NONE',  ( 11.63197158325052172, -331.8906705383788562, 52.50000000000000711 ) ) ;
#63196 = CARTESIAN_POINT ( 'NONE',  ( -1.472081416084617622, -276.3960717918301384, -333.9979572841067466 ) ) ;
#63197 = CARTESIAN_POINT ( 'NONE',  ( -71.75168969512166939, -297.5080764983356403, -336.8282998311944993 ) ) ;
#63198 = CARTESIAN_POINT ( 'NONE',  ( -27.57261772641772524, -284.1763831357010304, -196.1681705154648512 ) ) ;
#63199 = CARTESIAN_POINT ( 'NONE',  ( -34.95681520275245902, -291.7480253732489928, -193.4060674126369292 ) ) ;
#63200 = CARTESIAN_POINT ( 'NONE',  ( 22.00422952914819064, -272.9493759197994223, -225.0641665144460433 ) ) ;
#63201 = CARTESIAN_POINT ( 'NONE',  ( 19.98464413268053619, -289.8387149093874200, -320.5816847339579567 ) ) ;
#63202 = CARTESIAN_POINT ( 'NONE',  ( -110.6766662959683885, -289.4977101895710803, -268.4399982533130924 ) ) ;
#63203 = ORIENTED_EDGE ( 'NONE', *, *, #36505, .F. ) ;
#63204 = CARTESIAN_POINT ( 'NONE',  ( 10.76203714416920398, -291.2766798812465368, -210.9243793734091241 ) ) ;
#63205 = CARTESIAN_POINT ( 'NONE',  ( -101.6637814664811259, -289.7463750275625216, -305.0335967805089012 ) ) ;
#63206 = ORIENTED_EDGE ( 'NONE', *, *, #17291, .F. ) ;
#63207 = CARTESIAN_POINT ( 'NONE',  ( 28.42635435392962506, -288.1141349376257494, -230.8118584029870703 ) ) ;
#63208 = CARTESIAN_POINT ( 'NONE',  ( -108.3112203614117846, -279.1121394554951394, -253.1734862457694533 ) ) ;
#63209 = CARTESIAN_POINT ( 'NONE',  ( -86.20896796138724483, -294.6323435329302924, -329.4668084310036988 ) ) ;
#63210 = CARTESIAN_POINT ( 'NONE',  ( -32.32136991245290858, -286.7652765054399993, -193.6139540210300822 ) ) ;
#63211 = CARTESIAN_POINT ( 'NONE',  ( -76.09974660554641446, -285.8827376696555120, -203.7898980279237549 ) ) ;
#63212 = CARTESIAN_POINT ( 'NONE',  ( -10.96417174173520692, -283.0319818911924585, -338.5051956362725036 ) ) ;
#63213 = CARTESIAN_POINT ( 'NONE',  ( 138.8680847268318814, 180.6334471161891031, -241.4751441910937899 ) ) ;
#63214 = CARTESIAN_POINT ( 'NONE',  ( -114.3093312043316132, -271.9319807694569135, -283.9828466565109011 ) ) ;
#63215 = CARTESIAN_POINT ( 'NONE',  ( 183.5144294471984381, 261.3764885010062926, -151.1767051898502530 ) ) ;
#63216 = CARTESIAN_POINT ( 'NONE',  ( 23.93431497806644614, -274.1966492604556151, -230.3879807570918103 ) ) ;
#63217 = CARTESIAN_POINT ( 'NONE',  ( 35.91006722011604779, -274.5247815569367731, -274.3430696287165347 ) ) ;
#63218 = CARTESIAN_POINT ( 'NONE',  ( -111.5343403596023819, -295.8044288841543903, -290.7321522920910297 ) ) ;
#63219 = CARTESIAN_POINT ( 'NONE',  ( 85.54234477158686900, 81.19049204599852487, -299.1564525335649591 ) ) ;
#63220 = CARTESIAN_POINT ( 'NONE',  ( 37.73804855772906564, -274.0518521039967368, -255.6529701949339426 ) ) ;
#63221 = CARTESIAN_POINT ( 'NONE',  ( -91.88425395836236476, -275.0206243463375131, -220.3115213371761456 ) ) ;
#63222 = CARTESIAN_POINT ( 'NONE',  ( -91.91241638468210340, -292.3295968127715696, -221.3906983321252540 ) ) ;
#63223 = ORIENTED_EDGE ( 'NONE', *, *, #66418, .F. ) ;
#63224 = CARTESIAN_POINT ( 'NONE',  ( -103.6526159665097424, -297.9993407255161628, -231.5822784496067470 ) ) ;
#63225 = CARTESIAN_POINT ( 'NONE',  ( 35.51378855602177254, -288.1251559077391562, -276.4802535409087909 ) ) ;
#63226 = CARTESIAN_POINT ( 'NONE',  ( -68.15202833535775540, -296.2494162280391379, -340.7520442207594442 ) ) ;
#63227 = CARTESIAN_POINT ( 'NONE',  ( -101.5734321378067335, -296.4860463053695980, -312.8108698787508501 ) ) ;
#63228 = CARTESIAN_POINT ( 'NONE',  ( 8.847199111232466606, -292.8725799752006083, -213.7660430709252353 ) ) ;
#63229 = ORIENTED_EDGE ( 'NONE', *, *, #22620, .F. ) ;
#63230 = CARTESIAN_POINT ( 'NONE',  ( 9.649993932451877754, -278.3319237031839180, -329.5979980628904400 ) ) ;
#63231 = EDGE_CURVE ( 'NONE', #30244, #77857, #66971, .T. ) ;
#63232 = ORIENTED_EDGE ( 'NONE', *, *, #1762, .T. ) ;
#63233 = CARTESIAN_POINT ( 'NONE',  ( 21.92731382997954981, -280.3998111506041937, -221.3028782268150962 ) ) ;
#63234 = AXIS2_PLACEMENT_3D ( 'NONE', #4334, #63538, #77242 ) ;
#63235 = CARTESIAN_POINT ( 'NONE',  ( 11.91479219664280720, -277.2890571715314536, -324.6259421384361872 ) ) ;
#63236 = CARTESIAN_POINT ( 'NONE',  ( 24.48912554410425813, -276.7191217165149055, -226.1696133046375792 ) ) ;
#63237 = CARTESIAN_POINT ( 'NONE',  ( -112.4421988741684402, -276.4854099179709692, -277.1571048728020514 ) ) ;
#63238 = CARTESIAN_POINT ( 'NONE',  ( -77.57498951706452317, -298.1481362308763892, -209.2660732051698176 ) ) ;
#63239 = CARTESIAN_POINT ( 'NONE',  ( -100.6828221755220909, -294.6150959388896808, -307.9218366813141756 ) ) ;
#63240 = PLANE ( 'NONE',  #48707 ) ;
#63241 = CARTESIAN_POINT ( 'NONE',  ( 22.82326365675837820, -281.4017117710948241, -222.3849455507653090 ) ) ;
#63242 = CARTESIAN_POINT ( 'NONE',  ( 33.89373311509346109, -275.9300352735922388, -286.3714315939866424 ) ) ;
#63243 = CARTESIAN_POINT ( 'NONE',  ( 13.92890161770685076, -285.4381813583173084, -213.5042571678424963 ) ) ;
#63244 = CARTESIAN_POINT ( 'NONE',  ( -40.39199204732053516, -300.0141807766151487, -195.2054793147930525 ) ) ;
#63245 = DIRECTION ( 'NONE',  ( -0.000000000000000000, 1.000000000000000000, 0.000000000000000000 ) ) ;
#63246 = CARTESIAN_POINT ( 'NONE',  ( 20.47453412858477506, -286.1192738877761030, -225.5293794050041924 ) ) ;
#63247 = CARTESIAN_POINT ( 'NONE',  ( 20.48154518866151363, -279.1482848145506068, -224.1610496080544124 ) ) ;
#63249 = CARTESIAN_POINT ( 'NONE',  ( -51.31165164250147370, -281.3118382834701947, -343.5311176431419540 ) ) ;
#63248 = CARTESIAN_POINT ( 'NONE',  ( -74.79012999345189883, -278.1182157286625056, -206.9543895945637644 ) ) ;
#63250 = CARTESIAN_POINT ( 'NONE',  ( -5.285663586863666552, -288.4740437397809956, -202.5430161413130747 ) ) ;
#63251 = CARTESIAN_POINT ( 'NONE',  ( -26.95021117837024605, -278.1221545454647526, -343.0188599066872825 ) ) ;
#63252 = DIRECTION ( 'NONE',  ( 0.000000000000000000, 0.000000000000000000, 1.000000000000000000 ) ) ;
#63253 = CARTESIAN_POINT ( 'NONE',  ( 22.36712787761467780, -294.9310972204266363, -224.9543510085378557 ) ) ;
#63254 = CARTESIAN_POINT ( 'NONE',  ( -111.1956788631972870, -276.5647775228716228, -288.2920306373241033 ) ) ;
#63255 = CARTESIAN_POINT ( 'NONE',  ( -59.21761157775852524, -277.9943410688059089, -340.1130868881748484 ) ) ;
#63256 = CARTESIAN_POINT ( 'NONE',  ( 20.22282853303963535, -284.2189616330234117, -318.6969584108889535 ) ) ;
#63257 = DIRECTION ( 'NONE',  ( 0.000000000000000000, -0.000000000000000000, -1.000000000000000000 ) ) ;
#63258 = CARTESIAN_POINT ( 'NONE',  ( -107.4530336370362562, -292.1079338968769434, -298.5340679407805169 ) ) ;
#63259 = CARTESIAN_POINT ( 'NONE',  ( -112.3178643632237339, -294.5950691873683809, -267.0058100862269725 ) ) ;
#63260 = CARTESIAN_POINT ( 'NONE',  ( -35.14259250810531654, -285.2762442845022974, -193.5409534053348750 ) ) ;
#63261 = DIRECTION ( 'NONE',  ( -1.000000000000000000, 0.000000000000000000, 0.000000000000000000 ) ) ;
#63262 = CARTESIAN_POINT ( 'NONE',  ( 29.54175329825874030, -273.8275906543187261, -239.7773650165581500 ) ) ;
#63263 = CARTESIAN_POINT ( 'NONE',  ( 22.81941209189212927, -291.0932141143767353, -226.8480447967785381 ) ) ;
#63264 = DIRECTION ( 'NONE',  ( 0.000000000000000000, 0.000000000000000000, 1.000000000000000000 ) ) ;
#63265 = CARTESIAN_POINT ( 'NONE',  ( 138.6539576904058606, 275.5000000000000568, 10.50000000000000000 ) ) ;
#63266 = CARTESIAN_POINT ( 'NONE',  ( -110.9587438908396422, -289.2863944448677671, -250.2307816561519758 ) ) ;
#63267 = CARTESIAN_POINT ( 'NONE',  ( -95.73708873633613337, -285.5235509007023893, -315.5084392600292063 ) ) ;
#63268 = CARTESIAN_POINT ( 'NONE',  ( -21.17738660665003891, -284.4966322767228917, -196.1136333135789869 ) ) ;
#63269 = CARTESIAN_POINT ( 'NONE',  ( -107.0966143826628354, -286.2882375635215908, -246.7573178097935340 ) ) ;
#63270 = CARTESIAN_POINT ( 'NONE',  ( -83.75819036978028009, -286.1991106314869739, -213.7434415420709115 ) ) ;
#63271 = CARTESIAN_POINT ( 'NONE',  ( -105.7774696973465609, -292.9457699474629067, -238.6938416093715603 ) ) ;
#63272 = CARTESIAN_POINT ( 'NONE',  ( 36.54258831923565509, -273.4295390553292009, -254.4750028838569449 ) ) ;
#63273 = CARTESIAN_POINT ( 'NONE',  ( -17.35929706935331041, -277.1343783495568687, -344.7012004377090193 ) ) ;
#63274 = CARTESIAN_POINT ( 'NONE',  ( -108.1162850536406239, -288.9747752233414531, -243.7494825035878989 ) ) ;
#63275 = CARTESIAN_POINT ( 'NONE',  ( -82.23885752248339998, -279.4580821340770171, -207.8051809509536838 ) ) ;
#63276 = CARTESIAN_POINT ( 'NONE',  ( -70.43102110461339294, -297.4704528193520332, -337.2710846843863237 ) ) ;
#63277 = CARTESIAN_POINT ( 'NONE',  ( -48.18343439339133027, -254.6182378140498486, -482.3412084739298962 ) ) ;
#63278 = FACE_OUTER_BOUND ( 'NONE', #66449, .T. ) ;
#63279 = CARTESIAN_POINT ( 'NONE',  ( -109.6754384916872880, -283.4082788649991471, -257.2875719025667536 ) ) ;
#63280 = CARTESIAN_POINT ( 'NONE',  ( -31.21115950989508292, -278.1293027334774592, -195.5607684447492716 ) ) ;
#63281 = DIRECTION ( 'NONE',  ( 0.000000000000000000, 0.000000000000000000, 1.000000000000000000 ) ) ;
#63282 = CARTESIAN_POINT ( 'NONE',  ( 34.07968044430916166, -273.6890826553030820, -243.4967522051013020 ) ) ;
#63283 = CARTESIAN_POINT ( 'NONE',  ( -109.1449719022743778, -277.7191543809244649, -284.1452712682504398 ) ) ;
#63284 = CARTESIAN_POINT ( 'NONE',  ( -36.97281847377762887, -296.5675419774173633, -344.0660731612117047 ) ) ;
#63285 = CARTESIAN_POINT ( 'NONE',  ( 39.21963152212485682, -280.5389356741616780, -275.6533220712422008 ) ) ;
#63286 = CARTESIAN_POINT ( 'NONE',  ( 19.02183748762764282, -295.1544676015564619, -317.1217860302025429 ) ) ;
#63287 = CARTESIAN_POINT ( 'NONE',  ( -102.6856361244626754, -297.3443446626416744, -310.1539351794719437 ) ) ;
#63288 = CARTESIAN_POINT ( 'NONE',  ( -39.16620042462899676, -297.8619763040144903, -197.3715125946057469 ) ) ;
#63289 = CARTESIAN_POINT ( 'NONE',  ( -112.3366323615187525, -292.5411176586992497, -271.2333478531952551 ) ) ;
#63290 = CARTESIAN_POINT ( 'NONE',  ( -107.9269797263946629, -285.1125860053548422, -239.4590038071630431 ) ) ;
#63291 = CARTESIAN_POINT ( 'NONE',  ( 17.98476997060967975, -274.4092843453402111, -322.1229493548431719 ) ) ;
#63292 = CARTESIAN_POINT ( 'NONE',  ( 20.57149925643157218, -288.0721919372417119, -321.1260430685949814 ) ) ;
#63293 = CARTESIAN_POINT ( 'NONE',  ( -62.89519318174656348, -281.6978572709766127, -200.1719240426389206 ) ) ;
#63294 = EDGE_CURVE ( 'NONE', #52690, #84307, #32162, .T. ) ;
#63295 = CARTESIAN_POINT ( 'NONE',  ( -103.6935821020003630, -284.0295633711314167, -239.2435851917049092 ) ) ;
#63296 = AXIS2_PLACEMENT_3D ( 'NONE', #8528, #37407, #66316 ) ;
#63297 = CARTESIAN_POINT ( 'NONE',  ( -7.733544505421187765, -286.6639937694782816, -339.2833144905030736 ) ) ;
#63298 = CARTESIAN_POINT ( 'NONE',  ( 26.40820234725076787, -24.66803830325296687, -341.1985388896944755 ) ) ;
#63299 = CARTESIAN_POINT ( 'NONE',  ( -41.32001614970636894, -285.5084000093574446, -197.3954635197628704 ) ) ;
#63300 = CARTESIAN_POINT ( 'NONE',  ( 155.3967522965732257, 18.12362412296499770, 8.741384835539003362 ) ) ;
#63301 = CARTESIAN_POINT ( 'NONE',  ( -41.54423160417324823, -284.0449741152323782, -347.0628703967219622 ) ) ;
#63302 = CARTESIAN_POINT ( 'NONE',  ( -101.4807494939215502, -290.1681617457197717, -228.0875275019855337 ) ) ;
#63303 = CARTESIAN_POINT ( 'NONE',  ( -109.8985848374399126, -279.8545586158737137, -293.8104415641644778 ) ) ;
#63304 = CARTESIAN_POINT ( 'NONE',  ( -100.0516267721233845, -279.2842137432617733, -314.1876324846426769 ) ) ;
#63305 = CARTESIAN_POINT ( 'NONE',  ( 11.30739951486635242, -280.5824260019657572, -215.9344231681857025 ) ) ;
#63306 = CARTESIAN_POINT ( 'NONE',  ( 37.09421864241076605, -277.6755328977007480, -279.9576504304097284 ) ) ;
#63307 = CARTESIAN_POINT ( 'NONE',  ( -56.07028341321783671, -295.2869415952472423, -345.0487352168224788 ) ) ;
#63308 = CARTESIAN_POINT ( 'NONE',  ( -108.5281749271665888, -288.2791341774243961, -292.9896135880377415 ) ) ;
#63309 = CARTESIAN_POINT ( 'NONE',  ( -108.2721384043396995, -295.2283654606972050, -288.9337183668135935 ) ) ;
#63310 = ORIENTED_EDGE ( 'NONE', *, *, #49364, .F. ) ;
#63311 = ORIENTED_EDGE ( 'NONE', *, *, #1954, .T. ) ;
#63312 = CARTESIAN_POINT ( 'NONE',  ( -68.36259239206556515, -285.3830385236655047, -338.0295629498184553 ) ) ;
#63313 = CARTESIAN_POINT ( 'NONE',  ( -107.4784947900113821, -296.4875622568389417, -250.0407459051728267 ) ) ;
#63314 = CARTESIAN_POINT ( 'NONE',  ( -25.08444572857407096, -293.2846291714917015, -194.6560836479893339 ) ) ;
#63315 = CARTESIAN_POINT ( 'NONE',  ( -84.92185123040701455, -284.3806409966656474, -325.8590628898555224 ) ) ;
#63316 = CARTESIAN_POINT ( 'NONE',  ( -18.59579272537223815, -273.3465019727900653, -195.8655987189355869 ) ) ;
#63317 = CARTESIAN_POINT ( 'NONE',  ( -79.54541412990505478, -292.1499025450798968, -206.0155880775002686 ) ) ;
#63318 = CARTESIAN_POINT ( 'NONE',  ( -91.01103837213831582, -283.4393515043308298, -216.8830139408525781 ) ) ;
#63319 = CARTESIAN_POINT ( 'NONE',  ( -108.3492679745883720, -291.2636356959866930, -240.6345372850109925 ) ) ;
#63320 = CARTESIAN_POINT ( 'NONE',  ( 35.57348053269802080, -287.8223972295223803, -265.5810910896143469 ) ) ;
#63321 = DIRECTION ( 'NONE',  ( 0.000000000000000000, 1.000000000000000000, 0.000000000000000000 ) ) ;
#63322 = CARTESIAN_POINT ( 'NONE',  ( 185.4166944662832179, 249.5000000000000568, 23.37680765314684095 ) ) ;
#63323 = CARTESIAN_POINT ( 'NONE',  ( -21.51142200380889946, -109.0746302473303331, -358.9104106151312408 ) ) ;
#63324 = CARTESIAN_POINT ( 'NONE',  ( -35.89277258145762772, -284.5544389133588652, -346.6670282107009484 ) ) ;
#63325 = CARTESIAN_POINT ( 'NONE',  ( 10.59707575819633618, -291.9094976428776818, -330.5268031993606428 ) ) ;
#63326 = ORIENTED_EDGE ( 'NONE', *, *, #63818, .F. ) ;
#63327 = CARTESIAN_POINT ( 'NONE',  ( 1.252402303661884098, -281.4442099325958679, -332.7479206258836939 ) ) ;
#63328 = CARTESIAN_POINT ( 'NONE',  ( -54.13077262984366911, -276.9286405235873190, -345.5414474655901245 ) ) ;
#63329 = CARTESIAN_POINT ( 'NONE',  ( -106.9643909474264518, -280.1943879425912769, -297.7966669535657616 ) ) ;
#63330 = CARTESIAN_POINT ( 'NONE',  ( 181.5289669338484657, 251.5006589549888645, -165.3271292094310070 ) ) ;
#63331 = CARTESIAN_POINT ( 'NONE',  ( 27.36214648389219306, -279.5894814000602651, -229.6168920535202744 ) ) ;
#63332 = CARTESIAN_POINT ( 'NONE',  ( -110.3336466543562580, -282.3699478421068534, -286.0431409718472651 ) ) ;
#63333 = CARTESIAN_POINT ( 'NONE',  ( -97.45882870465375447, -297.6836258872466487, -316.8358946755942611 ) ) ;
#63334 = CARTESIAN_POINT ( 'NONE',  ( 34.54259340403847034, -293.8714098260960554, -257.2287812982983723 ) ) ;
#63335 = ORIENTED_EDGE ( 'NONE', *, *, #19699, .T. ) ;
#63336 = CARTESIAN_POINT ( 'NONE',  ( -104.5051629824076116, -288.8365008741224642, -300.3249704701875089 ) ) ;
#63337 = CARTESIAN_POINT ( 'NONE',  ( 25.98765919217384734, -276.7812294726693381, -314.0733021426435698 ) ) ;
#63338 = CARTESIAN_POINT ( 'NONE',  ( -87.33330285485418187, -273.3318000072327436, -217.0956709510115274 ) ) ;
#63339 = EDGE_LOOP ( 'NONE', ( #3448, #56200, #40420, #39053 ) ) ;
#63340 = CARTESIAN_POINT ( 'NONE',  ( -13.14692271601287032, -273.2796180865968836, -197.5867732229094429 ) ) ;
#63341 = FILL_AREA_STYLE_COLOUR ( '', #64416 ) ;
#63342 = CARTESIAN_POINT ( 'NONE',  ( 154.1779308144228935, 20.65864417925001462, -13.49368544356955901 ) ) ;
#63343 = CARTESIAN_POINT ( 'NONE',  ( 153.9079962421555763, 20.48904911123736383, 11.76949543550875354 ) ) ;
#63344 = CARTESIAN_POINT ( 'NONE',  ( -4.677132606053719499, -283.6910173250950038, -335.9907766988711728 ) ) ;
#63345 = CARTESIAN_POINT ( 'NONE',  ( -5.390743042716076516, -282.2269186829847172, -201.4183130037586977 ) ) ;
#63346 = CARTESIAN_POINT ( 'NONE',  ( -91.84815931963028390, -282.9129456252104546, -319.2927134845928663 ) ) ;
#63347 = CARTESIAN_POINT ( 'NONE',  ( -8.793868743443603364, -282.2900916284773984, -201.8345771032478240 ) ) ;
#63348 = CARTESIAN_POINT ( 'NONE',  ( 24.38471855504198160, -273.4794755556297901, -230.1049757329376462 ) ) ;
#63349 = EDGE_CURVE ( 'NONE', #66913, #4348, #79086, .T. ) ;
#63350 = DIRECTION ( 'NONE',  ( -1.000000000000000000, 0.000000000000000000, 0.000000000000000000 ) ) ;
#63351 = EDGE_CURVE ( 'NONE', #63777, #35022, #33258, .T. ) ;
#63352 = DIRECTION ( 'NONE',  ( 0.000000000000000000, 1.000000000000000000, 0.000000000000000000 ) ) ;
#63353 = CARTESIAN_POINT ( 'NONE',  ( -112.3245841357175294, -279.1446233611774801, -287.1458112260974644 ) ) ;
#63354 = ORIENTED_EDGE ( 'NONE', *, *, #30500, .T. ) ;
#63355 = VERTEX_POINT ( 'NONE', #11950 ) ;
#63356 = DIRECTION ( 'NONE',  ( 0.000000000000000000, 0.7071067811865561215, 0.7071067811865389130 ) ) ;
#63357 = CARTESIAN_POINT ( 'NONE',  ( -32.41085433867187504, -287.9740840468297165, -194.7439814509482403 ) ) ;
#63358 = CARTESIAN_POINT ( 'NONE',  ( 0.0002403523676656696027, -291.7601370730342865, -207.4470400019629892 ) ) ;
#63359 = CARTESIAN_POINT ( 'NONE',  ( -43.18283780114209947, -288.4726747380678944, -347.0370196550280184 ) ) ;
#63360 = CARTESIAN_POINT ( 'NONE',  ( -67.94653331856557088, -283.8846137902221471, -202.9718146672726959 ) ) ;
#63362 = CARTESIAN_POINT ( 'NONE',  ( -56.34712896225217804, -287.5401149642161158, -341.9459940440991659 ) ) ;
#63361 = CARTESIAN_POINT ( 'NONE',  ( -96.22661192625950832, -283.7414727544141329, -226.2256211456656558 ) ) ;
#63363 = VECTOR ( 'NONE', #27610, 1000.000000000000000 ) ;
#63364 = CARTESIAN_POINT ( 'NONE',  ( -103.3631639362055097, -285.3240595082319260, -302.5448580271842047 ) ) ;
#63365 = CARTESIAN_POINT ( 'NONE',  ( 34.95083735305195205, -273.8093906626360763, -290.3786626950142704 ) ) ;
#63366 = CARTESIAN_POINT ( 'NONE',  ( 17.78695433068271115, -285.2244864174737700, -217.6801330819846783 ) ) ;
#63367 = CARTESIAN_POINT ( 'NONE',  ( -90.24334274061806127, -299.3040049424387234, -217.1970619252629433 ) ) ;
#63368 = CARTESIAN_POINT ( 'NONE',  ( -84.34615385057271908, -283.4068543128089459, -211.7044069113624403 ) ) ;
#63369 = CARTESIAN_POINT ( 'NONE',  ( 9.417588190318248564, -281.6543325051471243, -213.9303381918627451 ) ) ;
#63370 = CARTESIAN_POINT ( 'NONE',  ( 34.21057718990975616, -289.8489573500260121, -293.3893623157172783 ) ) ;
#63371 = CARTESIAN_POINT ( 'NONE',  ( 175.2296996224750103, 140.2072866198470251, 0.000000000000000000 ) ) ;
#63372 = LINE ( 'NONE', #53900, #6556 ) ;
#63373 = CARTESIAN_POINT ( 'NONE',  ( -1.369764346864409177, -296.4991389612242187, -336.8237069303060593 ) ) ;
#63374 = CARTESIAN_POINT ( 'NONE',  ( -36.97363010064713507, -278.0566052562255663, -195.3620168015945069 ) ) ;
#63375 = CARTESIAN_POINT ( 'NONE',  ( -112.1079507480223185, -289.5264802661381509, -288.1421918639035766 ) ) ;
#63376 = CARTESIAN_POINT ( 'NONE',  ( 1.979022500949452867, -292.9166040905300861, -332.8741832534555556 ) ) ;
#63377 = CARTESIAN_POINT ( 'NONE',  ( -6.547601964989245182, -279.1500236574109977, -203.6168238788341682 ) ) ;
#63378 = CARTESIAN_POINT ( 'NONE',  ( -41.92126853163554756, -296.1334074908899083, -196.2673055922932690 ) ) ;
#63379 = CARTESIAN_POINT ( 'NONE',  ( 17.09224104264845678, -294.1638216175812772, -220.9084719378967634 ) ) ;
#63380 = CARTESIAN_POINT ( 'NONE',  ( 21.27581636871892101, -289.4090924074130839, -223.5744983911110353 ) ) ;
#63381 = CARTESIAN_POINT ( 'NONE',  ( -97.67376968805652382, -295.6616800873560464, -223.6201368145549964 ) ) ;
#63382 = CARTESIAN_POINT ( 'NONE',  ( -31.79106778512614540, -290.5812147842836453, -344.0032664663007154 ) ) ;
#63383 = CARTESIAN_POINT ( 'NONE',  ( 36.10892248153815842, -291.5444706346461885, -250.8434499350653653 ) ) ;
#63384 = CARTESIAN_POINT ( 'NONE',  ( -109.2344962802145147, -291.7711371976793089, -286.1295237892260843 ) ) ;
#63385 = CARTESIAN_POINT ( 'NONE',  ( 222.8344101925596306, 3.000000000000000000, 10.00000000000000000 ) ) ;
#63386 = CARTESIAN_POINT ( 'NONE',  ( -88.04986210452346995, -292.1236792364506982, -217.5532146111113434 ) ) ;
#63387 = DIRECTION ( 'NONE',  ( -0.000000000000000000, -0.000000000000000000, -1.000000000000000000 ) ) ;
#63388 = EDGE_CURVE ( 'NONE', #77042, #12355, #32799, .T. ) ;
#63389 = CARTESIAN_POINT ( 'NONE',  ( -76.97702002071703475, -292.7390859550529285, -204.7480474552395151 ) ) ;
#63391 = CARTESIAN_POINT ( 'NONE',  ( 35.62132981578164959, -293.5215081312270513, -268.0381325303991957 ) ) ;
#63390 = CARTESIAN_POINT ( 'NONE',  ( 9.813803242897584767, -278.7174007043979032, -211.5169668397512908 ) ) ;
#63392 = CARTESIAN_POINT ( 'NONE',  ( -14.22775861683004273, -280.3437030819081315, -196.8562851808001142 ) ) ;
#63393 = CARTESIAN_POINT ( 'NONE',  ( -37.31852028506730079, -282.7185539428414245, -347.3530322087046898 ) ) ;
#63394 = CARTESIAN_POINT ( 'NONE',  ( 21.79084572217033156, -286.1823452680244486, -316.2443724027060625 ) ) ;
#63395 = CARTESIAN_POINT ( 'NONE',  ( 25.15778577855219567, -280.2378175147488832, -310.5140267591602310 ) ) ;
#63396 = CARTESIAN_POINT ( 'NONE',  ( -40.70071967932008761, -284.0098745136969569, -195.3855330098118372 ) ) ;
#63397 = CARTESIAN_POINT ( 'NONE',  ( -186.9122233887894140, -89.54582641780471874, -22.50000000000000000 ) ) ;
#63398 = CARTESIAN_POINT ( 'NONE',  ( 33.68621961589681746, -279.6736475377336433, -242.3287744070736949 ) ) ;
#63399 = CARTESIAN_POINT ( 'NONE',  ( 33.57884248879058475, -286.0985502209837819, -241.0372377868471858 ) ) ;
#63400 = DIRECTION ( 'NONE',  ( 0.000000000000000000, 0.000000000000000000, 1.000000000000000000 ) ) ;
#63401 = CARTESIAN_POINT ( 'NONE',  ( 32.30170494877508247, -295.4754336087215734, -294.9322122211624446 ) ) ;
#63402 = CARTESIAN_POINT ( 'NONE',  ( -29.91435360129797516, -275.5696947930615011, -194.3121810011747357 ) ) ;
#63403 = CARTESIAN_POINT ( 'NONE',  ( -27.02271926388235102, -276.5840454100101056, -342.6494719591161697 ) ) ;
#63404 = CARTESIAN_POINT ( 'NONE',  ( -103.2169436489691208, -291.2403280469488323, -230.3903768987567560 ) ) ;
#63405 = CARTESIAN_POINT ( 'NONE',  ( -55.38250664504730025, -281.3623541608585583, -343.7357968260704411 ) ) ;
#63406 = EDGE_CURVE ( 'NONE', #84959, #3069, #85078, .T. ) ;
#63407 = CARTESIAN_POINT ( 'NONE',  ( -55.05771012719652191, -290.8774180103706612, -199.3009221124509907 ) ) ;
#63408 = CARTESIAN_POINT ( 'NONE',  ( -93.18004292028670932, -293.8543926375297133, -320.4510112440859757 ) ) ;
#63409 = ORIENTED_EDGE ( 'NONE', *, *, #80190, .T. ) ;
#63410 = CARTESIAN_POINT ( 'NONE',  ( 151.9308040601938217, 19.99432900747112285, 6.268121358094561835 ) ) ;
#63411 = CARTESIAN_POINT ( 'NONE',  ( 26.29123287527274044, -292.5675825573036377, -234.3574085703215815 ) ) ;
#63412 = CARTESIAN_POINT ( 'NONE',  ( 219.8344101925596021, 35.72494958537217968, 10.00000000000000000 ) ) ;
#63413 = CARTESIAN_POINT ( 'NONE',  ( -37.30987171927208834, -271.5523547857346784, -200.3611179825600459 ) ) ;
#63414 = CARTESIAN_POINT ( 'NONE',  ( -112.9053835206017595, -295.7805825568702858, -256.8352181784918002 ) ) ;
#63415 = CARTESIAN_POINT ( 'NONE',  ( 36.78126115972154508, -279.4915616319282776, -254.6116388800126344 ) ) ;
#63416 = CARTESIAN_POINT ( 'NONE',  ( -100.5982566196063033, -286.4395172795497615, -227.2337231558821600 ) ) ;
#63417 = CARTESIAN_POINT ( 'NONE',  ( 11.13564330270977365, -286.5788372088599658, -215.7134671445068079 ) ) ;
#63418 = CARTESIAN_POINT ( 'NONE',  ( -3.532291924242987324, -278.1174992233793546, -335.8411276878217109 ) ) ;
#63419 = CARTESIAN_POINT ( 'NONE',  ( -110.9897807612209277, -294.4154136088573068, -282.5187091491648630 ) ) ;
#63420 = CARTESIAN_POINT ( 'NONE',  ( -72.58766957388525043, -297.2856104660420442, -335.4578052676396851 ) ) ;
#63421 = CARTESIAN_POINT ( 'NONE',  ( -109.2733383077971041, -277.5393716156920618, -255.7045796643695894 ) ) ;
#63422 = VERTEX_POINT ( 'NONE', #55522 ) ;
#63423 = CARTESIAN_POINT ( 'NONE',  ( 194.7288575836260804, 39.67451392790587050, 14.01013636219982672 ) ) ;
#63424 = CARTESIAN_POINT ( 'NONE',  ( -99.90189105279193882, -296.8134374587357343, -225.5061650450461457 ) ) ;
#63425 = CARTESIAN_POINT ( 'NONE',  ( 23.94916730868969523, -290.0495163960730451, -312.6298241657378867 ) ) ;
#63426 = CARTESIAN_POINT ( 'NONE',  ( 200.4551663812866025, 64.49084098423909950, -2.633798379906725273 ) ) ;
#63427 = CARTESIAN_POINT ( 'NONE',  ( -3.311537114643715807, -289.2420469840506598, -335.1152577459354802 ) ) ;
#63428 = ORIENTED_EDGE ( 'NONE', *, *, #19673, .T. ) ;
#63429 = CARTESIAN_POINT ( 'NONE',  ( -68.56580941317044164, -278.7105403515757303, -200.2192135571431777 ) ) ;
#63430 = CARTESIAN_POINT ( 'NONE',  ( -85.15952346178548282, -298.0627449385340242, -210.1384598056344828 ) ) ;
#63431 = CARTESIAN_POINT ( 'NONE',  ( -103.5193828768155129, -289.1777917244504579, -233.4718270675326153 ) ) ;
#63432 = VECTOR ( 'NONE', #51242, 1000.000000000000114 ) ;
#63433 = CARTESIAN_POINT ( 'NONE',  ( -95.56272344187836154, -296.2049341759523031, -320.7203945448667923 ) ) ;
#63434 = CARTESIAN_POINT ( 'NONE',  ( 17.09916428460538285, -294.5815578933360257, -319.0449458822104702 ) ) ;
#63435 = DIRECTION ( 'NONE',  ( 0.000000000000000000, 0.000000000000000000, -1.000000000000000000 ) ) ;
#63436 = CARTESIAN_POINT ( 'NONE',  ( 200.3186454232214828, 250.5000000000000568, -3.421094783296261710 ) ) ;
#63437 = CARTESIAN_POINT ( 'NONE',  ( 29.76228481224210043, -289.5477299558951358, -306.8002171729538077 ) ) ;
#63438 = CARTESIAN_POINT ( 'NONE',  ( -55.63300648810263738, -276.3376638359844719, -190.3683826091709363 ) ) ;
#63439 = CARTESIAN_POINT ( 'NONE',  ( 39.53908953109786495, -280.8595259618310251, -267.0700248326328961 ) ) ;
#63440 = CARTESIAN_POINT ( 'NONE',  ( -99.64725244132328896, -287.1135753172270029, -228.9117925661760182 ) ) ;
#63441 = CARTESIAN_POINT ( 'NONE',  ( -2.475450634261491256, -285.0789096323716194, -202.3541908783233794 ) ) ;
#63442 = CARTESIAN_POINT ( 'NONE',  ( -99.48851566804796676, -289.1904288329418478, -229.2908617249132703 ) ) ;
#63443 = CARTESIAN_POINT ( 'NONE',  ( -12.25249928554282342, -278.5897376470998097, -341.9062764110363446 ) ) ;
#63444 = ORIENTED_EDGE ( 'NONE', *, *, #1761, .F. ) ;
#63446 = CARTESIAN_POINT ( 'NONE',  ( -36.99953479745897766, -279.4051341648615789, -197.2599853547728515 ) ) ;
#63445 = CARTESIAN_POINT ( 'NONE',  ( -80.81938008473255763, -277.6611140641101088, -329.0014739295272079 ) ) ;
#63447 = CARTESIAN_POINT ( 'NONE',  ( 32.74287989804032861, -277.0308448625507936, -301.5002276593469333 ) ) ;
#63448 = CARTESIAN_POINT ( 'NONE',  ( -111.7929223867247401, -277.1197530511220180, -288.4445316558101240 ) ) ;
#63449 = CARTESIAN_POINT ( 'NONE',  ( -113.3917889056992436, -270.8501404346486652, -270.3394472961810493 ) ) ;
#63450 = CARTESIAN_POINT ( 'NONE',  ( -66.15007414649615214, -274.6254463306890443, -199.1929472639433243 ) ) ;
#63451 = CARTESIAN_POINT ( 'NONE',  ( -59.99088444011947274, -299.1896602990232736, -197.3291652706923003 ) ) ;
#63452 = CARTESIAN_POINT ( 'NONE',  ( -85.33152481854864391, -293.9090924074130839, -210.2361428286349110 ) ) ;
#63453 = ORIENTED_EDGE ( 'NONE', *, *, #47800, .F. ) ;
#63454 = CARTESIAN_POINT ( 'NONE',  ( 82.63349580044121012, -300.7641721541951370, -193.1664502239968897 ) ) ;
#63455 = CARTESIAN_POINT ( 'NONE',  ( 14.31088586477970281, -289.3845567966654926, -322.3826177067371077 ) ) ;
#63456 = CARTESIAN_POINT ( 'NONE',  ( 34.87882036094710969, -289.0091572631905592, -246.5673664989975862 ) ) ;
#63457 = CARTESIAN_POINT ( 'NONE',  ( -26.46790819163601327, -288.2588489968362637, -342.7009185497882413 ) ) ;
#63458 = CARTESIAN_POINT ( 'NONE',  ( -97.12854247041207145, -283.4095930436573667, -318.8076470488693985 ) ) ;
#63459 = CARTESIAN_POINT ( 'NONE',  ( 29.70794543208570460, -279.5391046955959382, -239.4037654485818223 ) ) ;
#63460 = CARTESIAN_POINT ( 'NONE',  ( -92.45388373561425510, -287.1136277388338272, -220.5511347061224114 ) ) ;
#63461 = CARTESIAN_POINT ( 'NONE',  ( 9.734180712776103306, -279.1933545875294840, -213.5974117790156583 ) ) ;
#63462 = EDGE_CURVE ( 'NONE', #67590, #67510, #69252, .T. ) ;
#63463 = CARTESIAN_POINT ( 'NONE',  ( -108.6464988376608289, -279.6333825968851556, -288.2137677879306921 ) ) ;
#63464 = CARTESIAN_POINT ( 'NONE',  ( 9.708459146132552675, -276.8761381028799065, -326.2562962516623770 ) ) ;
#63465 = CARTESIAN_POINT ( 'NONE',  ( -5.804062505380270132, -287.4415526140517159, -340.1707601035203083 ) ) ;
#63466 = CARTESIAN_POINT ( 'NONE',  ( 17.71772245008054725, -283.0920284130585287, -324.0339728135249402 ) ) ;
#63467 = CARTESIAN_POINT ( 'NONE',  ( -112.4636465300569910, -284.8364758898206333, -286.9809877877719373 ) ) ;
#63468 = CARTESIAN_POINT ( 'NONE',  ( 7.795626209133624585, -282.5828587568330477, -327.7983346106207136 ) ) ;
#63469 = ORIENTED_EDGE ( 'NONE', *, *, #29709, .F. ) ;
#63470 = ORIENTED_EDGE ( 'NONE', *, *, #20244, .T. ) ;
#63471 = PLANE ( 'NONE',  #65591 ) ;
#63472 = CARTESIAN_POINT ( 'NONE',  ( -104.9133894839825416, -292.8622579405289343, -235.9762545252293080 ) ) ;
#63473 = CARTESIAN_POINT ( 'NONE',  ( -3.524145681270232977, -291.1740041986148526, -201.7196266523338011 ) ) ;
#63474 = CARTESIAN_POINT ( 'NONE',  ( 35.93406110213977911, -274.6271962164046840, -271.6008724313213634 ) ) ;
#63475 = CARTESIAN_POINT ( 'NONE',  ( 38.71450315925660846, -293.0428461013116248, -281.7086608053122632 ) ) ;
#63476 = ADVANCED_FACE ( 'NONE', ( #41755 ), #19986, .T. ) ;
#63477 = CARTESIAN_POINT ( 'NONE',  ( -66.62215398130057054, -287.9225393099275152, -338.0422975230064253 ) ) ;
#63478 = CARTESIAN_POINT ( 'NONE',  ( 34.29456961880003263, -291.5497233487307653, -251.7541603490146542 ) ) ;
#63479 = CARTESIAN_POINT ( 'NONE',  ( -58.79058938073196572, -290.5407935632852627, -340.6073362785776339 ) ) ;
#63480 = DIRECTION ( 'NONE',  ( 1.000000000000000000, 0.000000000000000000, 0.000000000000000000 ) ) ;
#63481 = CARTESIAN_POINT ( 'NONE',  ( -105.8927239133560647, -292.1521867690851195, -300.9150203858601458 ) ) ;
#63482 = CARTESIAN_POINT ( 'NONE',  ( -87.40891630622529362, -289.3554763264990584, -214.2959568920143738 ) ) ;
#63483 = CARTESIAN_POINT ( 'NONE',  ( -8.935721882019969087, -294.4238225140535405, -200.9348435521304737 ) ) ;
#63484 = CARTESIAN_POINT ( 'NONE',  ( -35.94094786127367769, -287.0114029018113229, -197.1392200154339491 ) ) ;
#63485 = CARTESIAN_POINT ( 'NONE',  ( 32.74396599752798664, -295.1980916628122600, -243.0507376597385019 ) ) ;
#63486 = DIRECTION ( 'NONE',  ( 0.000000000000000000, 0.000000000000000000, -1.000000000000000000 ) ) ;
#63487 = CARTESIAN_POINT ( 'NONE',  ( -43.54160339317392214, -248.0334966641272842, -430.6442049081568939 ) ) ;
#63488 = CARTESIAN_POINT ( 'NONE',  ( 37.74377208733400835, -277.6134522826981765, -276.7312563652594690 ) ) ;
#63489 = CARTESIAN_POINT ( 'NONE',  ( -107.6211904154694992, -296.1479739792430905, -239.1659288299988475 ) ) ;
#63490 = CARTESIAN_POINT ( 'NONE',  ( 14.21842321400900389, -273.0285999412687374, -217.2618930054013049 ) ) ;
#63491 = CARTESIAN_POINT ( 'NONE',  ( -111.7199265676652402, -276.5927671492967193, -273.3932173955231519 ) ) ;
#63492 = CARTESIAN_POINT ( 'NONE',  ( -69.67965915161632040, -274.8216527840484673, -204.4719161937341880 ) ) ;
#63493 = CARTESIAN_POINT ( 'NONE',  ( -110.8291434654652505, -297.9267994205091554, -274.2303023187665758 ) ) ;
#63494 = SPHERICAL_SURFACE ( 'NONE', #55082, 1.000000000000000000 ) ;
#63495 = CARTESIAN_POINT ( 'NONE',  ( -60.57684897720904615, -298.5458866157442230, -200.9336885025287529 ) ) ;
#63496 = VECTOR ( 'NONE', #54499, 1000.000000000000000 ) ;
#63497 = CARTESIAN_POINT ( 'NONE',  ( 209.6315158418980502, 36.17082498069705565, 14.26380412667038655 ) ) ;
#63499 = CARTESIAN_POINT ( 'NONE',  ( -107.9395334423564066, -272.6330337193019204, -251.5945820704199605 ) ) ;
#63498 = CARTESIAN_POINT ( 'NONE',  ( 20.83672661848881802, -284.9148030687157416, -222.4687650643165853 ) ) ;
#63500 = CARTESIAN_POINT ( 'NONE',  ( -46.50549779701704267, -285.9388967164653081, -193.9083560162137019 ) ) ;
#63501 = AXIS2_PLACEMENT_3D ( 'NONE', #50886, #41422, #45148 ) ;
#63502 = CARTESIAN_POINT ( 'NONE',  ( 5.542024480287892629, -288.1552058773006593, -334.2886586451904236 ) ) ;
#63503 = CARTESIAN_POINT ( 'NONE',  ( -96.95741075061937408, -297.9033412845108728, -316.4520482590865527 ) ) ;
#63504 = CARTESIAN_POINT ( 'NONE',  ( 21.11019634088313879, -292.1961249530592681, -317.1084472769126705 ) ) ;
#63505 = EDGE_CURVE ( 'NONE', #75656, #90187, #68178, .T. ) ;
#63506 = CARTESIAN_POINT ( 'NONE',  ( 17.11590126150796465, -280.0016126334721775, -216.0783035972525283 ) ) ;
#63507 = CARTESIAN_POINT ( 'NONE',  ( -69.85430415644619018, -295.1237833571632905, -202.7746430608542312 ) ) ;
#63508 = CYLINDRICAL_SURFACE ( 'NONE', #1542, 5.000000000000000888 ) ;
#63509 = CARTESIAN_POINT ( 'NONE',  ( -72.56281592650945811, -288.3244551162549101, -334.7552443248590635 ) ) ;
#63510 = CARTESIAN_POINT ( 'NONE',  ( 115.2448031289451222, -299.5541904835127980, -192.4725777504219764 ) ) ;
#63511 = CARTESIAN_POINT ( 'NONE',  ( 4.715632006333960291, -286.4845634660563860, -332.5218879349656618 ) ) ;
#63512 = CARTESIAN_POINT ( 'NONE',  ( -96.85262479312437733, -274.6761594956954013, -226.8118680660714688 ) ) ;
#63513 = CARTESIAN_POINT ( 'NONE',  ( -28.31278078357101435, -281.5897110582178584, -194.4324480135501005 ) ) ;
#63515 = CARTESIAN_POINT ( 'NONE',  ( -1.252006348918950795, -282.5589870264482215, -333.8160941698243960 ) ) ;
#63514 = CARTESIAN_POINT ( 'NONE',  ( -111.9692483712619122, -294.7069538468271048, -259.8211879118365459 ) ) ;
#63516 = CARTESIAN_POINT ( 'NONE',  ( -111.9681222818362158, -296.4808446223850069, -289.3852961257915695 ) ) ;
#63517 = CARTESIAN_POINT ( 'NONE',  ( -110.4733397539654760, -274.0846547869002165, -262.1673275134239702 ) ) ;
#63518 = CARTESIAN_POINT ( 'NONE',  ( 37.14160967504894728, -285.4690400418269860, -257.5745972863552993 ) ) ;
#63519 = CARTESIAN_POINT ( 'NONE',  ( 17.67526877177949984, -282.8394078387713080, -219.3892259008433996 ) ) ;
#63520 = CARTESIAN_POINT ( 'NONE',  ( -110.4962142403251590, -271.5445183617832754, -264.8766913285733153 ) ) ;
#63521 = ORIENTED_EDGE ( 'NONE', *, *, #80099, .T. ) ;
#63522 = FACE_OUTER_BOUND ( 'NONE', #30589, .T. ) ;
#63523 = CARTESIAN_POINT ( 'NONE',  ( -88.02761849207243472, -285.7448040222273562, -325.2294788307875137 ) ) ;
#63524 = FACE_OUTER_BOUND ( 'NONE', #64615, .T. ) ;
#63525 = CARTESIAN_POINT ( 'NONE',  ( -85.33152481854864391, -293.1952119285920162, -330.4860931364850671 ) ) ;
#63526 = CARTESIAN_POINT ( 'NONE',  ( -6.648613222671792222, -275.8565030084237719, -340.8174700780544981 ) ) ;
#63527 = CARTESIAN_POINT ( 'NONE',  ( 2.242282885843235096, -292.4316107313379121, -208.9652089898891916 ) ) ;
#63528 = CARTESIAN_POINT ( 'NONE',  ( -13.28491113351632968, -284.2542170530506382, -340.0713828620420713 ) ) ;
#63529 = CARTESIAN_POINT ( 'NONE',  ( 35.90264312936438529, -277.2755653046600059, -279.8087547624083413 ) ) ;
#63530 = CARTESIAN_POINT ( 'NONE',  ( -87.91783460465950384, -285.1679985562252000, -327.7088054837951177 ) ) ;
#63531 = CARTESIAN_POINT ( 'NONE',  ( -8.351452149322609486, -281.4588251740967735, -337.7903106794484529 ) ) ;
#63532 = CARTESIAN_POINT ( 'NONE',  ( -98.03888760067734154, -281.1523823497943795, -226.3060151704531506 ) ) ;
#63533 = CARTESIAN_POINT ( 'NONE',  ( 9.508660332924277370, -274.8432997001667104, -209.2542957025698627 ) ) ;
#63534 = CARTESIAN_POINT ( 'NONE',  ( 39.62331646840029720, -275.4315580328646433, -274.0460811728977433 ) ) ;
#63535 = ADVANCED_FACE ( 'NONE', ( #90519 ), #83573, .T. ) ;
#63536 = CARTESIAN_POINT ( 'NONE',  ( -76.39306964733597738, -297.4984922509403873, -333.7955251545253645 ) ) ;
#63537 = CARTESIAN_POINT ( 'NONE',  ( 175.2296996224749250, 275.5000000000000568, -24.99999999999999289 ) ) ;
#63538 = DIRECTION ( 'NONE',  ( -0.000000000000000000, -1.000000000000000000, -0.000000000000000000 ) ) ;
#63539 = CARTESIAN_POINT ( 'NONE',  ( -67.75248974617781528, -293.5865982181844061, -339.7548450588759579 ) ) ;
#63540 = CARTESIAN_POINT ( 'NONE',  ( 35.44011158421625396, -274.9683292407249269, -263.4211312380294316 ) ) ;
#63541 = CARTESIAN_POINT ( 'NONE',  ( 38.91471928111801759, -295.1072153258937760, -273.1299173373506051 ) ) ;
#63542 = CARTESIAN_POINT ( 'NONE',  ( 17.28918780799027743, -295.4989021673561638, -324.1345762994708366 ) ) ;
#63543 = CARTESIAN_POINT ( 'NONE',  ( -92.11809222832076216, -293.2675844129392431, -219.3561340634631733 ) ) ;
#63544 = CARTESIAN_POINT ( 'NONE',  ( -111.7292988090824224, -276.4411255325180719, -278.9762012215477966 ) ) ;
#63545 = CARTESIAN_POINT ( 'NONE',  ( -105.7753005641902888, -280.8582068985479623, -241.0668092086709464 ) ) ;
#63546 = CARTESIAN_POINT ( 'NONE',  ( -99.95756674138739584, -294.0845780357494164, -310.7118647824431150 ) ) ;
#63547 = CARTESIAN_POINT ( 'NONE',  ( -100.3780759615394516, -285.8492128994921018, -312.4875889980253305 ) ) ;
#63548 = CARTESIAN_POINT ( 'NONE',  ( -110.6178915127884608, -283.5013314358732259, -268.1643365109780461 ) ) ;
#63549 = CARTESIAN_POINT ( 'NONE',  ( 187.0472849604405781, 261.5718128686381760, -152.6093149707159569 ) ) ;
#63550 = ORIENTED_EDGE ( 'NONE', *, *, #73502, .F. ) ;
#63551 = CARTESIAN_POINT ( 'NONE',  ( -110.3401169112278808, -284.1756953226254154, -273.6348520302908014 ) ) ;
#63552 = ORIENTED_EDGE ( 'NONE', *, *, #75701, .T. ) ;
#63553 = CARTESIAN_POINT ( 'NONE',  ( 34.03167829427027868, -282.2730222910362272, -242.1567798322602130 ) ) ;
#63554 = CARTESIAN_POINT ( 'NONE',  ( -112.6051703620723003, -283.5297988000982059, -255.8229296987388182 ) ) ;
#63555 = CARTESIAN_POINT ( 'NONE',  ( -111.1144529447006448, -279.7602976436205040, -249.1384613371601802 ) ) ;
#63556 = EDGE_CURVE ( 'NONE', #56922, #37982, #19066, .T. ) ;
#63557 = CARTESIAN_POINT ( 'NONE',  ( -53.96121231241312444, -278.7817454314504175, -344.8900885684331001 ) ) ;
#63558 = CARTESIAN_POINT ( 'NONE',  ( -77.44644497616656054, -280.1808219814556082, -204.6875642340633874 ) ) ;
#63559 = CIRCLE ( 'NONE', #43843, 0.5000000000000009992 ) ;
#63560 = CARTESIAN_POINT ( 'NONE',  ( -105.5795714935544112, -276.2666405000204009, -254.7536222014695397 ) ) ;
#63561 = CARTESIAN_POINT ( 'NONE',  ( -47.24013756723644519, -155.4399423264042071, -365.2501074656324818 ) ) ;
#63562 = ORIENTED_EDGE ( 'NONE', *, *, #25879, .T. ) ;
#63563 = CARTESIAN_POINT ( 'NONE',  ( 14.75516282931950052, -276.7882957715298176, -216.6401230650349419 ) ) ;
#63564 = CARTESIAN_POINT ( 'NONE',  ( -31.81167078611810695, -123.9956632658876146, -363.9854646715294280 ) ) ;
#63565 = CIRCLE ( 'NONE', #30280, 1.000000000000006439 ) ;
#63566 = CARTESIAN_POINT ( 'NONE',  ( -70.44758232897444827, -277.6336853112175049, -203.4451894397258513 ) ) ;
#63567 = CARTESIAN_POINT ( 'NONE',  ( 36.80020992900830379, -295.5239366589992187, -287.0617739621884539 ) ) ;
#63568 = CARTESIAN_POINT ( 'NONE',  ( 10.35176132541909766, -293.7216967948251636, -325.7617172793203508 ) ) ;
#63569 = CARTESIAN_POINT ( 'NONE',  ( -89.45440923371522501, -289.2709095125413796, -326.9631714149327308 ) ) ;
#63570 = DIRECTION ( 'NONE',  ( -1.000000000000000000, 0.000000000000000000, 0.000000000000000000 ) ) ;
#63572 = CARTESIAN_POINT ( 'NONE',  ( -79.75254850530826900, -283.8683700503522118, -209.9017007766233291 ) ) ;
#63571 = CARTESIAN_POINT ( 'NONE',  ( 30.37173277726344267, -292.5871970033860521, -305.7658817230463342 ) ) ;
#63573 = CARTESIAN_POINT ( 'NONE',  ( -38.94765747131378930, -293.8922084227853588, -196.1432873476060195 ) ) ;
#63574 = CARTESIAN_POINT ( 'NONE',  ( 2.841125475369175923, -285.0821094715004165, -208.5869463730107327 ) ) ;
#63575 = CARTESIAN_POINT ( 'NONE',  ( -102.6844519964159588, -286.3215390767849726, -236.7223270575540823 ) ) ;
#63576 = ORIENTED_EDGE ( 'NONE', *, *, #51225, .F. ) ;
#63577 = CARTESIAN_POINT ( 'NONE',  ( -111.0097469576136575, -291.7649438751481625, -248.7778121772562372 ) ) ;
#63578 = CARTESIAN_POINT ( 'NONE',  ( 35.20166298559555429, -282.1644260867324761, -279.4596837621922418 ) ) ;
#63579 = CARTESIAN_POINT ( 'NONE',  ( -8.551585269441503101, -293.4786751454732325, -341.4041887609004675 ) ) ;
#63580 = CARTESIAN_POINT ( 'NONE',  ( -69.28083974303591219, -290.2645762096418025, -340.2614901387378836 ) ) ;
#63581 = CARTESIAN_POINT ( 'NONE',  ( -87.33968151546935133, -290.2197185975394405, -328.9095370581140969 ) ) ;
#63582 = CARTESIAN_POINT ( 'NONE',  ( 34.01112987939171717, -287.9229723422158145, -285.8396637892997205 ) ) ;
#63583 = VERTEX_POINT ( 'NONE', #40799 ) ;
#63584 = LINE ( 'NONE', #92409, #477 ) ;
#63585 = CARTESIAN_POINT ( 'NONE',  ( -112.3817357046219740, -298.5466424332565225, -259.8124665686835328 ) ) ;
#63586 = CARTESIAN_POINT ( 'NONE',  ( -3.663580564556140118, -297.1503186028055552, -193.8616065276860070 ) ) ;
#63587 = EDGE_CURVE ( 'NONE', #48695, #13368, #17090, .T. ) ;
#63588 = CARTESIAN_POINT ( 'NONE',  ( 13.50706971362714448, -279.8438260783021860, -217.5854926527914870 ) ) ;
#63589 = CARTESIAN_POINT ( 'NONE',  ( -32.68006188642020504, -273.6170480296686947, -193.5508683744300527 ) ) ;
#63590 = CARTESIAN_POINT ( 'NONE',  ( -84.94055180905242253, -294.2022650195208371, -326.6869733843120116 ) ) ;
#63591 = CARTESIAN_POINT ( 'NONE',  ( 26.13350792768045139, -276.7946931963322186, -232.1978456819760197 ) ) ;
#63592 = CARTESIAN_POINT ( 'NONE',  ( -35.76641730591592250, -296.3119934201538967, -196.3482578600380748 ) ) ;
#63593 = CARTESIAN_POINT ( 'NONE',  ( -47.83471425619570994, -296.3935046237718893, -343.0558249699116686 ) ) ;
#63594 = CARTESIAN_POINT ( 'NONE',  ( -2.986777450175233994, -295.6665421648442020, -335.1219499884488187 ) ) ;
#63595 = CARTESIAN_POINT ( 'NONE',  ( 0.000000000000000000, 3.000000000000000000, -10.00000000000000000 ) ) ;
#63596 = CARTESIAN_POINT ( 'NONE',  ( -19.45508608312137966, -296.4260678229265977, -344.4864124382992827 ) ) ;
#63597 = CARTESIAN_POINT ( 'NONE',  ( -96.83929914791860938, -293.9239326507102987, -316.2965524691065298 ) ) ;
#63598 = CARTESIAN_POINT ( 'NONE',  ( -34.86212271287116238, -292.7355360786215215, -197.3012496258579347 ) ) ;
#63599 = CARTESIAN_POINT ( 'NONE',  ( -44.03889511919753375, -274.7724858189113775, -193.7618148407555054 ) ) ;
#63600 = CARTESIAN_POINT ( 'NONE',  ( -97.23039852896205559, -289.7206124650849688, -227.5114321755981166 ) ) ;
#63601 = CARTESIAN_POINT ( 'NONE',  ( -88.72148850990205915, -275.3316383894008368, -215.6537546093924789 ) ) ;
#63602 = CARTESIAN_POINT ( 'NONE',  ( -113.4843341027583818, -273.1871977505134055, -258.9600484469769412 ) ) ;
#63603 = CARTESIAN_POINT ( 'NONE',  ( -96.42302294119896544, -296.2847928861135642, -313.2949832391473137 ) ) ;
#63604 = CARTESIAN_POINT ( 'NONE',  ( -81.30024790682465152, -281.4376555876295924, -209.1561110198740039 ) ) ;
#63605 = CARTESIAN_POINT ( 'NONE',  ( 1.140507894786421783, -279.2391311490027874, -204.1765336916885758 ) ) ;
#63606 = CARTESIAN_POINT ( 'NONE',  ( -38.55168491383747664, -276.4155416398226635, -347.2496653994394364 ) ) ;
#63607 = CARTESIAN_POINT ( 'NONE',  ( 8.086118574069120157, -279.0611655433428950, -209.1174659537655316 ) ) ;
#63608 = CARTESIAN_POINT ( 'NONE',  ( 12.44691076144868269, -280.3607973189054974, -326.7431004749354884 ) ) ;
#63609 = CARTESIAN_POINT ( 'NONE',  ( -85.68368174464589515, -271.9426698922451351, -214.8096350125262006 ) ) ;
#63610 = CARTESIAN_POINT ( 'NONE',  ( -98.97871779457889829, -279.9717813711176859, -313.1798294181111828 ) ) ;
#63611 = CARTESIAN_POINT ( 'NONE',  ( 140.6539576904058606, 275.5000000000000568, -12.00000000000000000 ) ) ;
#63612 = CARTESIAN_POINT ( 'NONE',  ( 153.2628468892384603, 20.37991841447901820, 11.93555113919331312 ) ) ;
#63613 = CARTESIAN_POINT ( 'NONE',  ( 7.270731545534527385, -296.8432417712202778, -194.3875932721223876 ) ) ;
#63614 = CARTESIAN_POINT ( 'NONE',  ( 35.49930013023998754, -291.3247551984768506, -251.0085373285693038 ) ) ;
#63615 = CARTESIAN_POINT ( 'NONE',  ( -56.18878721987374547, -291.8159877864858345, -195.6483685492484597 ) ) ;
#63616 = CARTESIAN_POINT ( 'NONE',  ( -6.024810851595579386, -278.6416711573056659, -338.6932544657472590 ) ) ;
#63617 = CARTESIAN_POINT ( 'NONE',  ( 24.72128344378412024, -272.9817730926432091, -228.2288473141829570 ) ) ;
#63618 = CARTESIAN_POINT ( 'NONE',  ( 139.6539576904058606, 275.0000000000000568, -10.49999999999999822 ) ) ;
#63619 = CARTESIAN_POINT ( 'NONE',  ( -13.84605608623171058, -284.6697458700030552, -342.1752454739954601 ) ) ;
#63620 = CARTESIAN_POINT ( 'NONE',  ( 160.5350683151633291, 250.0000000000000568, 20.22542485937379908 ) ) ;
#63621 = CARTESIAN_POINT ( 'NONE',  ( -96.25096420031067623, -283.1896048210906542, -223.9220389708277708 ) ) ;
#63622 = DIRECTION ( 'NONE',  ( -0.000000000000000000, -0.000000000000000000, -1.000000000000000000 ) ) ;
#63623 = CARTESIAN_POINT ( 'NONE',  ( -68.70085376097279095, -294.2686422860041375, -336.7355608441679919 ) ) ;
#63624 = CARTESIAN_POINT ( 'NONE',  ( 23.75321667938735715, -286.2695566538734511, -312.5531319799890184 ) ) ;
#63625 = CARTESIAN_POINT ( 'NONE',  ( 157.4851178187871312, 14.99999999999999467, -7.000000000000000888 ) ) ;
#63626 = CARTESIAN_POINT ( 'NONE',  ( -8.484261040513862540, -292.6742987289941311, -339.6011649178135485 ) ) ;
#63627 = CARTESIAN_POINT ( 'NONE',  ( -38.73943341945930285, -281.5492694448396946, -346.6549846866687403 ) ) ;
#63628 = CARTESIAN_POINT ( 'NONE',  ( -22.04830474426682230, -281.8513427663378366, -198.1106862788269041 ) ) ;
#63629 = CARTESIAN_POINT ( 'NONE',  ( -37.99453783505155258, -287.2492129303208799, -193.7609709635084130 ) ) ;
#63630 = CARTESIAN_POINT ( 'NONE',  ( 32.62401310169249768, -280.1758766801574438, -300.1395017171752784 ) ) ;
#63631 = CARTESIAN_POINT ( 'NONE',  ( 13.13955349035435205, -286.7813699701385417, -217.5595752225050887 ) ) ;
#63632 = CARTESIAN_POINT ( 'NONE',  ( -99.66452850903843341, -279.4402355833959177, -309.5873284188227785 ) ) ;
#63633 = CARTESIAN_POINT ( 'NONE',  ( -105.4143127907583590, -278.9972528677299692, -297.1700928207763468 ) ) ;
#63634 = CARTESIAN_POINT ( 'NONE',  ( -88.78225866803254007, -287.3145523014766241, -215.2240213693260102 ) ) ;
#63635 = CIRCLE ( 'NONE', #22694, 5.568361562975243650 ) ;
#63636 = VERTEX_POINT ( 'NONE', #76824 ) ;
#63637 = CARTESIAN_POINT ( 'NONE',  ( -48.96789359179543766, -297.7414090931777650, -194.1902287730759724 ) ) ;
#63639 = CARTESIAN_POINT ( 'NONE',  ( -98.68658680091428437, -291.9522714501241012, -312.9118093830333009 ) ) ;
#63638 = AXIS2_PLACEMENT_3D ( 'NONE', #9668, #67908, #74069 ) ;
#63640 = FACE_OUTER_BOUND ( 'NONE', #62452, .T. ) ;
#63641 = CARTESIAN_POINT ( 'NONE',  ( 36.57525178469696669, -295.6233781216987495, -234.7283546768995564 ) ) ;
#63642 = ORIENTED_EDGE ( 'NONE', *, *, #34990, .F. ) ;
#63643 = CARTESIAN_POINT ( 'NONE',  ( 21.34338638418532597, -272.9073228981062584, -223.3716754176242887 ) ) ;
#63644 = CARTESIAN_POINT ( 'NONE',  ( -106.4494898238646101, -294.5368695084363821, -302.4633580410126683 ) ) ;
#63645 = CARTESIAN_POINT ( 'NONE',  ( -79.75868411222276677, -296.9687054029865863, -210.8734057120314276 ) ) ;
#63646 = CARTESIAN_POINT ( 'NONE',  ( 30.06702910626900760, -289.4707491685632590, -300.2664992799170705 ) ) ;
#63647 = CARTESIAN_POINT ( 'NONE',  ( 30.94796143133324051, -282.9346893650776451, -241.8217393034181271 ) ) ;
#63648 = CARTESIAN_POINT ( 'NONE',  ( -34.66911401790626002, -290.4444504070248172, -346.7251381603615528 ) ) ;
#63649 = CARTESIAN_POINT ( 'NONE',  ( -113.6193618540808359, -291.7846663697735607, -276.9280413314039038 ) ) ;
#63650 = CARTESIAN_POINT ( 'NONE',  ( -74.56992585627847347, -287.5570800587402118, -205.2381592798225256 ) ) ;
#63651 = CARTESIAN_POINT ( 'NONE',  ( -22.56825951563721944, -280.4027918226349811, -194.7373883799859016 ) ) ;
#63652 = CARTESIAN_POINT ( 'NONE',  ( 23.70810382217629453, -292.2344658252532668, -314.9052085002197714 ) ) ;
#63653 = CARTESIAN_POINT ( 'NONE',  ( 36.47807151846856044, -281.6623156860285917, -292.4452423094710980 ) ) ;
#63654 = CARTESIAN_POINT ( 'NONE',  ( 34.09282492035468692, -277.6756924297259843, -290.6060599060998015 ) ) ;
#63655 = CARTESIAN_POINT ( 'NONE',  ( -114.2704648735229114, -299.0519495502701943, -270.3937649182068981 ) ) ;
#63656 = CARTESIAN_POINT ( 'NONE',  ( -3.200753811961945861, -274.8473952525937420, -338.2605758223133421 ) ) ;
#63657 = DIRECTION ( 'NONE',  ( 5.551115123125777653E-14, 0.000000000000000000, 1.000000000000000000 ) ) ;
#63658 = CARTESIAN_POINT ( 'NONE',  ( 21.85812250357357200, -281.6585488036643028, -313.2003999035796937 ) ) ;
#63659 = CARTESIAN_POINT ( 'NONE',  ( -112.0935483623751310, -279.5468013900305095, -287.0993946595646662 ) ) ;
#63660 = CARTESIAN_POINT ( 'NONE',  ( -19.16574801169045728, -275.6060272647622469, -199.0982403697296661 ) ) ;
#63661 = CARTESIAN_POINT ( 'NONE',  ( -49.29622491187091526, -284.9622309750282625, -194.4793892137579405 ) ) ;
#63662 = CARTESIAN_POINT ( 'NONE',  ( -109.6479298844231494, -292.1059518732088236, -286.2244806824243142 ) ) ;
#63663 = CARTESIAN_POINT ( 'NONE',  ( -106.1298781139952752, -274.5769215735016360, -237.5796143140116214 ) ) ;
#63664 = CARTESIAN_POINT ( 'NONE',  ( -29.90359703394742041, -275.4596142662841771, -194.2166966849506480 ) ) ;
#63665 = CYLINDRICAL_SURFACE ( 'NONE', #56116, 4.999999999999997335 ) ;
#63666 = CARTESIAN_POINT ( 'NONE',  ( 17.43382353512224725, -276.0747326739855225, -318.6359802855083103 ) ) ;
#63667 = CARTESIAN_POINT ( 'NONE',  ( -69.27715342387141106, -297.4733591727828639, -338.0520366508173424 ) ) ;
#63668 = CARTESIAN_POINT ( 'NONE',  ( -99.05843318894099525, -281.9762871665454895, -312.7725464775796240 ) ) ;
#63669 = CARTESIAN_POINT ( 'NONE',  ( -88.63223674173994482, -291.0220872701289068, -212.9588084007271505 ) ) ;
#63670 = CARTESIAN_POINT ( 'NONE',  ( 31.79207601991550192, -273.9426320196336064, -298.6475660743995491 ) ) ;
#63671 = CARTESIAN_POINT ( 'NONE',  ( -29.04383125834513280, -290.5489164195581111, -346.1609421142818519 ) ) ;
#63672 = CARTESIAN_POINT ( 'NONE',  ( -108.6542976877102689, -289.2492470986931039, -287.3534546068873397 ) ) ;
#63673 = ORIENTED_EDGE ( 'NONE', *, *, #65170, .T. ) ;
#63674 = CARTESIAN_POINT ( 'NONE',  ( -112.5885856976706663, -289.2943231149649819, -257.0753170745582565 ) ) ;
#63675 = CARTESIAN_POINT ( 'NONE',  ( -92.43047088025990377, -289.5350012985219905, -318.3669984504579133 ) ) ;
#63676 = ORIENTED_EDGE ( 'NONE', *, *, #82014, .F. ) ;
#63677 = CARTESIAN_POINT ( 'NONE',  ( 9.610619951405739769, -287.7608868028872848, -209.7230758965140467 ) ) ;
#63678 = CARTESIAN_POINT ( 'NONE',  ( -109.1536657757257558, -279.0599576937108282, -257.1274836875249434 ) ) ;
#63679 = CARTESIAN_POINT ( 'NONE',  ( -76.93447480514839754, -294.4893377425151471, -336.1032278560408031 ) ) ;
#63680 = CARTESIAN_POINT ( 'NONE',  ( -76.69858512047977683, -284.2154580921784941, -336.4860668419599961 ) ) ;
#63681 = EDGE_CURVE ( 'NONE', #93231, #36642, #56466, .T. ) ;
#63682 = CARTESIAN_POINT ( 'NONE',  ( -40.81976679879269199, -286.3429391840497829, -193.4086966328136441 ) ) ;
#63683 = CARTESIAN_POINT ( 'NONE',  ( 15.84417465479622322, -282.6061953805953522, -320.4675635854309803 ) ) ;
#63684 = CARTESIAN_POINT ( 'NONE',  ( -31.07673192236308424, -124.3734504823686962, -364.3838213891494888 ) ) ;
#63685 = CARTESIAN_POINT ( 'NONE',  ( 43.83784456572419685, 12.84970072374473737, -330.9960382518970619 ) ) ;
#63686 = CARTESIAN_POINT ( 'NONE',  ( -39.93747649349531059, -139.5826026648105085, -361.0100247098301907 ) ) ;
#63687 = CARTESIAN_POINT ( 'NONE',  ( -1.634905906460258906, -273.7354602071849854, -206.4904756821619856 ) ) ;
#63688 = CARTESIAN_POINT ( 'NONE',  ( 20.10628150010920834, -273.8321851414908110, -224.8003252046226805 ) ) ;
#63689 = CARTESIAN_POINT ( 'NONE',  ( 6.573729391164721214, -293.9807122299586126, -333.6000913306708071 ) ) ;
#63690 = CARTESIAN_POINT ( 'NONE',  ( -11.55711478694791161, -92.90135622777104629, -356.6579504680683499 ) ) ;
#63691 = CARTESIAN_POINT ( 'NONE',  ( 39.13833294582089906, -274.2114841270401939, -268.3355779384526159 ) ) ;
#63692 = CARTESIAN_POINT ( 'NONE',  ( -107.8879127575920336, -298.7160927182049477, -247.0874419083096711 ) ) ;
#63693 = CARTESIAN_POINT ( 'NONE',  ( -36.21511383969458819, -293.1462426274928248, -197.0481323084369762 ) ) ;
#63694 = ORIENTED_EDGE ( 'NONE', *, *, #31803, .T. ) ;
#63695 = CARTESIAN_POINT ( 'NONE',  ( -75.67284489018850024, -298.4952808069903654, -203.7903821163441478 ) ) ;
#63696 = CARTESIAN_POINT ( 'NONE',  ( 17.87615561098969152, -288.7264212935947967, -318.2801268898141984 ) ) ;
#63697 = CARTESIAN_POINT ( 'NONE',  ( -98.14040841507191715, -296.7264721508881280, -317.3470296139737457 ) ) ;
#63698 = CARTESIAN_POINT ( 'NONE',  ( -103.0597634418432307, -296.5216504262801891, -310.3694053417344776 ) ) ;
#63699 = CARTESIAN_POINT ( 'NONE',  ( 21.80346220801986945, -293.1199825662564535, -227.5514318310680437 ) ) ;
#63700 = EDGE_LOOP ( 'NONE', ( #6329, #8967, #69251, #172 ) ) ;
#63701 = CARTESIAN_POINT ( 'NONE',  ( 35.19641342558200847, -277.1998366912591223, -249.0234314943387233 ) ) ;
#63702 = EDGE_CURVE ( 'NONE', #33827, #67960, #12916, .T. ) ;
#63703 = ORIENTED_EDGE ( 'NONE', *, *, #27878, .F. ) ;
#63704 = CARTESIAN_POINT ( 'NONE',  ( 30.67034995205150238, -280.5936670031093172, -234.2768650438665929 ) ) ;
#63705 = CARTESIAN_POINT ( 'NONE',  ( -4.008259465461589066, -275.4442166790726105, -205.1374542664041769 ) ) ;
#63706 = CARTESIAN_POINT ( 'NONE',  ( 32.76979212578559242, -276.9331675882158379, -240.9276603867034794 ) ) ;
#63707 = CARTESIAN_POINT ( 'NONE',  ( -28.81278724125510138, -274.9647697364574697, -345.2845329032169275 ) ) ;
#63708 = CARTESIAN_POINT ( 'NONE',  ( -88.20261373559930007, -297.9687287417392554, -217.7827221894572460 ) ) ;
#63709 = CARTESIAN_POINT ( 'NONE',  ( -90.84804216980678859, -294.4043526758500775, -320.9562648391395783 ) ) ;
#63710 = CARTESIAN_POINT ( 'NONE',  ( -147.0026986695707762, -210.7421749798627388, 22.50000000000000000 ) ) ;
#63711 = CARTESIAN_POINT ( 'NONE',  ( -110.6061385808732780, -278.7469560954016288, -294.0240732530908190 ) ) ;
#63712 = CARTESIAN_POINT ( 'NONE',  ( 26.76777047168038948, -276.1966812995781879, -305.3806301853728087 ) ) ;
#63713 = CARTESIAN_POINT ( 'NONE',  ( 38.48871946633914831, -286.1092089911608696, -260.2099733851670749 ) ) ;
#63714 = CARTESIAN_POINT ( 'NONE',  ( -109.1304039746951986, -274.8341690070667482, -248.4720392225015644 ) ) ;
#63715 = CARTESIAN_POINT ( 'NONE',  ( 0.000000000000000000, 15.00000000000000000, -9.000000000000001776 ) ) ;
#63716 = CARTESIAN_POINT ( 'NONE',  ( 34.72826240167805878, -286.5798283089247320, -257.4845635184381649 ) ) ;
#63717 = CARTESIAN_POINT ( 'NONE',  ( -92.03067547374351420, -277.4973931828174045, -220.4903851839320339 ) ) ;
#63719 = CARTESIAN_POINT ( 'NONE',  ( -94.54401026523802898, -281.9691851961850944, -317.9973428115391698 ) ) ;
#63718 = CARTESIAN_POINT ( 'NONE',  ( -108.5380785521290363, -277.3712424963451895, -251.6984852186540138 ) ) ;
#63720 = CARTESIAN_POINT ( 'NONE',  ( -74.39005688471782207, -287.5597041575051094, -205.1359047472036252 ) ) ;
#63721 = CARTESIAN_POINT ( 'NONE',  ( -11.09780799893162317, -277.9073718091227079, -338.9059108617805691 ) ) ;
#63722 = DIRECTION ( 'NONE',  ( 1.000000000000000000, -0.000000000000000000, 0.000000000000000000 ) ) ;
#63723 = CARTESIAN_POINT ( 'NONE',  ( -98.41756170676512738, -293.1441825838879822, -226.8325091971890117 ) ) ;
#63724 = CARTESIAN_POINT ( 'NONE',  ( -88.54602570495654845, -275.9985925782652885, -326.5046042829356452 ) ) ;
#63725 = CARTESIAN_POINT ( 'NONE',  ( -34.04437078377078763, -274.7461334701972078, -197.3335869576112316 ) ) ;
#63726 = CARTESIAN_POINT ( 'NONE',  ( 22.80383219056214017, -284.1669401045190853, -315.4448553135704856 ) ) ;
#63727 = DIRECTION ( 'NONE',  ( 1.000000000000000000, 0.000000000000000000, 0.000000000000000000 ) ) ;
#63728 = CARTESIAN_POINT ( 'NONE',  ( 38.13770408471518181, -289.4151841304492905, -265.8789775539829634 ) ) ;
#63729 = CARTESIAN_POINT ( 'NONE',  ( -7.258204104566812198, -292.6575793450151650, -339.1179434068606611 ) ) ;
#63730 = DIRECTION ( 'NONE',  ( -0.000000000000000000, -1.000000000000000000, -0.000000000000000000 ) ) ;
#63731 = CARTESIAN_POINT ( 'NONE',  ( -48.93683761338657234, -272.5863141585922449, -197.7369036391480108 ) ) ;
#63732 = CARTESIAN_POINT ( 'NONE',  ( 33.81983940537519118, -291.4145406229175705, -249.0437582118194939 ) ) ;
#63733 = CARTESIAN_POINT ( 'NONE',  ( -113.2098679957031493, -271.2709011634024137, -296.4525692007673570 ) ) ;
#63734 = CARTESIAN_POINT ( 'NONE',  ( 165.2494399300530290, -11.64849832608277325, 10.00000000000000000 ) ) ;
#63735 = CARTESIAN_POINT ( 'NONE',  ( -107.7201381255608368, -289.4105309400522970, -240.8724215698831586 ) ) ;
#63736 = CARTESIAN_POINT ( 'NONE',  ( 19.54325550619518737, -285.0998133111575612, -219.9040976386709758 ) ) ;
#63737 = CARTESIAN_POINT ( 'NONE',  ( -107.9252669706393561, -286.2527566660064622, -249.3675327935352470 ) ) ;
#63738 = CARTESIAN_POINT ( 'NONE',  ( -105.7194745871824324, -285.7016360030070814, -244.3403246303864194 ) ) ;
#63739 = CARTESIAN_POINT ( 'NONE',  ( -63.83466660808178972, -293.6884461325701068, -199.7616146812952991 ) ) ;
#63740 = CARTESIAN_POINT ( 'NONE',  ( 37.70434537338154968, -273.7497022758938670, -279.5966210289873288 ) ) ;
#63741 = CARTESIAN_POINT ( 'NONE',  ( 20.80706618780867601, -276.5674423442608827, -320.8237625279735994 ) ) ;
#63742 = CARTESIAN_POINT ( 'NONE',  ( -107.4712194354002435, -288.2682441628352308, -298.4887683905960216 ) ) ;
#63743 = CARTESIAN_POINT ( 'NONE',  ( 18.90321009041295497, -276.2694000751052386, -322.9492352193798865 ) ) ;
#63744 = CARTESIAN_POINT ( 'NONE',  ( -91.58554430201388641, -297.8089678893813925, -321.7137113574090677 ) ) ;
#63745 = CYLINDRICAL_SURFACE ( 'NONE', #60574, 3.842139515347647638 ) ;
#63746 = CARTESIAN_POINT ( 'NONE',  ( 165.2494399300530290, 8.542400036368780647, 25.74970488511327815 ) ) ;
#63747 = CARTESIAN_POINT ( 'NONE',  ( -92.04322998459038274, -282.5390839857075775, -319.4614828439005123 ) ) ;
#63748 = CARTESIAN_POINT ( 'NONE',  ( -4.509517342370576998, -278.4845707405439725, -202.9151682825841760 ) ) ;
#63749 = CARTESIAN_POINT ( 'NONE',  ( 201.2929949297285077, 65.04117685566218654, 7.250946725472672938 ) ) ;
#63750 = CARTESIAN_POINT ( 'NONE',  ( 30.64144728577259613, -273.5816689302036480, -235.7056794681675171 ) ) ;
#63751 = CARTESIAN_POINT ( 'NONE',  ( -83.07698397872601959, -277.0457044972561107, -327.4541297975299017 ) ) ;
#63752 = CARTESIAN_POINT ( 'NONE',  ( 35.89823626676859192, -295.1848101735887440, -278.9725172894914635 ) ) ;
#63753 = CARTESIAN_POINT ( 'NONE',  ( 39.33219139450238799, -280.4313367002683322, -267.0843536968103535 ) ) ;
#63754 = CARTESIAN_POINT ( 'NONE',  ( -82.49549168579201819, -296.6272288680765428, -328.0846212851636778 ) ) ;
#63755 = CARTESIAN_POINT ( 'NONE',  ( -33.44310843291610524, -296.3192385725066629, -346.7816087142763308 ) ) ;
#63756 = CARTESIAN_POINT ( 'NONE',  ( -72.84502542494871591, -297.4010674665589136, -206.5762146167980120 ) ) ;
#63757 = CARTESIAN_POINT ( 'NONE',  ( -22.36549584848196304, -294.2441040320430830, -196.8715680377788146 ) ) ;
#63758 = CARTESIAN_POINT ( 'NONE',  ( -78.52425460745261887, -285.6806199053597197, -205.2996300572852135 ) ) ;
#63759 = CARTESIAN_POINT ( 'NONE',  ( -89.29829430854913142, -271.4701366504730800, -215.1458851708738393 ) ) ;
#63760 = CARTESIAN_POINT ( 'NONE',  ( 32.71291018312218313, -286.9754881330266585, -238.2741641205226415 ) ) ;
#63761 = CARTESIAN_POINT ( 'NONE',  ( -108.8090316680152654, -280.8110248899912449, -248.8142544969474841 ) ) ;
#63762 = ADVANCED_FACE ( 'NONE', ( #77290 ), #91942, .F. ) ;
#63763 = CARTESIAN_POINT ( 'NONE',  ( -54.80085219291658660, -284.8810501478265564, -199.1849130997260602 ) ) ;
#63764 = CARTESIAN_POINT ( 'NONE',  ( -92.14914908545156891, -287.8345793509295731, -321.6331060379923201 ) ) ;
#63765 = CARTESIAN_POINT ( 'NONE',  ( 207.9739649226136180, 291.4638663531892462, -68.48153742335392735 ) ) ;
#63766 = CARTESIAN_POINT ( 'NONE',  ( 34.05747892948230060, -286.8555494794040328, -254.8644837746137455 ) ) ;
#63767 = AXIS2_PLACEMENT_3D ( 'NONE', #32059, #3652, #53361 ) ;
#63768 = CARTESIAN_POINT ( 'NONE',  ( -50.04273765835110765, -284.1515421170400941, -346.1215237110538965 ) ) ;
#63769 = CARTESIAN_POINT ( 'NONE',  ( -94.52799409573900391, -290.3077173873032848, -219.1502988574988535 ) ) ;
#63770 = CARTESIAN_POINT ( 'NONE',  ( -113.2489331221395048, -280.2439095637512310, -263.1105287173102738 ) ) ;
#63771 = CARTESIAN_POINT ( 'NONE',  ( -101.4869556204810408, -280.4195366246457297, -228.5676890210993406 ) ) ;
#63772 = CARTESIAN_POINT ( 'NONE',  ( 34.33464662420605862, -281.2020511916978194, -256.4568544086280326 ) ) ;
#63773 = CARTESIAN_POINT ( 'NONE',  ( 12.86702739149617436, -276.7526178099279264, -214.5769015516253262 ) ) ;
#63774 = CARTESIAN_POINT ( 'NONE',  ( -69.52792029245891570, -295.4641715322786695, -340.3258708293686823 ) ) ;
#63775 = CARTESIAN_POINT ( 'NONE',  ( -108.5636036013131900, -288.8623837752676877, -247.9733699220326173 ) ) ;
#63776 = CARTESIAN_POINT ( 'NONE',  ( -108.7751547041566056, -295.6889208430971507, -253.8842359332637670 ) ) ;
#63777 = VERTEX_POINT ( 'NONE', #5342 ) ;
#63778 = VERTEX_POINT ( 'NONE', #27096 ) ;
#63779 = CARTESIAN_POINT ( 'NONE',  ( 34.35280635332465238, -283.7319234407000295, -290.3913935670002502 ) ) ;
#63780 = CARTESIAN_POINT ( 'NONE',  ( -106.8907132148062971, -295.9219512209721188, -292.7739342437091636 ) ) ;
#63781 = CARTESIAN_POINT ( 'NONE',  ( 39.34638038248613867, -294.5950747074009541, -267.4346271081413420 ) ) ;
#63782 = CARTESIAN_POINT ( 'NONE',  ( -3.566921220749860844, -283.2454588910824782, -335.2069023307449811 ) ) ;
#63783 = CARTESIAN_POINT ( 'NONE',  ( 19.86855022352509081, -273.9139232226220884, -219.0989316371287998 ) ) ;
#63784 = CARTESIAN_POINT ( 'NONE',  ( -4.369239354835378286, -289.2803436228336409, -339.8459298248872074 ) ) ;
#63785 = CARTESIAN_POINT ( 'NONE',  ( -5.988645452508174927, -280.7840180005426305, -339.3342391686034034 ) ) ;
#63786 = CARTESIAN_POINT ( 'NONE',  ( -113.7920368271609988, -290.7672799340705296, -279.8058919025192495 ) ) ;
#63787 = CARTESIAN_POINT ( 'NONE',  ( -3.352748113942630059, -288.9239665833383128, -335.0455866819347648 ) ) ;
#63788 = DIRECTION ( 'NONE',  ( -1.000000000000000000, 0.000000000000000000, 0.000000000000000000 ) ) ;
#63789 = DIRECTION ( 'NONE',  ( 0.000000000000000000, 1.000000000000000000, -0.000000000000000000 ) ) ;
#63790 = CARTESIAN_POINT ( 'NONE',  ( 202.4138562182569672, 292.0436489450776207, -53.99999999998431832 ) ) ;
#63791 = CARTESIAN_POINT ( 'NONE',  ( -8.284807207348070079, -284.1987788159655679, -340.9749666555922545 ) ) ;
#63792 = CARTESIAN_POINT ( 'NONE',  ( 35.77081079830085031, -291.2666405000204577, -287.0812184334320705 ) ) ;
#63793 = ORIENTED_EDGE ( 'NONE', *, *, #29767, .F. ) ;
#63794 = CARTESIAN_POINT ( 'NONE',  ( -91.51601861600957477, -278.1777531467093354, -220.9711464265127461 ) ) ;
#63795 = CARTESIAN_POINT ( 'NONE',  ( -18.55102464135140039, -273.9543749488533422, -195.6558859789888061 ) ) ;
#63796 = CARTESIAN_POINT ( 'NONE',  ( -46.09795327289893407, -279.1634940189329086, -344.7323015913306108 ) ) ;
#63797 = CARTESIAN_POINT ( 'NONE',  ( 162.6064035890194646, 217.7902839693395549, -203.4103096416544929 ) ) ;
#63798 = CARTESIAN_POINT ( 'NONE',  ( 38.68987013377453366, -280.2291292074517060, -278.4741444403497894 ) ) ;
#63799 = CARTESIAN_POINT ( 'NONE',  ( -0.4607812854550503712, -280.5794144521117914, -335.2583030436366016 ) ) ;
#63800 = CARTESIAN_POINT ( 'NONE',  ( -109.3778401604835295, -298.0037104908390120, -294.5431059548459416 ) ) ;
#63801 = CARTESIAN_POINT ( 'NONE',  ( 18.02316104008952635, -294.7230418898782318, -318.0532549517193388 ) ) ;
#63802 = VERTEX_POINT ( 'NONE', #55983 ) ;
#63803 = CARTESIAN_POINT ( 'NONE',  ( -57.77610454242650206, -290.4676348550997318, -199.7127135470596500 ) ) ;
#63804 = CARTESIAN_POINT ( 'NONE',  ( 21.76717817412899336, -275.5410885884037953, -221.1731794928912223 ) ) ;
#63805 = CARTESIAN_POINT ( 'NONE',  ( -90.19660543137686659, -273.2784594614061007, -219.9904813671150521 ) ) ;
#63806 = EDGE_LOOP ( 'NONE', ( #90699, #20950, #67790, #93653, #81461 ) ) ;
#63807 = DIRECTION ( 'NONE',  ( -0.000000000000000000, -0.000000000000000000, 1.000000000000000000 ) ) ;
#63808 = DIRECTION ( 'NONE',  ( 1.000000000000000000, 0.000000000000000000, 0.000000000000000000 ) ) ;
#63809 = FACE_OUTER_BOUND ( 'NONE', #35101, .T. ) ;
#63810 = CARTESIAN_POINT ( 'NONE',  ( -62.42759092147420574, -280.7977816206793023, -201.4241203814754329 ) ) ;
#63811 = CARTESIAN_POINT ( 'NONE',  ( 21.17581120810025652, -282.6519351503295070, -221.8876728420265749 ) ) ;
#63812 = CARTESIAN_POINT ( 'NONE',  ( -109.6515444122650251, -283.7645479020408743, -258.6759517145612222 ) ) ;
#63813 = CARTESIAN_POINT ( 'NONE',  ( -6.273742743945875944, -282.3250987886999610, -202.9258257372329979 ) ) ;
#63814 = CARTESIAN_POINT ( 'NONE',  ( 36.29368926362795378, -274.0844018883019544, -274.3694596340391172 ) ) ;
#63815 = DIRECTION ( 'NONE',  ( -0.000000000000000000, -0.000000000000000000, 1.000000000000000000 ) ) ;
#63816 = CARTESIAN_POINT ( 'NONE',  ( 189.9243309297870610, 250.5000000000000568, 24.72542485937349710 ) ) ;
#63817 = CARTESIAN_POINT ( 'NONE',  ( -75.24762348572066628, -278.3469872631963540, -337.1989799694664498 ) ) ;
#63818 = EDGE_CURVE ( 'NONE', #82379, #64275, #63584, .T. ) ;
#63819 = ORIENTED_EDGE ( 'NONE', *, *, #45978, .F. ) ;
#63820 = VERTEX_POINT ( 'NONE', #27569 ) ;
#63821 = CARTESIAN_POINT ( 'NONE',  ( -44.24291873220152382, -285.1187785616862129, -345.4518581966116244 ) ) ;
#63822 = CARTESIAN_POINT ( 'NONE',  ( 22.72634353672973617, -292.1682229093307228, -228.5726439016649465 ) ) ;
#63823 = EDGE_CURVE ( 'NONE', #90166, #6260, #65515, .T. ) ;
#63824 = CARTESIAN_POINT ( 'NONE',  ( 38.00674755905752988, -287.0930927040805614, -285.7209427902196239 ) ) ;
#63825 = CARTESIAN_POINT ( 'NONE',  ( -109.6501525313736067, -282.9982799642866098, -254.5076713940242996 ) ) ;
#63827 = CARTESIAN_POINT ( 'NONE',  ( 23.57130789212449429, -286.3698151807546992, -312.4260393832969953 ) ) ;
#63826 = CARTESIAN_POINT ( 'NONE',  ( -79.63319640983496583, -284.0431979902666626, -210.0756156493136757 ) ) ;
#63828 = CARTESIAN_POINT ( 'NONE',  ( 35.91523753047317058, -282.6977550788365079, -265.8277319654869757 ) ) ;
#63829 = CARTESIAN_POINT ( 'NONE',  ( -5.928139016700665564, -272.4649302086914986, -202.2568682551758172 ) ) ;
#63830 = VECTOR ( 'NONE', #86466, 1000.000000000000000 ) ;
#63831 = CARTESIAN_POINT ( 'NONE',  ( -110.1554670494622457, -283.2391298779421618, -247.7204685870175638 ) ) ;
#63832 = CARTESIAN_POINT ( 'NONE',  ( -102.1351669354357341, -299.0580786989693252, -232.4856098810211904 ) ) ;
#63833 = CARTESIAN_POINT ( 'NONE',  ( -111.1920370516100149, -282.7348430719764565, -256.0852206937172468 ) ) ;
#63834 = CIRCLE ( 'NONE', #75892, 4.499999999999990230 ) ;
#63835 = CARTESIAN_POINT ( 'NONE',  ( -16.86738248179304023, -281.2644266761291192, -200.0460359272181279 ) ) ;
#63836 = CARTESIAN_POINT ( 'NONE',  ( 37.86847630212764670, -289.5668755342401255, -271.4975313261301721 ) ) ;
#63837 = CARTESIAN_POINT ( 'NONE',  ( 196.6877655503061817, 293.7115289173626707, -7.999911143031724237 ) ) ;
#63838 = LINE ( 'NONE', #20723, #54921 ) ;
#63839 = CARTESIAN_POINT ( 'NONE',  ( 37.42333510476321123, -295.3285179475146265, -259.0790458297708483 ) ) ;
#63840 = VECTOR ( 'NONE', #7906, 1000.000000000000000 ) ;
#63841 = CARTESIAN_POINT ( 'NONE',  ( -99.31543678382014662, -275.9800244515741952, -312.6015797959382780 ) ) ;
#63842 = CARTESIAN_POINT ( 'NONE',  ( -91.49200464830124702, -288.9962009914140708, -324.9511423292060499 ) ) ;
#63843 = CARTESIAN_POINT ( 'NONE',  ( -15.37391446412879326, -293.1629958653196582, -340.8695105723052734 ) ) ;
#63844 = CARTESIAN_POINT ( 'NONE',  ( -30.19788987629874200, -278.8290988925231773, -197.1652965699153128 ) ) ;
#63845 = CARTESIAN_POINT ( 'NONE',  ( -104.4937802609203175, -271.0580530685751341, -238.2377257472312522 ) ) ;
#63846 = CARTESIAN_POINT ( 'NONE',  ( -4.628515023603078760, -293.8075450568010183, -204.5360756298416050 ) ) ;
#63847 = CARTESIAN_POINT ( 'NONE',  ( -110.4683760289727132, -287.2662352645559167, -253.7030783399848985 ) ) ;
#63848 = CARTESIAN_POINT ( 'NONE',  ( -111.9187178457651441, -295.2366300057087187, -254.1454466737765188 ) ) ;
#63849 = CARTESIAN_POINT ( 'NONE',  ( 1.752452504987862536, -290.1198481316873767, -332.9557475003668401 ) ) ;
#63850 = CARTESIAN_POINT ( 'NONE',  ( -44.77530831762304331, -290.1992870000940457, -194.6867032898723266 ) ) ;
#63851 = CARTESIAN_POINT ( 'NONE',  ( -110.8943557418349570, -291.9303931852601295, -273.9556923212676907 ) ) ;
#63852 = CARTESIAN_POINT ( 'NONE',  ( 189.9243309297870610, 250.0000000000000568, 20.22542485937349355 ) ) ;
#63853 = CARTESIAN_POINT ( 'NONE',  ( -107.5531388676546811, -291.6270004388076131, -249.7507281951459674 ) ) ;
#63854 = FACE_OUTER_BOUND ( 'NONE', #55298, .T. ) ;
#63855 = CARTESIAN_POINT ( 'NONE',  ( -96.97126178976934341, -291.1090196875140350, -318.4684305686678840 ) ) ;
#63857 = CARTESIAN_POINT ( 'NONE',  ( 24.84787079955360412, -293.0240290120265740, -232.0361438693508092 ) ) ;
#63856 = CARTESIAN_POINT ( 'NONE',  ( 37.63876384571953082, -279.6745986813138529, -278.3693361883300099 ) ) ;
#63858 = CARTESIAN_POINT ( 'NONE',  ( -45.27337108283251865, -279.9544503059973977, -193.7177326970513036 ) ) ;
#63859 = CARTESIAN_POINT ( 'NONE',  ( 17.80816477315422119, -281.9560978229920352, -324.1423692431051222 ) ) ;
#63860 = CARTESIAN_POINT ( 'NONE',  ( 6.908704449835291861, -286.4486423060803304, -330.7740870580619799 ) ) ;
#63861 = CARTESIAN_POINT ( 'NONE',  ( 21.98296813773478320, -280.3082111784922290, -315.0077722923272745 ) ) ;
#63862 = CARTESIAN_POINT ( 'NONE',  ( -57.20117490572079788, -283.7958924556551779, -197.9843088319997548 ) ) ;
#63863 = CARTESIAN_POINT ( 'NONE',  ( -5.218093358983717955, -278.9471862940930578, -201.1456454107276670 ) ) ;
#63864 = CARTESIAN_POINT ( 'NONE',  ( -2.351619894606735262, -285.4244546327939815, -202.1028391750618880 ) ) ;
#63865 = CARTESIAN_POINT ( 'NONE',  ( 3.010500028292293351, -275.4117782673250190, -209.2735199486696729 ) ) ;
#63866 = CARTESIAN_POINT ( 'NONE',  ( 195.3516019189765132, 40.92429273362618858, 14.83660509754012047 ) ) ;
#63867 = CARTESIAN_POINT ( 'NONE',  ( 33.89420135918904009, -295.4048268992617636, -289.6935827811574882 ) ) ;
#63868 = CARTESIAN_POINT ( 'NONE',  ( 38.15646561286266802, -277.1300008898330134, -282.4679599193767672 ) ) ;
#63869 = CARTESIAN_POINT ( 'NONE',  ( -89.10380335433531229, -277.4713381324768307, -321.9379933816849757 ) ) ;
#63870 = CARTESIAN_POINT ( 'NONE',  ( -73.43559284086877881, -291.7535333634036760, -202.3298162416406569 ) ) ;
#63871 = CARTESIAN_POINT ( 'NONE',  ( -49.87911212311918518, -281.2905966865749292, -344.9265872018413006 ) ) ;
#63872 = CARTESIAN_POINT ( 'NONE',  ( -62.87155754369371152, -290.7701714296186992, -201.7197687210510537 ) ) ;
#63873 = CARTESIAN_POINT ( 'NONE',  ( 30.41203594710298574, -291.9765684371523093, -302.6446823547061626 ) ) ;
#63874 = EDGE_LOOP ( 'NONE', ( #91211, #10291, #83399, #2986 ) ) ;
#63875 = LINE ( 'NONE', #27882, #77183 ) ;
#63876 = CARTESIAN_POINT ( 'NONE',  ( -60.27233686336654728, -291.2544695448601146, -200.9381976835420005 ) ) ;
#63877 = CARTESIAN_POINT ( 'NONE',  ( 208.7622976689241057, 29.39913517558109035, 13.48907645363312291 ) ) ;
#63878 = CARTESIAN_POINT ( 'NONE',  ( -105.5795714935544112, -298.8376638359844719, -285.9686137636504668 ) ) ;
#63879 = CARTESIAN_POINT ( 'NONE',  ( -113.1552694616390227, -295.7630695077583027, -258.2312289835654724 ) ) ;
#63880 = ADVANCED_FACE ( 'NONE', ( #42217 ), #28506, .T. ) ;
#63881 = ADVANCED_FACE ( 'NONE', ( #78237 ), #12570, .T. ) ;
#63882 = CARTESIAN_POINT ( 'NONE',  ( -95.88209119270837277, -285.1995417971489815, -319.6390812674281392 ) ) ;
#63883 = CARTESIAN_POINT ( 'NONE',  ( 24.95182763898558775, -286.8610996736716174, -232.3017380240255818 ) ) ;
#63884 = CARTESIAN_POINT ( 'NONE',  ( 35.05100779430772207, -276.8921519726080192, -256.5769388807461837 ) ) ;
#63885 = CARTESIAN_POINT ( 'NONE',  ( -109.7647924879880890, -294.8061539525104990, -252.2328422257478167 ) ) ;
#63886 = CARTESIAN_POINT ( 'NONE',  ( -107.8275230432567469, -298.0150359777803715, -293.1039117068961559 ) ) ;
#63887 = CARTESIAN_POINT ( 'NONE',  ( -21.58264370543693289, -275.6406449344836460, -342.0986934635167813 ) ) ;
#63888 = ORIENTED_EDGE ( 'NONE', *, *, #69493, .F. ) ;
#63889 = PLANE ( 'NONE',  #36491 ) ;
#63890 = CARTESIAN_POINT ( 'NONE',  ( -105.2329583771384449, -296.6891710807491904, -233.9641532944656888 ) ) ;
#63891 = CARTESIAN_POINT ( 'NONE',  ( -23.49377399475570982, -290.7940722046583915, -343.5544519936491952 ) ) ;
#63892 = CARTESIAN_POINT ( 'NONE',  ( 85.55100297371609486, -373.0521521680024648, -525.1711561948568487 ) ) ;
#63893 = CARTESIAN_POINT ( 'NONE',  ( -13.24646216962237943, -289.3821390969849858, -339.3778708459862514 ) ) ;
#63894 = EDGE_LOOP ( 'NONE', ( #47083, #17204, #42529, #61906, #78587, #65103, #12786, #12659, #46149, #13591, #76197, #81576, #9445, #30437 ) ) ;
#63895 = CARTESIAN_POINT ( 'NONE',  ( 6.061120384202320466, -279.6842153298699714, -207.0443320249913768 ) ) ;
#63896 = CARTESIAN_POINT ( 'NONE',  ( -87.40220084427529912, -298.0268834631633013, -211.9191841063840798 ) ) ;
#63897 = CARTESIAN_POINT ( 'NONE',  ( -110.3580236809855393, -288.4342662246273221, -290.5829373117604177 ) ) ;
#63898 = CARTESIAN_POINT ( 'NONE',  ( -111.9471045184252773, -296.6474188180910687, -289.3821338599424848 ) ) ;
#63900 = CARTESIAN_POINT ( 'NONE',  ( 35.55548941238512839, -293.8188307166893765, -265.3106526661845237 ) ) ;
#63899 = AXIS2_PLACEMENT_3D ( 'NONE', #87299, #35740, #93020 ) ;
#63901 = CYLINDRICAL_SURFACE ( 'NONE', #79092, 3.000000000000000888 ) ;
#63902 = CIRCLE ( 'NONE', #30602, 1.000000000000000888 ) ;
#63903 = SURFACE_STYLE_FILL_AREA ( #70527 ) ;
#63904 = CARTESIAN_POINT ( 'NONE',  ( 196.7383257810085979, 42.27872732282705925, 11.00000000000000000 ) ) ;
#63905 = CARTESIAN_POINT ( 'NONE',  ( 35.29376715004156040, -289.3689962735458039, -293.7448013053996760 ) ) ;
#63906 = CARTESIAN_POINT ( 'NONE',  ( -19.05039376806008633, -279.3376638359844719, -350.3538533559490702 ) ) ;
#63907 = CIRCLE ( 'NONE', #26137, 7.500000000000013323 ) ;
#63908 = CARTESIAN_POINT ( 'NONE',  ( 38.69521478830813521, -280.7526989510703288, -258.5394398989590172 ) ) ;
#63909 = CARTESIAN_POINT ( 'NONE',  ( -12.90727045389426841, -284.7341782109277233, -341.1478725720385228 ) ) ;
#63910 = CARTESIAN_POINT ( 'NONE',  ( 9.464244038540272186, -285.2563462623699024, -209.9640163802309871 ) ) ;
#63912 = CARTESIAN_POINT ( 'NONE',  ( -107.0506840028030950, -288.9753708477634859, -244.1003949682119014 ) ) ;
#63911 = AXIS2_PLACEMENT_3D ( 'NONE', #52615, #45984, #81497 ) ;
#63913 = CARTESIAN_POINT ( 'NONE',  ( -25.93221553894920106, -278.7687428519294031, -345.2619133044655655 ) ) ;
#63915 = CARTESIAN_POINT ( 'NONE',  ( 32.07601627227643348, -280.5950732792880444, -247.2870407276015783 ) ) ;
#63914 = CARTESIAN_POINT ( 'NONE',  ( -104.4420681256212760, -278.9383619206318485, -241.6114986008234666 ) ) ;
#63916 = CARTESIAN_POINT ( 'NONE',  ( 19.65671261876532583, -277.3312506461663247, -321.6903594015559520 ) ) ;
#63917 = CARTESIAN_POINT ( 'NONE',  ( -84.31129892726592345, -278.2174077550121751, -209.7806518728222613 ) ) ;
#63918 = CARTESIAN_POINT ( 'NONE',  ( -90.76730617333356577, -228.9098355046940867, -345.5290054426631059 ) ) ;
#63919 = CARTESIAN_POINT ( 'NONE',  ( -52.51089187581975182, -274.8038067254300358, -195.0558227561601257 ) ) ;
#63920 = CARTESIAN_POINT ( 'NONE',  ( -67.95816730762523150, -299.0834443002640342, -200.2959036786763534 ) ) ;
#63921 = CARTESIAN_POINT ( 'NONE',  ( -114.2704648735229114, -293.0519495502703080, -270.3937649182068981 ) ) ;
#63922 = CARTESIAN_POINT ( 'NONE',  ( 175.2296996224750103, 154.6894116713782807, 0.000000000000000000 ) ) ;
#63923 = CARTESIAN_POINT ( 'NONE',  ( 35.93962257626139944, -288.6764844544147763, -273.7605098693581454 ) ) ;
#63924 = CARTESIAN_POINT ( 'NONE',  ( -111.3775496909184568, -286.5290943280365923, -253.2536050915478825 ) ) ;
#63925 = CARTESIAN_POINT ( 'NONE',  ( 32.37330116776406186, -286.6091009658677535, -248.3257585204912345 ) ) ;
#63926 = CARTESIAN_POINT ( 'NONE',  ( -112.9365813393347082, -284.2424117108164410, -255.7682841167352876 ) ) ;
#63927 = CARTESIAN_POINT ( 'NONE',  ( 31.82716349144546086, -279.6108167209565636, -244.4829234508656270 ) ) ;
#63928 = CARTESIAN_POINT ( 'NONE',  ( -22.23117688646444279, -288.1080109496847399, -197.6272956720659408 ) ) ;
#63929 = CARTESIAN_POINT ( 'NONE',  ( -5.239131764100291910, -278.9624145647896967, -204.0276207189525906 ) ) ;
#63930 = CARTESIAN_POINT ( 'NONE',  ( -39.15324416686435427, -278.3905360031849341, -343.8319406777193876 ) ) ;
#63931 = CARTESIAN_POINT ( 'NONE',  ( 9.519751953192566063, -275.2090770793129764, -214.2413899064675036 ) ) ;
#63932 = CARTESIAN_POINT ( 'NONE',  ( 5.323378345878090556, -287.2835517467686373, -333.9826536177548064 ) ) ;
#63933 = CARTESIAN_POINT ( 'NONE',  ( -21.74874811472405156, -283.6600031040663907, -345.6008592600969678 ) ) ;
#63934 = CARTESIAN_POINT ( 'NONE',  ( -79.12104613906727479, -284.0920160009975461, -334.9677209734464896 ) ) ;
#63935 = CARTESIAN_POINT ( 'NONE',  ( 13.92619242967292870, -282.4752263544112338, -322.3996205455611062 ) ) ;
#63936 = ORIENTED_EDGE ( 'NONE', *, *, #23960, .F. ) ;
#63937 = ORIENTED_EDGE ( 'NONE', *, *, #50938, .T. ) ;
#63938 = CARTESIAN_POINT ( 'NONE',  ( 165.2424497756046549, 214.5000000000000568, 22.91843887563435800 ) ) ;
#63939 = CARTESIAN_POINT ( 'NONE',  ( -6.113612522359519019, -290.5065484773019762, -339.3909088555104177 ) ) ;
#63940 = CARTESIAN_POINT ( 'NONE',  ( -86.18524014526099108, -290.0761294878942635, -211.4059533497838572 ) ) ;
#63941 = CARTESIAN_POINT ( 'NONE',  ( -92.18644043809439381, -272.3021030421900264, -221.8280065137352892 ) ) ;
#63942 = CARTESIAN_POINT ( 'NONE',  ( 39.12569766671325766, -292.7928488575410597, -261.7455906419088478 ) ) ;
#63943 = CARTESIAN_POINT ( 'NONE',  ( -18.31296690027854979, -287.2824853615557572, -341.6084061846958662 ) ) ;
#63944 = CARTESIAN_POINT ( 'NONE',  ( 32.48875889757632507, -292.1157054966603823, -295.0436267988609984 ) ) ;
#63945 = CARTESIAN_POINT ( 'NONE',  ( 1.534839239654746335, -289.7248591643124769, -332.6166012055394958 ) ) ;
#63946 = CARTESIAN_POINT ( 'NONE',  ( -37.37352853689063892, -288.5519495502701943, -195.3611179825600175 ) ) ;
#63947 = CARTESIAN_POINT ( 'NONE',  ( -102.0594008324897430, -292.0446285133974698, -308.3665507390087441 ) ) ;
#63948 = CARTESIAN_POINT ( 'NONE',  ( -111.1204602315069110, -288.7370523743019248, -255.9163171806554828 ) ) ;
#63949 = CARTESIAN_POINT ( 'NONE',  ( -64.34574406780967593, -293.7000612935581785, -200.3370762585978184 ) ) ;
#63950 = CARTESIAN_POINT ( 'NONE',  ( -71.29792806797661342, -286.5334382806494773, -205.4736536093269024 ) ) ;
#63951 = CARTESIAN_POINT ( 'NONE',  ( 18.98750762650380608, -294.8616755098453268, -220.5717214058626041 ) ) ;
#63952 = CARTESIAN_POINT ( 'NONE',  ( -112.5397100641337147, -270.5523142621870534, -270.3356552556126076 ) ) ;
#63953 = CARTESIAN_POINT ( 'NONE',  ( 175.2296996224749250, 249.5000000000000568, -24.99999999999999289 ) ) ;
#63954 = CARTESIAN_POINT ( 'NONE',  ( -36.97363918710599506, -276.0366581621883597, -194.9940397895167621 ) ) ;
#63955 = CARTESIAN_POINT ( 'NONE',  ( -59.56439087084695672, -281.3396374717880235, -342.0477862637842463 ) ) ;
#63956 = CARTESIAN_POINT ( 'NONE',  ( -113.7836169506870050, -295.6516053025841870, -278.1580515267068563 ) ) ;
#63957 = CARTESIAN_POINT ( 'NONE',  ( -8.556310642217372475, -272.6738577108719710, -202.1201210344045478 ) ) ;
#63958 = CARTESIAN_POINT ( 'NONE',  ( -104.4393792924921485, -276.2029107980352478, -302.7173383343444470 ) ) ;
#63959 = CARTESIAN_POINT ( 'NONE',  ( -79.09348697847681819, -274.6804055336842794, -209.9344927259447218 ) ) ;
#63960 = CARTESIAN_POINT ( 'NONE',  ( 6.908656765525013732, -273.2157517946503162, -208.0024159844666372 ) ) ;
#63961 = CARTESIAN_POINT ( 'NONE',  ( -108.5350469604711350, -297.7329041329210781, -289.0356676466272461 ) ) ;
#63962 = CARTESIAN_POINT ( 'NONE',  ( 175.2296996224750103, 140.2072866198470251, -21.95310499597075804 ) ) ;
#63963 = CARTESIAN_POINT ( 'NONE',  ( -82.05085867560535462, -298.2278221456635947, -212.3858269163354748 ) ) ;
#63964 = CARTESIAN_POINT ( 'NONE',  ( 199.4757856505664790, 63.23505538068130249, 9.191047964627605538 ) ) ;
#63966 = CARTESIAN_POINT ( 'NONE',  ( -107.1959075243145918, -272.6682334736833013, -248.9891644333909824 ) ) ;
#63965 = CARTESIAN_POINT ( 'NONE',  ( 33.51701669605155587, -285.9049048152741079, -296.1535586554102792 ) ) ;
#63967 = AXIS2_PLACEMENT_3D ( 'NONE', #35372, #44669, #92175 ) ;
#63968 = CARTESIAN_POINT ( 'NONE',  ( -63.20143416468979325, -285.7244031416678354, -197.8333704954370091 ) ) ;
#63969 = CARTESIAN_POINT ( 'NONE',  ( 16.28750053660273878, -286.4555227192495295, -215.1374534216471091 ) ) ;
#63970 = CARTESIAN_POINT ( 'NONE',  ( -100.9419878495283029, -299.0733041075435494, -229.9456481275238389 ) ) ;
#63971 = CARTESIAN_POINT ( 'NONE',  ( -48.08069442457507847, -293.1887845623392650, -344.4724648055770899 ) ) ;
#63972 = CIRCLE ( 'NONE', #23097, 20.00000000000000000 ) ;
#63973 = VECTOR ( 'NONE', #37304, 1000.000000000000000 ) ;
#63974 = CARTESIAN_POINT ( 'NONE',  ( -28.23397479790325804, -279.3619652105966225, -194.0107625888133782 ) ) ;
#63975 = CARTESIAN_POINT ( 'NONE',  ( -37.37352853689063181, -286.5523547857347353, -345.3611179825600175 ) ) ;
#63976 = AXIS2_PLACEMENT_3D ( 'NONE', #83677, #55755, #55292 ) ;
#63977 = CARTESIAN_POINT ( 'NONE',  ( 152.7546676148615745, 130.4533703983871931, 11.50000000000000000 ) ) ;
#63978 = CARTESIAN_POINT ( 'NONE',  ( -39.98770596539654321, -287.8809283587211780, -343.7603309726471821 ) ) ;
#63979 = CARTESIAN_POINT ( 'NONE',  ( 198.5368075633269314, 65.94727227685316961, -10.76536576713345994 ) ) ;
#63980 = CARTESIAN_POINT ( 'NONE',  ( -107.9231239757965568, -288.2232244667166015, -295.7237529994458214 ) ) ;
#63981 = CARTESIAN_POINT ( 'NONE',  ( -111.0357539742292801, -274.1079617381141134, -267.6306981556637652 ) ) ;
#63982 = CARTESIAN_POINT ( 'NONE',  ( -50.85340104127683247, -281.3080300680329060, -195.1544678121706511 ) ) ;
#63984 = CARTESIAN_POINT ( 'NONE',  ( -21.38821466200059263, -282.8419486104713769, -341.6485595088821583 ) ) ;
#63983 = CARTESIAN_POINT ( 'NONE',  ( -94.35395794113870238, -293.8921346682355988, -319.6359519670539271 ) ) ;
#63985 = CARTESIAN_POINT ( 'NONE',  ( -109.8515755478251776, -297.0458897517643777, -244.4513134462553694 ) ) ;
#63986 = CARTESIAN_POINT ( 'NONE',  ( -77.90965545200457143, -299.0167050613230799, -208.7778506104841085 ) ) ;
#63987 = CARTESIAN_POINT ( 'NONE',  ( 7.334211319854624378, -282.6608750085383122, -210.0548661866774864 ) ) ;
#63988 = CARTESIAN_POINT ( 'NONE',  ( -96.60585650401269220, -295.0104656711245639, -313.4077316617878068 ) ) ;
#63989 = DIRECTION ( 'NONE',  ( -0.000000000000000000, 0.000000000000000000, 1.000000000000000000 ) ) ;
#63990 = CARTESIAN_POINT ( 'NONE',  ( -37.51968410788270347, -285.0343163989131767, -345.0184190254362306 ) ) ;
#63991 = CARTESIAN_POINT ( 'NONE',  ( 216.5288609127277084, 293.9636489450776935, -40.00000000000000711 ) ) ;
#63992 = CARTESIAN_POINT ( 'NONE',  ( -20.25526795762938548, -286.3380690714490697, -345.3683826091709648 ) ) ;
#63993 = CARTESIAN_POINT ( 'NONE',  ( 38.97595581957405386, -274.8668436350243383, -279.7383590416616812 ) ) ;
#63994 = EDGE_CURVE ( 'NONE', #84679, #30244, #54930, .T. ) ;
#63995 = ADVANCED_FACE ( 'NONE', ( #58331 ), #71131, .F. ) ;
#63996 = CARTESIAN_POINT ( 'NONE',  ( 19.34713351667051384, -292.7345472496355683, -224.3481285050190195 ) ) ;
#63997 = CARTESIAN_POINT ( 'NONE',  ( 22.66693542582543586, -282.4803380483452315, -227.5864594530907254 ) ) ;
#63998 = CARTESIAN_POINT ( 'NONE',  ( 23.13297719271521302, -277.7367969593358907, -312.7484570792333329 ) ) ;
#63999 = AXIS2_PLACEMENT_3D ( 'NONE', #45513, #82457, #67339 ) ;
#64000 = CARTESIAN_POINT ( 'NONE',  ( -103.8948131869147034, -285.4852951630426787, -308.0087442827289124 ) ) ;
#64001 = CARTESIAN_POINT ( 'NONE',  ( 12.17331818995174331, -281.1395012102180999, -324.5403895253638211 ) ) ;
#64002 = CARTESIAN_POINT ( 'NONE',  ( -84.72036587700959842, -281.3998237883651541, -212.1538534874497941 ) ) ;
#64003 = CARTESIAN_POINT ( 'NONE',  ( -36.54062426294925103, -298.0619223292007973, -193.3611179782305101 ) ) ;
#64004 = CARTESIAN_POINT ( 'NONE',  ( 12.70300882681554810, -276.2095954623048328, -328.8805772256615114 ) ) ;
#64005 = CARTESIAN_POINT ( 'NONE',  ( 23.75612834044204291, -294.8907699401158879, -227.8137400918135427 ) ) ;
#64006 = DIRECTION ( 'NONE',  ( -1.000000000000000000, -0.000000000000000000, -0.000000000000000000 ) ) ;
#64007 = CARTESIAN_POINT ( 'NONE',  ( 152.4536156746142410, 275.0000000000000568, -14.50000000000000000 ) ) ;
#64008 = CARTESIAN_POINT ( 'NONE',  ( -108.6797376087111786, -295.0191204664316729, -244.8426954685156147 ) ) ;
#64009 = CARTESIAN_POINT ( 'NONE',  ( 22.51264878595645413, -275.6446592090524632, -312.3460000388446360 ) ) ;
#64010 = CARTESIAN_POINT ( 'NONE',  ( 22.63880648962044262, -295.7089856591564967, -317.5524876303701376 ) ) ;
#64011 = CARTESIAN_POINT ( 'NONE',  ( 37.37060531289780840, -294.5439271686976781, -253.3884559164038990 ) ) ;
#64012 = CARTESIAN_POINT ( 'NONE',  ( 31.11216437304329929, -289.9507104260557639, -300.7238162934110619 ) ) ;
#64013 = CARTESIAN_POINT ( 'NONE',  ( -57.10836075811388213, -275.3074325443680550, -342.5904730229486859 ) ) ;
#64014 = CARTESIAN_POINT ( 'NONE',  ( -24.04890530807592697, -278.8013690487071585, -343.6571236880507172 ) ) ;
#64015 = CARTESIAN_POINT ( 'NONE',  ( -58.84716550517746469, -293.4123591213312920, -341.6270225551393196 ) ) ;
#64016 = CARTESIAN_POINT ( 'NONE',  ( 25.24663991732245094, -282.8391641673076720, -227.5729509991774080 ) ) ;
#64017 = CARTESIAN_POINT ( 'NONE',  ( -83.83333562459020527, -284.3169095373505684, -213.6140109585516882 ) ) ;
#64018 = CARTESIAN_POINT ( 'NONE',  ( 155.5793399543505586, 205.2758529659251394, -216.3944369107308034 ) ) ;
#64019 = ORIENTED_EDGE ( 'NONE', *, *, #55446, .F. ) ;
#64020 = CARTESIAN_POINT ( 'NONE',  ( -110.1171876763455657, -284.1399445133095014, -276.3457565537390224 ) ) ;
#64021 = ORIENTED_EDGE ( 'NONE', *, *, #69913, .F. ) ;
#64022 = CARTESIAN_POINT ( 'NONE',  ( 26.47233443660443086, -283.1939359025325871, -312.8965326654148953 ) ) ;
#64023 = VECTOR ( 'NONE', #59632, 1000.000000000000000 ) ;
#64024 = CARTESIAN_POINT ( 'NONE',  ( -111.1132387943987396, -283.0871840292786032, -290.9952838733511271 ) ) ;
#64025 = CARTESIAN_POINT ( 'NONE',  ( -74.90329787781249138, -280.5057736683519352, -203.4137760814069225 ) ) ;
#64026 = CARTESIAN_POINT ( 'NONE',  ( -94.67693004519308886, -279.3846409035803049, -320.7136667173180058 ) ) ;
#64027 = CARTESIAN_POINT ( 'NONE',  ( 34.45848030099739390, -273.0523547857346784, -270.3937649182068412 ) ) ;
#64028 = CARTESIAN_POINT ( 'NONE',  ( 200.7966458510228449, 288.9840134172227408, -97.53539858349294889 ) ) ;
#64029 = AXIS2_PLACEMENT_3D ( 'NONE', #56496, #84865, #85807 ) ;
#64030 = CARTESIAN_POINT ( 'NONE',  ( 12.75541053804829161, -276.7526178115898006, -214.7008287420459567 ) ) ;
#64031 = CARTESIAN_POINT ( 'NONE',  ( -104.5909623734931273, -255.9058999860332335, -326.6256074632783566 ) ) ;
#64032 = CARTESIAN_POINT ( 'NONE',  ( -62.84780177995892814, -277.7387112948403001, -200.1546915667861981 ) ) ;
#64033 = CARTESIAN_POINT ( 'NONE',  ( -40.61154822904870088, -293.7717267207963801, -194.4318258477070174 ) ) ;
#64034 = CARTESIAN_POINT ( 'NONE',  ( 18.90622322352169959, -293.5620600956856379, -317.0522711826295676 ) ) ;
#64035 = CARTESIAN_POINT ( 'NONE',  ( -51.67998891948372631, -288.7385239450921972, -345.9517283624059019 ) ) ;
#64036 = DIRECTION ( 'NONE',  ( 0.000000000000000000, 0.000000000000000000, 1.000000000000000000 ) ) ;
#64038 = CARTESIAN_POINT ( 'NONE',  ( -1.783228305354786603, -284.9310473934086758, -205.6351137785605658 ) ) ;
#64037 = CARTESIAN_POINT ( 'NONE',  ( -47.57079430274748688, -293.7544940496728145, -346.0841126684085793 ) ) ;
#64039 = CARTESIAN_POINT ( 'NONE',  ( -68.33817933045455106, -293.5010254382592052, -202.8928401261020440 ) ) ;
#64040 = CARTESIAN_POINT ( 'NONE',  ( -27.72710760521565376, -284.6563443067515209, -197.2976704723051569 ) ) ;
#64041 = CARTESIAN_POINT ( 'NONE',  ( -7.034914135984592143, -283.9611432629989167, -337.3282096492065989 ) ) ;
#64042 = VERTEX_POINT ( 'NONE', #50261 ) ;
#64043 = CARTESIAN_POINT ( 'NONE',  ( -86.37198769585229741, -292.3321923883326008, -211.2255915447739483 ) ) ;
#64044 = CIRCLE ( 'NONE', #73135, 4.025000000000000355 ) ;
#64045 = CARTESIAN_POINT ( 'NONE',  ( 33.17132662052006253, -281.7914566761671153, -251.1847165259451629 ) ) ;
#64046 = CARTESIAN_POINT ( 'NONE',  ( -13.91812492433534842, -293.5497350752999068, -343.2949567851319443 ) ) ;
#64047 = CARTESIAN_POINT ( 'NONE',  ( 36.23373874178597021, -288.6341432698250173, -292.5611506483164703 ) ) ;
#64048 = CARTESIAN_POINT ( 'NONE',  ( -40.33008639354127212, -289.5810883632068453, -347.2545928553726640 ) ) ;
#64049 = CARTESIAN_POINT ( 'NONE',  ( 23.51067020293623244, -288.2786349373474195, -310.7075053992594462 ) ) ;
#64050 = ORIENTED_EDGE ( 'NONE', *, *, #36204, .F. ) ;
#64051 = CARTESIAN_POINT ( 'NONE',  ( 196.9534188175200029, 25.84350552936208700, 12.42857142857141994 ) ) ;
#64052 = CARTESIAN_POINT ( 'NONE',  ( 24.71674628524373674, -295.9968793596246428, -313.8470264043663747 ) ) ;
#64053 = AXIS2_PLACEMENT_3D ( 'NONE', #53072, #66827, #89985 ) ;
#64054 = CARTESIAN_POINT ( 'NONE',  ( -111.1418765721582389, -295.4934666835799248, -249.9954375051690931 ) ) ;
#64055 = CARTESIAN_POINT ( 'NONE',  ( -92.91297942904134288, -276.9339945138503367, -318.0606081844316577 ) ) ;
#64056 = CARTESIAN_POINT ( 'NONE',  ( -67.50573499266110389, -273.1745731492483173, -199.5821811154191039 ) ) ;
#64057 = CARTESIAN_POINT ( 'NONE',  ( -50.61490697035502251, -293.7046267835437448, -342.8492530863629781 ) ) ;
#64058 = CARTESIAN_POINT ( 'NONE',  ( 27.51382453650762372, -276.8305632108537679, -234.5929674519288142 ) ) ;
#64059 = CARTESIAN_POINT ( 'NONE',  ( 9.759455282733700443, -296.8894988464056723, -196.3621327438673347 ) ) ;
#64060 = CARTESIAN_POINT ( 'NONE',  ( -45.11762753652972435, -296.3577559014474900, -343.3958771987321938 ) ) ;
#64061 = CARTESIAN_POINT ( 'NONE',  ( -97.42888997956573860, -297.0486816243500243, -312.3582094261772113 ) ) ;
#64062 = DIRECTION ( 'NONE',  ( -0.000000000000000000, -1.000000000000000000, -0.000000000000000000 ) ) ;
#64063 = CARTESIAN_POINT ( 'NONE',  ( -30.64079257569892789, -296.5688866449104921, -346.2659152823010800 ) ) ;
#64064 = AXIS2_PLACEMENT_3D ( 'NONE', #82311, #17461, #46311 ) ;
#64065 = CARTESIAN_POINT ( 'NONE',  ( -109.8309105504848588, -294.2968592590907519, -290.2443471237517656 ) ) ;
#64066 = CARTESIAN_POINT ( 'NONE',  ( -36.19461568192025425, -298.7175698476569892, -193.4629270313071174 ) ) ;
#64067 = CARTESIAN_POINT ( 'NONE',  ( -110.9567690822490391, -289.1521649065282986, -268.4283185786113108 ) ) ;
#64068 = CARTESIAN_POINT ( 'NONE',  ( -100.9908986399047706, -275.0852220119529079, -230.6902196267084832 ) ) ;
#64069 = CARTESIAN_POINT ( 'NONE',  ( -94.10410378094181283, -273.7516478925962815, -218.4036583419192823 ) ) ;
#64070 = CARTESIAN_POINT ( 'NONE',  ( -110.1199159360397459, -296.7991256590588591, -276.9057601707949061 ) ) ;
#64071 = CARTESIAN_POINT ( 'NONE',  ( -17.45094494918996020, -282.2874648003502216, -197.6784882941391004 ) ) ;
#64072 = CARTESIAN_POINT ( 'NONE',  ( -7.712410511587266093, -279.1172581008897851, -199.8103649508600768 ) ) ;
#64073 = CIRCLE ( 'NONE', #509, 2.000000000000000000 ) ;
#64074 = CARTESIAN_POINT ( 'NONE',  ( -24.55870517756808624, -282.2418420497596685, -346.2433080362148985 ) ) ;
#64075 = CARTESIAN_POINT ( 'NONE',  ( 39.60530611315584792, -274.9109805147836596, -271.1788498611365981 ) ) ;
#64076 = CARTESIAN_POINT ( 'NONE',  ( 36.21813101987581973, -279.6998352095608880, -250.4271280434108746 ) ) ;
#64077 = CARTESIAN_POINT ( 'NONE',  ( -94.49484596136692005, -277.2268040602398855, -221.5197803589919374 ) ) ;
#64078 = CARTESIAN_POINT ( 'NONE',  ( -33.99587345615407230, -272.6697835427397649, -196.8479874408589581 ) ) ;
#64079 = CARTESIAN_POINT ( 'NONE',  ( 34.28744386409212552, -277.2636364680579959, -247.9591903884178805 ) ) ;
#64080 = DIRECTION ( 'NONE',  ( 0.000000000000000000, 1.000000000000000000, 0.000000000000000000 ) ) ;
#64081 = CARTESIAN_POINT ( 'NONE',  ( 153.1901962297479827, 19.73438857712018901, 11.80184082122065981 ) ) ;
#64082 = CARTESIAN_POINT ( 'NONE',  ( -112.7495695017638297, -271.0950597997922387, -259.0431613161582050 ) ) ;
#64083 = CARTESIAN_POINT ( 'NONE',  ( -50.25907620316200308, -289.9081487786675098, -196.1213160197946195 ) ) ;
#64084 = CARTESIAN_POINT ( 'NONE',  ( -61.68858096559480231, -291.7444573679159134, -197.2554614762791800 ) ) ;
#64085 = CARTESIAN_POINT ( 'NONE',  ( 36.38915228898011378, -277.7396327998554852, -284.9826716471279724 ) ) ;
#64086 = CARTESIAN_POINT ( 'NONE',  ( 29.65909608989104029, -273.1067905970684251, -236.6580921268214013 ) ) ;
#64087 = DIRECTION ( 'NONE',  ( -0.6056179655966483777, 0.7957555401921981852, 0.000000000000000000 ) ) ;
#64088 = CARTESIAN_POINT ( 'NONE',  ( -34.50802493472657062, -284.9369429686649937, -345.8679685675796804 ) ) ;
#64089 =( NAMED_UNIT ( * ) PLANE_ANGLE_UNIT ( ) SI_UNIT ( $, .RADIAN. ) );
#64090 = CARTESIAN_POINT ( 'NONE',  ( -16.85317983714815782, -284.3164602854000123, -198.1605061003254491 ) ) ;
#64091 = CARTESIAN_POINT ( 'NONE',  ( 156.1449889021179160, 250.0000000000000568, 16.91223866672558529 ) ) ;
#64092 = CARTESIAN_POINT ( 'NONE',  ( 28.74543454758475036, -292.7782742620349836, -302.4097828290336452 ) ) ;
#64093 = CARTESIAN_POINT ( 'NONE',  ( -10.27795049251010440, -284.5487136744127383, -201.2212522984016516 ) ) ;
#64094 = CARTESIAN_POINT ( 'NONE',  ( 157.3189109369757261, 16.43186977800929682, -7.221609175748580967 ) ) ;
#64095 = CARTESIAN_POINT ( 'NONE',  ( -68.13914373595406460, -293.4563744259562554, -338.7602745174829693 ) ) ;
#64096 = CARTESIAN_POINT ( 'NONE',  ( -109.3168021589384580, -283.3546573709051586, -245.0176288876326964 ) ) ;
#64097 = CARTESIAN_POINT ( 'NONE',  ( -96.26263673611968841, -280.7699506527359858, -225.9018216441143636 ) ) ;
#64098 = CARTESIAN_POINT ( 'NONE',  ( -75.92008999479128306, -286.7543915711464138, -204.1206009370356185 ) ) ;
#64099 = CARTESIAN_POINT ( 'NONE',  ( 21.72128077065429252, -280.4418637209396366, -318.1889431672349247 ) ) ;
#64100 = CARTESIAN_POINT ( 'NONE',  ( 18.66176132030001966, -286.8873174291267105, -223.5163052786766116 ) ) ;
#64101 = CIRCLE ( 'NONE', #61033, 1.895975569037589015 ) ;
#64102 = CARTESIAN_POINT ( 'NONE',  ( -87.48386711921313008, -279.1938344061942985, -324.2233311327559022 ) ) ;
#64103 = CARTESIAN_POINT ( 'NONE',  ( -109.1999551214033346, -279.1731650636668860, -284.1747338502843832 ) ) ;
#64104 = EDGE_CURVE ( 'NONE', #71459, #25330, #35276, .T. ) ;
#64105 = CARTESIAN_POINT ( 'NONE',  ( -101.1396447034011459, -287.0686075209389401, -230.2583865339261706 ) ) ;
#64106 = EDGE_LOOP ( 'NONE', ( #66022, #22538, #13152, #55740, #32082, #73437, #62572, #71019, #13948, #23675, #9329, #82976, #55760, #65216, #66925, #91784, #8671, #46349, #27561, #5082, #53468, #30786 ) ) ;
#64107 = AXIS2_PLACEMENT_3D ( 'NONE', #3220, #19763, #61007 ) ;
#64108 = CARTESIAN_POINT ( 'NONE',  ( 76.38888381899823798, -299.2725563385990313, -193.3641481775453030 ) ) ;
#64109 = CARTESIAN_POINT ( 'NONE',  ( -45.51812760638178901, -291.1361767615164808, -344.5567569070808531 ) ) ;
#64110 = LINE ( 'NONE', #56995, #33672 ) ;
#64111 = CARTESIAN_POINT ( 'NONE',  ( -37.37352853689063181, -288.5519495502701375, -190.3611179825600175 ) ) ;
#64112 = ORIENTED_EDGE ( 'NONE', *, *, #70761, .F. ) ;
#64113 = CARTESIAN_POINT ( 'NONE',  ( -8.373007603888428463, -272.4302129317083541, -200.9456157213863889 ) ) ;
#64114 = ADVANCED_FACE ( 'NONE', ( #43626 ), #42726, .T. ) ;
#64115 = CARTESIAN_POINT ( 'NONE',  ( 38.43290177078794301, -291.8442865830637629, -261.8358771370611180 ) ) ;
#64116 = CARTESIAN_POINT ( 'NONE',  ( -106.3999656180249787, -272.2191569659897823, -246.3851167392122363 ) ) ;
#64117 = VECTOR ( 'NONE', #9654, 1000.000000000000114 ) ;
#64118 = CARTESIAN_POINT ( 'NONE',  ( 26.96301397165637681, -288.5832952640606663, -234.2621550006503810 ) ) ;
#64119 = PRODUCT ( 'L sheet band', 'L sheet band', '', ( #61102 ) ) ;
#64120 = CARTESIAN_POINT ( 'NONE',  ( -35.66196617530688684, -281.8336211531368463, -196.3542691956220665 ) ) ;
#64121 = CARTESIAN_POINT ( 'NONE',  ( -20.60763271351048687, -290.2667648619270722, -344.9712368994705116 ) ) ;
#64122 = CARTESIAN_POINT ( 'NONE',  ( -51.57702298160149468, -290.5457542013245984, -345.5319491256747710 ) ) ;
#64123 = CARTESIAN_POINT ( 'NONE',  ( -94.94216819528982398, -285.8888655504377425, -318.3943016243790680 ) ) ;
#64124 = CARTESIAN_POINT ( 'NONE',  ( -108.5134651390332579, -279.0923283651503084, -240.9743884994499012 ) ) ;
#64125 = VERTEX_POINT ( 'NONE', #16611 ) ;
#64126 = CARTESIAN_POINT ( 'NONE',  ( 25.30393350620322934, -292.1992669785503267, -312.6084703810788596 ) ) ;
#64127 = CARTESIAN_POINT ( 'NONE',  ( 23.74860176744353879, -280.7600081435238621, -223.4676775841971335 ) ) ;
#64128 = AXIS2_PLACEMENT_3D ( 'NONE', #27012, #32717, #92327 ) ;
#64129 = CARTESIAN_POINT ( 'NONE',  ( -49.09395476328017338, -275.7613928792315505, -197.0100318913119395 ) ) ;
#64130 = VECTOR ( 'NONE', #19727, 1000.000000000000000 ) ;
#64131 = CARTESIAN_POINT ( 'NONE',  ( 27.36219212280431989, -284.4805209788416391, -301.4846348637938149 ) ) ;
#64132 = CARTESIAN_POINT ( 'NONE',  ( 0.5223785719801525840, -274.7950237270176217, -336.3016355121197307 ) ) ;
#64133 = DIRECTION ( 'NONE',  ( -1.000000000000000000, 0.000000000000000000, 0.000000000000000000 ) ) ;
#64134 = CARTESIAN_POINT ( 'NONE',  ( 34.39586063615828948, -280.8764366924675073, -256.4492124749717732 ) ) ;
#64135 = CIRCLE ( 'NONE', #73152, 4.999999999999984013 ) ;
#64136 = CARTESIAN_POINT ( 'NONE',  ( -35.70453050172395848, -278.2371448505144258, -346.9596057014061898 ) ) ;
#64137 = CARTESIAN_POINT ( 'NONE',  ( -95.01002813568375416, -274.5058871928542317, -224.8022832246770406 ) ) ;
#64138 = CARTESIAN_POINT ( 'NONE',  ( -63.11113020456068767, -284.7833028981650045, -198.0509756357190270 ) ) ;
#64139 = CARTESIAN_POINT ( 'NONE',  ( -109.4193708314066527, -292.5318094380201615, -253.4896129621295131 ) ) ;
#64140 = CARTESIAN_POINT ( 'NONE',  ( -111.0497545917288562, -274.3990843985011452, -250.8311926227954700 ) ) ;
#64141 = CARTESIAN_POINT ( 'NONE',  ( -18.68653884735005377, -275.6025648677230038, -196.1088475022184241 ) ) ;
#64142 = DIRECTION ( 'NONE',  ( 0.000000000000000000, 0.000000000000000000, 1.000000000000000000 ) ) ;
#64143 = CARTESIAN_POINT ( 'NONE',  ( -38.34187344849005541, -297.0648776316222666, -345.1877715485082945 ) ) ;
#64144 = CARTESIAN_POINT ( 'NONE',  ( -81.73367015924681311, -281.6575907616522727, -330.6699517919837490 ) ) ;
#64145 = CARTESIAN_POINT ( 'NONE',  ( -112.5455963616639821, -290.0132706360507768, -286.7963935490153062 ) ) ;
#64146 = CARTESIAN_POINT ( 'NONE',  ( 16.65362924848868076, -272.8445629385341817, -218.7464661296594386 ) ) ;
#64147 = CARTESIAN_POINT ( 'NONE',  ( -23.94677231391226258, -287.8205023179548903, -195.2940260259423724 ) ) ;
#64148 = CARTESIAN_POINT ( 'NONE',  ( -64.17199378851334757, -290.6140415434508100, -202.1246483527534394 ) ) ;
#64149 = EDGE_LOOP ( 'NONE', ( #54189, #89787, #42196, #42281 ) ) ;
#64150 = CARTESIAN_POINT ( 'NONE',  ( -113.6636412024419371, -289.0804598119637490, -274.0445405853442935 ) ) ;
#64151 = CARTESIAN_POINT ( 'NONE',  ( -103.5737144329234809, -290.6337978217831051, -239.6136340562024998 ) ) ;
#64152 = ORIENTED_EDGE ( 'NONE', *, *, #49892, .F. ) ;
#64153 = CARTESIAN_POINT ( 'NONE',  ( 24.44603737428095158, -288.0259312057053762, -224.9324045427470367 ) ) ;
#64154 = CARTESIAN_POINT ( 'NONE',  ( -1.456138070629751091, -276.8959523008033443, -334.0132580270123412 ) ) ;
#64155 = CARTESIAN_POINT ( 'NONE',  ( -66.81839121405472781, -294.3497582806576816, -341.1751028590360306 ) ) ;
#64156 = CARTESIAN_POINT ( 'NONE',  ( -112.1180784621771807, -284.9782148037290312, -288.3557872313729717 ) ) ;
#64157 = CARTESIAN_POINT ( 'NONE',  ( -63.19832814098982965, -286.0576305887619242, -197.8547108223011151 ) ) ;
#64158 = CARTESIAN_POINT ( 'NONE',  ( -2.414817773127506673, -282.9098542242265921, -334.5018523341619812 ) ) ;
#64159 = CARTESIAN_POINT ( 'NONE',  ( -95.55820914780639441, -240.1411278548074790, -341.8388433382354492 ) ) ;
#64160 = CARTESIAN_POINT ( 'NONE',  ( 83.14950132131733085, 83.50475598798475119, -301.0942469162992552 ) ) ;
#64161 = CARTESIAN_POINT ( 'NONE',  ( -108.4024080554443685, -263.9389858668760098, -305.3879311740210483 ) ) ;
#64162 = AXIS2_PLACEMENT_3D ( 'NONE', #4459, #12032, #92488 ) ;
#64163 = CARTESIAN_POINT ( 'NONE',  ( 94.64983258005516120, -299.0959783674220489, -197.2743889382824136 ) ) ;
#64164 = CARTESIAN_POINT ( 'NONE',  ( 3.111926770055553515, -273.5295774831445215, -209.1634642982251648 ) ) ;
#64165 = CARTESIAN_POINT ( 'NONE',  ( -56.06138294541747058, -294.7946736442961537, -344.9875233514065940 ) ) ;
#64166 = CARTESIAN_POINT ( 'NONE',  ( 189.9032515046773426, 267.9733876889036992, -137.7336960540900179 ) ) ;
#64167 = CARTESIAN_POINT ( 'NONE',  ( 11.48393226028832537, -273.3975359398546630, -211.3910257787479736 ) ) ;
#64168 = CARTESIAN_POINT ( 'NONE',  ( -90.95405900927855214, -299.1418721902680318, -218.9398833114676108 ) ) ;
#64169 = CARTESIAN_POINT ( 'NONE',  ( 14.44265908629642503, -289.6200214537574880, -322.5111287044948085 ) ) ;
#64170 = CARTESIAN_POINT ( 'NONE',  ( -94.54069347392442069, -292.2773046407779702, -224.4881264791785043 ) ) ;
#64171 = EDGE_LOOP ( 'NONE', ( #62503, #14533, #30920, #27066 ) ) ;
#64172 = CARTESIAN_POINT ( 'NONE',  ( -111.3982813257405553, -297.7495281497535871, -249.9546102785856192 ) ) ;
#64173 = CARTESIAN_POINT ( 'NONE',  ( 25.75235456114296184, -288.5509133476144257, -307.3003775568747642 ) ) ;
#64174 = CARTESIAN_POINT ( 'NONE',  ( -8.439268677859162793, -295.4862593265058877, -341.6130484505632126 ) ) ;
#64175 = CARTESIAN_POINT ( 'NONE',  ( -24.91157101875893787, -295.3901541695384481, -346.3428619613575847 ) ) ;
#64176 = CARTESIAN_POINT ( 'NONE',  ( 6.674552539915903360, -292.8366658984132300, -212.1239347956079655 ) ) ;
#64177 = VERTEX_POINT ( 'NONE', #22780 ) ;
#64178 = CARTESIAN_POINT ( 'NONE',  ( 4.053434315715206182, -276.5248458520289887, -207.0870505141138551 ) ) ;
#64179 = VERTEX_POINT ( 'NONE', #68210 ) ;
#64180 = CARTESIAN_POINT ( 'NONE',  ( -113.1747728713155681, -278.2224583963825353, -257.3660426985651384 ) ) ;
#64181 = AXIS2_PLACEMENT_3D ( 'NONE', #15830, #72654, #59384 ) ;
#64182 = CARTESIAN_POINT ( 'NONE',  ( 23.24025661270209042, -275.9227109005238390, -229.1896928347936750 ) ) ;
#64183 = CARTESIAN_POINT ( 'NONE',  ( -38.36652684107135514, -275.7996055204619097, -194.3813591825203844 ) ) ;
#64184 = CARTESIAN_POINT ( 'NONE',  ( -2.256388939355643330, -274.6102226422161152, -337.0501556438189823 ) ) ;
#64185 = CARTESIAN_POINT ( 'NONE',  ( -110.4764251979117944, -297.2249395151284261, -268.7389001083938638 ) ) ;
#64186 = CARTESIAN_POINT ( 'NONE',  ( -109.6210102986301251, -295.3086423271090553, -256.4710576432662492 ) ) ;
#64187 = DIRECTION ( 'NONE',  ( 0.000000000000000000, 0.000000000000000000, 1.000000000000000000 ) ) ;
#64188 = CARTESIAN_POINT ( 'NONE',  ( -112.7320693007894477, -278.8514755870729118, -285.7826048526360410 ) ) ;
#64189 = CARTESIAN_POINT ( 'NONE',  ( -51.27880630789400840, -277.4020189159596725, -342.0183372686629468 ) ) ;
#64190 = CIRCLE ( 'NONE', #83792, 161.1282194813176716 ) ;
#64191 = EDGE_CURVE ( 'NONE', #4620, #56700, #15716, .T. ) ;
#64192 = CARTESIAN_POINT ( 'NONE',  ( -4.967305565061796990, -285.1543945540529990, -201.0415907810293277 ) ) ;
#64193 = CARTESIAN_POINT ( 'NONE',  ( -111.1060785622191105, -274.7299603217629738, -256.5254225831626513 ) ) ;
#64194 = CARTESIAN_POINT ( 'NONE',  ( 82.67382771687083221, -297.5965108451826495, -196.9258814007443164 ) ) ;
#64195 = AXIS2_PLACEMENT_3D ( 'NONE', #41070, #63387, #48664 ) ;
#64196 = CARTESIAN_POINT ( 'NONE',  ( 35.15758019924837896, -286.6151680731373972, -260.1694962532299655 ) ) ;
#64197 = TOROIDAL_SURFACE ( 'NONE', #61186, 24.50000000000000355, 0.5000000000000000000 ) ;
#64198 = CARTESIAN_POINT ( 'NONE',  ( -54.70912216946552320, -278.0658703971398040, -198.3613683552276825 ) ) ;
#64199 = CARTESIAN_POINT ( 'NONE',  ( -104.9765451648991217, -277.5133190422906182, -241.3627964370480754 ) ) ;
#64200 = CARTESIAN_POINT ( 'NONE',  ( -112.1687648118101777, -286.6267572425494450, -264.5634801422433497 ) ) ;
#64201 = CARTESIAN_POINT ( 'NONE',  ( -36.44601420421265203, -278.2457939693624098, -343.7652617077954460 ) ) ;
#64202 = CARTESIAN_POINT ( 'NONE',  ( 154.5625123364532101, 250.5000000000000568, 13.15740740740741899 ) ) ;
#64204 = CARTESIAN_POINT ( 'NONE',  ( -14.91050453446275981, -275.0054705135414110, -343.0165856159265445 ) ) ;
#64203 = AXIS2_PLACEMENT_3D ( 'NONE', #41282, #13385, #63125 ) ;
#64205 = CARTESIAN_POINT ( 'NONE',  ( -35.39591681071548379, -274.7285963412398360, -197.2725621310013366 ) ) ;
#64206 = CARTESIAN_POINT ( 'NONE',  ( 21.97232724543506421, -284.1843652723520677, -316.5541535020900028 ) ) ;
#64207 = CARTESIAN_POINT ( 'NONE',  ( 151.4851178187871312, 21.00000000000000000, 0.000000000000000000 ) ) ;
#64208 = CARTESIAN_POINT ( 'NONE',  ( -34.69235685029834571, -290.9392521634806599, -345.8746610110567872 ) ) ;
#64209 = CARTESIAN_POINT ( 'NONE',  ( -41.33907348793265157, -290.0016848261755626, -195.4550004045474338 ) ) ;
#64210 = CIRCLE ( 'NONE', #47518, 1.000000000000002887 ) ;
#64211 = CARTESIAN_POINT ( 'NONE',  ( 82.16888074921301666, -297.9818618066009321, -196.6132423200940309 ) ) ;
#64212 = CARTESIAN_POINT ( 'NONE',  ( -65.99003948167957390, -272.3540516583252611, -202.6816075593507378 ) ) ;
#64213 = CARTESIAN_POINT ( 'NONE',  ( 5.231080707489677906, -290.7739821697912816, -209.4834224960733025 ) ) ;
#64214 = CARTESIAN_POINT ( 'NONE',  ( 5.045406874201050940, -57.93311274753654061, -355.0152878038887820 ) ) ;
#64215 = CARTESIAN_POINT ( 'NONE',  ( -84.74921204074180991, -288.1716340090512745, -330.2218208164943576 ) ) ;
#64216 = CARTESIAN_POINT ( 'NONE',  ( -102.4677188092241948, -285.6830467179824495, -305.1835442133593119 ) ) ;
#64217 = CARTESIAN_POINT ( 'NONE',  ( 37.29907017803776625, -285.6115715254599081, -256.1228096611766318 ) ) ;
#64218 = CARTESIAN_POINT ( 'NONE',  ( -70.46400878843198257, -284.9228875084473316, -336.0888868238830014 ) ) ;
#64219 = CARTESIAN_POINT ( 'NONE',  ( -38.87824176622038408, -283.8747153740139311, -343.5189766448566502 ) ) ;
#64220 = ADVANCED_FACE ( 'NONE', ( #88092 ), #67290, .T. ) ;
#64221 = CARTESIAN_POINT ( 'NONE',  ( -58.50150318363142787, -293.7597959895502981, -198.0377501480702733 ) ) ;
#64222 = CARTESIAN_POINT ( 'NONE',  ( 31.25621102938738716, -273.2175486719318656, -238.5561439389797158 ) ) ;
#64223 = CARTESIAN_POINT ( 'NONE',  ( -27.00356244762539148, -274.5133106973700592, -194.0262031553308191 ) ) ;
#64224 = CARTESIAN_POINT ( 'NONE',  ( -105.9426017625730765, -289.0463512551486360, -238.5627326758650781 ) ) ;
#64225 = CARTESIAN_POINT ( 'NONE',  ( -14.58969424671998993, -276.7653283119158232, -343.9787966223019566 ) ) ;
#64226 = CARTESIAN_POINT ( 'NONE',  ( -7.303795217128174144, -296.6361658221218249, -338.7092637295635313 ) ) ;
#64227 = FACE_OUTER_BOUND ( 'NONE', #48614, .T. ) ;
#64228 = CARTESIAN_POINT ( 'NONE',  ( -110.4542110544635705, -298.8376638359844719, -287.0812184334320705 ) ) ;
#64229 = CARTESIAN_POINT ( 'NONE',  ( -104.5711279879627256, -282.8401187109731154, -300.0502996197664629 ) ) ;
#64230 = CARTESIAN_POINT ( 'NONE',  ( -42.27245524331343773, -277.9898048301911331, -195.5233714658876067 ) ) ;
#64231 = DIRECTION ( 'NONE',  ( 1.000000000000000000, 4.095251346825557639E-15, 0.000000000000000000 ) ) ;
#64232 = CARTESIAN_POINT ( 'NONE',  ( -109.4403766833796396, -271.3499589852424947, -245.3713482571579618 ) ) ;
#64233 = CARTESIAN_POINT ( 'NONE',  ( -103.2264729059779853, -277.4714475034114116, -302.1498597302763187 ) ) ;
#64234 = CARTESIAN_POINT ( 'NONE',  ( 18.99422663204113348, -294.4036296195081377, -222.8535279554371300 ) ) ;
#64235 = CARTESIAN_POINT ( 'NONE',  ( -17.06045176701547206, -279.2283937203210940, -196.4005644837530440 ) ) ;
#64236 = CARTESIAN_POINT ( 'NONE',  ( 30.80890949115166677, -294.8524572014763407, -297.3122901895367249 ) ) ;
#64237 = CARTESIAN_POINT ( 'NONE',  ( -81.57285785805777323, -296.9550445901002718, -332.8509930598797268 ) ) ;
#64238 = CARTESIAN_POINT ( 'NONE',  ( -70.46565135321603179, -297.4361464178937808, -205.2948902160746911 ) ) ;
#64239 = CARTESIAN_POINT ( 'NONE',  ( -42.78430026052969737, -291.1208601633182411, -345.2153724069146392 ) ) ;
#64240 = CARTESIAN_POINT ( 'NONE',  ( -89.88779501488360779, -285.5016321290386259, -214.0044260576217710 ) ) ;
#64241 = CARTESIAN_POINT ( 'NONE',  ( -55.02201972861390544, -271.9667315955380218, -196.6881122300655136 ) ) ;
#64242 = CARTESIAN_POINT ( 'NONE',  ( 35.84969678633999735, -287.0826467082037539, -246.2736572080849839 ) ) ;
#64243 = CARTESIAN_POINT ( 'NONE',  ( -109.2085981721099159, -280.7933829587623791, -250.1395495399056301 ) ) ;
#64244 = EDGE_CURVE ( 'NONE', #42782, #47679, #45466, .T. ) ;
#64245 = CARTESIAN_POINT ( 'NONE',  ( -10.65309267712260777, -285.4677292894647280, -202.1483782838506613 ) ) ;
#64246 = CARTESIAN_POINT ( 'NONE',  ( -106.9519126385471424, -288.1882506219339461, -298.2791938581951854 ) ) ;
#64247 = CARTESIAN_POINT ( 'NONE',  ( 85.37101130053461873, 80.99577858023421584, -298.5812782549759845 ) ) ;
#64248 = CARTESIAN_POINT ( 'NONE',  ( 9.074412919876589712, -286.2172963857036621, -213.9383132758052568 ) ) ;
#64249 = CARTESIAN_POINT ( 'NONE',  ( 33.35393457074724211, -282.8768350914514258, -300.4125903019410657 ) ) ;
#64250 = EDGE_CURVE ( 'NONE', #27807, #18158, #9966, .T. ) ;
#64251 = CARTESIAN_POINT ( 'NONE',  ( -56.11959337319295571, -290.8748872662643521, -195.8737470019289333 ) ) ;
#64252 = CARTESIAN_POINT ( 'NONE',  ( -90.51467456775094433, -280.9146923019625888, -215.7066333863451746 ) ) ;
#64253 = CARTESIAN_POINT ( 'NONE',  ( -104.3696486666726599, -280.3481382597793186, -233.4754515755964519 ) ) ;
#64254 = CARTESIAN_POINT ( 'NONE',  ( 35.51999108845736686, -281.3262201609597355, -265.8695750903006001 ) ) ;
#64255 = CARTESIAN_POINT ( 'NONE',  ( 24.69264436449613243, -276.9814485151051713, -228.1866902967092869 ) ) ;
#64256 = CARTESIAN_POINT ( 'NONE',  ( 19.52968153547678298, -294.2585922463209727, -322.3487600808773550 ) ) ;
#64257 = CARTESIAN_POINT ( 'NONE',  ( 8.981391797661739673, -286.4329754034737334, -328.8933138579299111 ) ) ;
#64258 = CARTESIAN_POINT ( 'NONE',  ( -73.07676811720180865, -293.1867500357013228, -203.0452172305451768 ) ) ;
#64259 = CARTESIAN_POINT ( 'NONE',  ( -90.25951223309061788, -296.2022589853284558, -219.5545602154507776 ) ) ;
#64260 = ORIENTED_EDGE ( 'NONE', *, *, #9747, .T. ) ;
#64261 = CARTESIAN_POINT ( 'NONE',  ( -51.26369735830706276, -285.1515284000663542, -343.5402582968472984 ) ) ;
#64262 = CARTESIAN_POINT ( 'NONE',  ( -98.75338481821634673, -295.6711950852856603, -309.9593555270666911 ) ) ;
#64263 = CARTESIAN_POINT ( 'NONE',  ( -2.209742686731688277, -293.5857512618093210, -202.1757467171505880 ) ) ;
#64264 = CONICAL_SURFACE ( 'NONE', #86914, 8.550761578869359170, 0.7853981633974639331 ) ;
#64265 = CARTESIAN_POINT ( 'NONE',  ( -2.372615935219600125, -283.2279348621967188, -334.5708781241722818 ) ) ;
#64266 = CARTESIAN_POINT ( 'NONE',  ( 26.74075959475894138, -274.0534428312576551, -228.0969656936518390 ) ) ;
#64267 = CARTESIAN_POINT ( 'NONE',  ( -65.40208670600769381, -290.0607710452212586, -342.0129663199547281 ) ) ;
#64268 = CARTESIAN_POINT ( 'NONE',  ( -108.1570458389323903, -282.3435728532241455, -297.4423969224559414 ) ) ;
#64269 = CARTESIAN_POINT ( 'NONE',  ( -100.6607907529931083, -290.3071342874925449, -314.1382473307544956 ) ) ;
#64270 = CARTESIAN_POINT ( 'NONE',  ( 33.72991039674568725, -287.6636870339884240, -253.5466128749491759 ) ) ;
#64271 = CARTESIAN_POINT ( 'NONE',  ( 208.4306832106271088, -74.55766379199613425, 7.500000000000013323 ) ) ;
#64272 = CARTESIAN_POINT ( 'NONE',  ( 202.2090562182569613, 292.1033822784109475, -53.99999999998392042 ) ) ;
#64273 = CARTESIAN_POINT ( 'NONE',  ( -95.95921662488163406, -276.6952119285918457, -223.5744983911110353 ) ) ;
#64274 = CARTESIAN_POINT ( 'NONE',  ( -83.53178740183430762, -278.5972817326481277, -213.5586391358351932 ) ) ;
#64275 = VERTEX_POINT ( 'NONE', #60185 ) ;
#64276 = CARTESIAN_POINT ( 'NONE',  ( 2.885043427152404583, -279.5260208023804580, -209.0136983235933030 ) ) ;
#64277 = CARTESIAN_POINT ( 'NONE',  ( 39.53348774345503358, -275.1573764929423760, -265.4453586957677658 ) ) ;
#64278 = CARTESIAN_POINT ( 'NONE',  ( 175.3651808782167620, 240.6162257589489286, -178.0254516555434350 ) ) ;
#64279 = CARTESIAN_POINT ( 'NONE',  ( -33.92333132851602073, -278.6691002554712213, -194.0268461996747931 ) ) ;
#64280 = CARTESIAN_POINT ( 'NONE',  ( -56.77077590340982738, -281.3240102541504370, -342.4330113552243233 ) ) ;
#64281 = CARTESIAN_POINT ( 'NONE',  ( -111.6099308129362129, -298.1086455285047805, -286.4298431388921244 ) ) ;
#64282 = AXIS2_PLACEMENT_3D ( 'NONE', #60143, #81883, #80970 ) ;
#64283 = CARTESIAN_POINT ( 'NONE',  ( 35.59567580923845043, -293.9778711251062759, -265.3058431170756535 ) ) ;
#64284 = ORIENTED_EDGE ( 'NONE', *, *, #38735, .F. ) ;
#64285 = CARTESIAN_POINT ( 'NONE',  ( -84.13019986963037411, -290.0778094746079319, -213.6859049832245034 ) ) ;
#64286 = CARTESIAN_POINT ( 'NONE',  ( -44.04215518520750550, -274.6210908728622826, -193.7022882765053566 ) ) ;
#64287 = CARTESIAN_POINT ( 'NONE',  ( -35.14989057605235701, -298.2470232487723933, -197.3610538051364642 ) ) ;
#64288 = VERTEX_POINT ( 'NONE', #15689 ) ;
#64289 = DIRECTION ( 'NONE',  ( 0.000000000000000000, -0.000000000000000000, 1.000000000000000000 ) ) ;
#64291 = VECTOR ( 'NONE', #25535, 1000.000000000000114 ) ;
#64290 = CARTESIAN_POINT ( 'NONE',  ( 197.0544939925610777, 42.37846845930137363, 12.19834728626771891 ) ) ;
#64292 = FACE_OUTER_BOUND ( 'NONE', #63700, .T. ) ;
#64293 = CARTESIAN_POINT ( 'NONE',  ( 29.24772827788807561, -282.2184733024449201, -239.5788855332017704 ) ) ;
#64294 = CARTESIAN_POINT ( 'NONE',  ( -25.57490725043009050, -281.9602612998589848, -195.2910400742656805 ) ) ;
#64295 = CARTESIAN_POINT ( 'NONE',  ( -103.2295756950217367, -283.1780771136274666, -302.4494280215002391 ) ) ;
#64296 = CARTESIAN_POINT ( 'NONE',  ( -24.68876554313450811, -282.0757311310477462, -197.2121690888495777 ) ) ;
#64297 = CARTESIAN_POINT ( 'NONE',  ( 36.28074556067961964, -273.9765777567299665, -266.1181661493768047 ) ) ;
#64298 = CARTESIAN_POINT ( 'NONE',  ( 82.64890176555634582, -299.5541904835127980, -197.7582414438974183 ) ) ;
#64299 = CARTESIAN_POINT ( 'NONE',  ( -43.18343439339132317, -253.0206516614774159, -472.6442049081569508 ) ) ;
#64300 = VECTOR ( 'NONE', #81592, 1000.000000000000000 ) ;
#64301 = CARTESIAN_POINT ( 'NONE',  ( -62.34376567437308836, -278.1719733601764801, -343.0744146994452990 ) ) ;
#64302 = ORIENTED_EDGE ( 'NONE', *, *, #27474, .F. ) ;
#64303 = ORIENTED_EDGE ( 'NONE', *, *, #17274, .T. ) ;
#64304 = CARTESIAN_POINT ( 'NONE',  ( 175.2296996224750103, 130.0000000000000568, 0.000000000000000000 ) ) ;
#64305 = CARTESIAN_POINT ( 'NONE',  ( -110.6137667434262681, -286.3064784948170427, -288.0114343624215394 ) ) ;
#64306 = ADVANCED_FACE ( 'NONE', ( #31299 ), #81462, .F. ) ;
#64307 = CARTESIAN_POINT ( 'NONE',  ( 35.69658172111954286, -292.6828998638386565, -265.3153683164657650 ) ) ;
#64308 = CARTESIAN_POINT ( 'NONE',  ( 21.40577683879840620, -287.5701198435004358, -319.9801338632363468 ) ) ;
#64309 = CARTESIAN_POINT ( 'NONE',  ( -37.25752343330825056, -284.2930418577966520, -196.3352183213253284 ) ) ;
#64311 = CARTESIAN_POINT ( 'NONE',  ( -23.61897982175615951, -287.1143691806655625, -343.1435868860552887 ) ) ;
#64310 = CARTESIAN_POINT ( 'NONE',  ( -110.8153276975776009, -283.1916945597094468, -265.4076021161958465 ) ) ;
#64312 = CARTESIAN_POINT ( 'NONE',  ( -4.636520057316280585, -283.8164013608051732, -336.0688169426838954 ) ) ;
#64313 = CARTESIAN_POINT ( 'NONE',  ( -19.01341392722402546, -272.2877638636493316, -197.5814888809499905 ) ) ;
#64314 = CARTESIAN_POINT ( 'NONE',  ( -73.21815181915705750, -283.9848573080953997, -203.0767914262243039 ) ) ;
#64315 = CARTESIAN_POINT ( 'NONE',  ( -67.40060577870521286, -297.4465505687067548, -339.0740195548497127 ) ) ;
#64316 = CARTESIAN_POINT ( 'NONE',  ( -105.0171709743313926, -282.9819557775090288, -237.6493606287095588 ) ) ;
#64317 = CARTESIAN_POINT ( 'NONE',  ( -96.60313430386329969, -280.0936449559250150, -227.3321641490323657 ) ) ;
#64318 = CARTESIAN_POINT ( 'NONE',  ( 35.92673468165072848, -289.3365992374277198, -253.5182266915477669 ) ) ;
#64319 = LINE ( 'NONE', #13624, #36852 ) ;
#64320 = FACE_OUTER_BOUND ( 'NONE', #6150, .T. ) ;
#64321 = CARTESIAN_POINT ( 'NONE',  ( 36.35134775167517063, -295.2588896797203120, -253.6104121694705498 ) ) ;
#64322 = CARTESIAN_POINT ( 'NONE',  ( -51.68772512496835247, -275.2355271519058988, -343.9762809082972126 ) ) ;
#64323 = CARTESIAN_POINT ( 'NONE',  ( -74.59164692859015133, -290.7666187596316263, -203.1554613454208038 ) ) ;
#64324 = CARTESIAN_POINT ( 'NONE',  ( -72.52370616124974845, -293.9258837640778097, -335.2497840450249100 ) ) ;
#64325 = CARTESIAN_POINT ( 'NONE',  ( -103.8087499645918399, -277.6592795817295496, -238.8827533835867030 ) ) ;
#64326 = CARTESIAN_POINT ( 'NONE',  ( -35.07725289688835346, -296.2203756193097206, -196.1266373355561541 ) ) ;
#64327 = CARTESIAN_POINT ( 'NONE',  ( -38.92488140263169782, -293.3470546993085009, -196.8850197163308167 ) ) ;
#64328 = CARTESIAN_POINT ( 'NONE',  ( -20.19161114001083490, -279.3376638359844719, -345.3538533559490702 ) ) ;
#64329 = CARTESIAN_POINT ( 'NONE',  ( -3.553361353515080090, -293.0942587454981094, -338.7938315540193912 ) ) ;
#64330 = CARTESIAN_POINT ( 'NONE',  ( -42.70189713450172064, -290.7208926183793665, -344.0173623997341110 ) ) ;
#64331 = CARTESIAN_POINT ( 'NONE',  ( -2.500232579277053002, -290.7463978564754825, -202.8184191527291489 ) ) ;
#64332 = CIRCLE ( 'NONE', #15897, 0.4999999999999989453 ) ;
#64333 = CARTESIAN_POINT ( 'NONE',  ( -80.74048096559134535, -291.0788983514864867, -329.8544814643549898 ) ) ;
#64334 = LINE ( 'NONE', #63385, #84952 ) ;
#64335 = CARTESIAN_POINT ( 'NONE',  ( -107.8787547516812708, -291.0967423015341069, -289.9674358561701411 ) ) ;
#64336 = ADVANCED_FACE ( 'NONE', ( #2871 ), #23719, .T. ) ;
#64337 = CARTESIAN_POINT ( 'NONE',  ( 196.8803347170859865, 20.19615242270661426, 12.49999999999999289 ) ) ;
#64338 = CARTESIAN_POINT ( 'NONE',  ( -112.2549087152298597, -291.9591115730350452, -254.2985499766523105 ) ) ;
#64340 = CARTESIAN_POINT ( 'NONE',  ( -77.25515655472437970, -291.5003627885799915, -209.2389779997480161 ) ) ;
#64339 = CARTESIAN_POINT ( 'NONE',  ( 35.74233106217786116, -279.3375189914528960, -251.9999853570184030 ) ) ;
#64341 = CARTESIAN_POINT ( 'NONE',  ( -22.56617992221908509, -280.2361386073488347, -194.7377947474200255 ) ) ;
#64342 = CARTESIAN_POINT ( 'NONE',  ( -16.15173329207562603, -282.4523106554419201, -344.4213171312875374 ) ) ;
#64343 = AXIS2_PLACEMENT_3D ( 'NONE', #52106, #36506, #59706 ) ;
#64344 = CARTESIAN_POINT ( 'NONE',  ( 21.08896203919870516, -284.9047667092990537, -223.3209963924220460 ) ) ;
#64345 = DIRECTION ( 'NONE',  ( 1.000000000000000000, -0.000000000000000000, -0.000000000000000000 ) ) ;
#64346 = CARTESIAN_POINT ( 'NONE',  ( 8.539088898974560138, -280.5560889380074059, -328.7861448993861586 ) ) ;
#64347 = CARTESIAN_POINT ( 'NONE',  ( -24.11297164892630818, -284.2207929268104749, -196.4841816055509298 ) ) ;
#64348 = CARTESIAN_POINT ( 'NONE',  ( 8.148869718730979983, -279.1411590877679032, -209.0311129058181621 ) ) ;
#64349 = AXIS2_PLACEMENT_3D ( 'NONE', #63436, #20327, #13691 ) ;
#64350 = CARTESIAN_POINT ( 'NONE',  ( 26.10937971688296955, -285.9020215805663838, -227.2626837416132446 ) ) ;
#64351 = CARTESIAN_POINT ( 'NONE',  ( 34.32479902042874187, -276.5486664835795523, -285.0755539980270328 ) ) ;
#64352 = CARTESIAN_POINT ( 'NONE',  ( 150.8012326218627948, 131.0000000000000568, -11.50000000000000000 ) ) ;
#64353 = CARTESIAN_POINT ( 'NONE',  ( -49.84408609892941655, -293.4902922642074827, -197.5759430103919101 ) ) ;
#64354 = CARTESIAN_POINT ( 'NONE',  ( -18.71134374824497115, -275.7126454326285625, -196.2017478159464190 ) ) ;
#64355 = CARTESIAN_POINT ( 'NONE',  ( -92.74545013234352098, -277.5418670399407688, -317.9269878085795540 ) ) ;
#64356 = CARTESIAN_POINT ( 'NONE',  ( -90.78746412824945367, -291.4861909013414447, -214.8565257819194585 ) ) ;
#64357 = CARTESIAN_POINT ( 'NONE',  ( 37.84263308624665711, -279.7343271825826037, -278.3902767621600560 ) ) ;
#64358 = CARTESIAN_POINT ( 'NONE',  ( -39.20956439237792779, -291.8626716879232958, -193.3707413523379159 ) ) ;
#64359 = ADVANCED_FACE ( 'NONE', ( #81926 ), #45005, .F. ) ;
#64360 = CARTESIAN_POINT ( 'NONE',  ( -107.6177114222323326, -289.8831974916220702, -249.7085902318378317 ) ) ;
#64361 = CARTESIAN_POINT ( 'NONE',  ( -30.79166626403450380, -292.9691785523134513, -345.0745552280749280 ) ) ;
#64362 = ORIENTED_EDGE ( 'NONE', *, *, #76024, .F. ) ;
#64363 = CARTESIAN_POINT ( 'NONE',  ( -22.72219127671001360, -291.7519975002983301, -198.7771923958328273 ) ) ;
#64364 = CARTESIAN_POINT ( 'NONE',  ( -26.41588298435790350, -486.4924983417995463, -465.6442049081569508 ) ) ;
#64365 = CARTESIAN_POINT ( 'NONE',  ( 27.33386217378598815, -273.4809262143061233, -301.5434626090942629 ) ) ;
#64366 = CARTESIAN_POINT ( 'NONE',  ( -95.38529460948660699, -296.2923134969316266, -220.0447483214486226 ) ) ;
#64367 = CARTESIAN_POINT ( 'NONE',  ( -113.1085767075949491, -285.7290089238606470, -281.3497512366016053 ) ) ;
#64368 = CARTESIAN_POINT ( 'NONE',  ( 35.62989344132367364, -287.4303335985832177, -273.7619457919724937 ) ) ;
#64369 = CARTESIAN_POINT ( 'NONE',  ( -18.82420813340162979, -278.3294950543986488, -341.6900058248146479 ) ) ;
#64370 = CARTESIAN_POINT ( 'NONE',  ( 25.80554818424433705, -292.1111315348035191, -310.2610728881064119 ) ) ;
#64371 = CARTESIAN_POINT ( 'NONE',  ( -85.11532307148122811, -297.4820003728777920, -326.9585154676223056 ) ) ;
#64372 = CARTESIAN_POINT ( 'NONE',  ( -1.288497971199028980, -275.3578437271847861, -334.3505975099982379 ) ) ;
#64373 = EDGE_LOOP ( 'NONE', ( #6791, #2962, #53275, #58767 ) ) ;
#64374 = CARTESIAN_POINT ( 'NONE',  ( 113.5000000000000568, -296.0521521680024080, -400.5374811273811702 ) ) ;
#64375 = CARTESIAN_POINT ( 'NONE',  ( -72.06829632172608058, -295.1655267636355688, -339.0619753893969346 ) ) ;
#64376 = CARTESIAN_POINT ( 'NONE',  ( -2.674383704818851459, -290.5105819744737232, -336.2930346170012967 ) ) ;
#64377 = CARTESIAN_POINT ( 'NONE',  ( 202.8433248031682865, 295.9636489450775230, -54.00000000006134115 ) ) ;
#64378 = EDGE_CURVE ( 'NONE', #43923, #50859, #89717, .T. ) ;
#64379 = CARTESIAN_POINT ( 'NONE',  ( -45.36540959979937071, -289.8079119360440359, -343.0213736551908141 ) ) ;
#64380 = EDGE_LOOP ( 'NONE', ( #47507, #90954, #89437, #34208, #41988, #82153 ) ) ;
#64381 = CARTESIAN_POINT ( 'NONE',  ( -36.74231642350465421, -279.1182660441641019, -193.5857453234507659 ) ) ;
#64382 = CARTESIAN_POINT ( 'NONE',  ( 6.562617068261710429, -295.1242884894569443, -333.5585932379202063 ) ) ;
#64383 = CARTESIAN_POINT ( 'NONE',  ( -82.14164690048340844, -287.7955781288341655, -331.4616110015456911 ) ) ;
#64384 = CARTESIAN_POINT ( 'NONE',  ( -113.1190505072844701, -297.0549098104040695, -256.8135181553838606 ) ) ;
#64385 = CARTESIAN_POINT ( 'NONE',  ( 35.44584944960058692, -293.9624009852225299, -276.1972222645192687 ) ) ;
#64386 = CARTESIAN_POINT ( 'NONE',  ( 197.7363269526848057, 68.71792440747597652, -9.406972186202848363 ) ) ;
#64387 = CARTESIAN_POINT ( 'NONE',  ( 138.6539576904058606, 132.0000000000000568, 10.50000000000000000 ) ) ;
#64388 = CARTESIAN_POINT ( 'NONE',  ( -43.11039638419920550, -290.6438594746966260, -346.4494212641529316 ) ) ;
#64389 = CARTESIAN_POINT ( 'NONE',  ( -99.90806341382575795, -293.4094976428775681, -320.2154176792147382 ) ) ;
#64390 = CARTESIAN_POINT ( 'NONE',  ( -95.82288174436936856, -278.5753332783679070, -220.4082995835377687 ) ) ;
#64391 = CARTESIAN_POINT ( 'NONE',  ( -15.57552213279881670, -284.7699773003335508, -341.9590363857040529 ) ) ;
#64392 = CARTESIAN_POINT ( 'NONE',  ( 19.85782846150384273, -285.4346281535941898, -219.6191930782352131 ) ) ;
#64393 = CARTESIAN_POINT ( 'NONE',  ( 36.55072908179593583, -285.7485823849149824, -279.3735040521349333 ) ) ;
#64394 = CARTESIAN_POINT ( 'NONE',  ( 31.90066331500138119, -277.8114637379513852, -301.1149890022907698 ) ) ;
#64395 = ORIENTED_EDGE ( 'NONE', *, *, #38609, .F. ) ;
#64397 = CARTESIAN_POINT ( 'NONE',  ( -95.68810345742923573, -278.5187732037104524, -226.2995676792914139 ) ) ;
#64396 = CARTESIAN_POINT ( 'NONE',  ( -110.2801391741247983, -278.5126121371581007, -273.3584684002801168 ) ) ;
#64398 = CARTESIAN_POINT ( 'NONE',  ( -5.256162063466479850, -275.5442637721104688, -200.7047416907461184 ) ) ;
#64399 = CARTESIAN_POINT ( 'NONE',  ( -112.3256842372725117, -277.5448076277122027, -254.6323289033134358 ) ) ;
#64400 = CARTESIAN_POINT ( 'NONE',  ( 4.168043760347364568, -58.11863228567613504, -352.1996900385278195 ) ) ;
#64401 = CARTESIAN_POINT ( 'NONE',  ( -93.00981761228777600, -274.2181319795718082, -217.4847574824377432 ) ) ;
#64402 = CARTESIAN_POINT ( 'NONE',  ( -87.09248407922208912, -298.8006180069590982, -212.2959583402710848 ) ) ;
#64403 = CARTESIAN_POINT ( 'NONE',  ( -106.6662871844225293, -281.4805209788417528, -237.0123917617630980 ) ) ;
#64404 = ORIENTED_EDGE ( 'NONE', *, *, #79357, .T. ) ;
#64405 = CARTESIAN_POINT ( 'NONE',  ( 82.64742324267871254, -299.6703133987807632, -192.8578546138987519 ) ) ;
#64406 = CARTESIAN_POINT ( 'NONE',  ( -57.49249684837443652, -286.8656650487132538, -199.8230215280137543 ) ) ;
#64407 = CARTESIAN_POINT ( 'NONE',  ( -87.10348453532112956, -287.1306894329230772, -212.8654993279931205 ) ) ;
#64408 = CARTESIAN_POINT ( 'NONE',  ( -5.755888562898014982, -287.9740461472354127, -336.2870550358711625 ) ) ;
#64409 = CARTESIAN_POINT ( 'NONE',  ( -106.9526328098753538, -283.6397291934030704, -303.1306915871295473 ) ) ;
#64410 = CARTESIAN_POINT ( 'NONE',  ( -62.56341090780811953, -278.1184138706750559, -200.9508150458516980 ) ) ;
#64411 = CARTESIAN_POINT ( 'NONE',  ( -70.55599010159551199, -287.4699311427598900, -203.9566022471602196 ) ) ;
#64412 = CARTESIAN_POINT ( 'NONE',  ( 17.59245306459891012, -279.3359059350454459, -221.2393655068098610 ) ) ;
#64413 = CARTESIAN_POINT ( 'NONE',  ( -51.35864970847332245, -278.5503280460064843, -342.5052002146613290 ) ) ;
#64414 = CARTESIAN_POINT ( 'NONE',  ( 34.90156370213900772, -275.8996708140516603, -259.3728939575050845 ) ) ;
#64415 = CARTESIAN_POINT ( 'NONE',  ( -4.517197329014404517, -287.4241552041630712, -339.5893979007939265 ) ) ;
#64416 = COLOUR_RGB ( '',0.7921568627450980005, 0.8196078431372548767, 0.9333333333333333481 ) ;
#64417 = CARTESIAN_POINT ( 'NONE',  ( -58.43258919843992771, -284.1207569454701343, -344.3037986221444839 ) ) ;
#64418 = CARTESIAN_POINT ( 'NONE',  ( -114.2931396907330139, -285.0133028107742916, -272.8535005684336738 ) ) ;
#64419 = CARTESIAN_POINT ( 'NONE',  ( 4.921427777927685376, -280.8080200882454278, -210.8394578571337945 ) ) ;
#64420 = ORIENTED_EDGE ( 'NONE', *, *, #36695, .T. ) ;
#64421 = ORIENTED_EDGE ( 'NONE', *, *, #1899, .T. ) ;
#64422 = DIRECTION ( 'NONE',  ( 0.000000000000000000, 0.000000000000000000, -1.000000000000000000 ) ) ;
#64423 = CARTESIAN_POINT ( 'NONE',  ( 24.85155857719669825, -289.9946971379707179, -313.7213640003960791 ) ) ;
#64424 = CARTESIAN_POINT ( 'NONE',  ( -113.6946172941926108, -289.2980369915989627, -265.5103127030022279 ) ) ;
#64425 = CARTESIAN_POINT ( 'NONE',  ( -34.46170431063792705, -297.2862779787807881, -197.2000453612116928 ) ) ;
#64426 = CARTESIAN_POINT ( 'NONE',  ( 38.75226698425536398, -292.7573656211983462, -258.9120952859369140 ) ) ;
#64427 = CARTESIAN_POINT ( 'NONE',  ( -72.70845329467637441, -288.0094597772149996, -335.0132681701780939 ) ) ;
#64428 = CARTESIAN_POINT ( 'NONE',  ( 33.30749109056069557, -292.0803484970601858, -292.4216210125902080 ) ) ;
#64429 = CARTESIAN_POINT ( 'NONE',  ( 32.64762668622217490, -288.4652903822090479, -248.2142144258249914 ) ) ;
#64430 = CARTESIAN_POINT ( 'NONE',  ( -85.33152481854864391, -287.9090924074130839, -210.2361428286349110 ) ) ;
#64431 = CARTESIAN_POINT ( 'NONE',  ( -23.65134415127682388, -290.8774919745281409, -344.1537428290707226 ) ) ;
#64432 = CARTESIAN_POINT ( 'NONE',  ( -70.07574955262866467, -289.6217537651576777, -202.6964267482321134 ) ) ;
#64433 = CARTESIAN_POINT ( 'NONE',  ( -0.2695735499708724059, -294.5449217423559389, -205.1060487566341521 ) ) ;
#64434 = CARTESIAN_POINT ( 'NONE',  ( -110.3292873604746944, -285.4142724016641068, -276.3794697227623374 ) ) ;
#64435 = CARTESIAN_POINT ( 'NONE',  ( 22.49984862790955731, -294.9310972230312586, -224.8534924383180282 ) ) ;
#64436 = FACE_OUTER_BOUND ( 'NONE', #16581, .T. ) ;
#64437 = CARTESIAN_POINT ( 'NONE',  ( 222.4306832106270804, -135.2391364535880882, -21.50000000000000000 ) ) ;
#64438 = CARTESIAN_POINT ( 'NONE',  ( -20.92538960612227683, -300.1762811758464977, -194.7957882766897626 ) ) ;
#64439 = CARTESIAN_POINT ( 'NONE',  ( 7.885778248651064359, -281.6135021240404512, -327.9330022750591525 ) ) ;
#64440 = CARTESIAN_POINT ( 'NONE',  ( -96.71493259058206604, -281.9238446246076251, -316.2058826776774936 ) ) ;
#64441 = CARTESIAN_POINT ( 'NONE',  ( -96.39389576316085595, -295.0864808814266667, -319.5445441175951942 ) ) ;
#64442 = CARTESIAN_POINT ( 'NONE',  ( 10.15226699601402771, -272.9569511001067781, -213.5287057410741340 ) ) ;
#64443 = CARTESIAN_POINT ( 'NONE',  ( -79.46664140816740485, -275.7053703248596435, -331.7981890460020509 ) ) ;
#64444 = CARTESIAN_POINT ( 'NONE',  ( -109.3646791436865584, -297.6748559057865009, -285.0502031847843796 ) ) ;
#64445 = CARTESIAN_POINT ( 'NONE',  ( -68.58639436204767037, -272.2242934687376987, -200.6160999988700269 ) ) ;
#64446 = CARTESIAN_POINT ( 'NONE',  ( -58.56093415721047535, -296.7572467868780564, -340.8247186789637908 ) ) ;
#64447 = DIRECTION ( 'NONE',  ( 1.000000000000000000, 0.000000000000000000, 0.000000000000000000 ) ) ;
#64448 = CARTESIAN_POINT ( 'NONE',  ( -88.24542140941591128, -298.1201237186459707, -217.7412304273850054 ) ) ;
#64449 = DIRECTION ( 'NONE',  ( -1.000000000000000000, 2.640448681563344014E-15, 0.000000000000000000 ) ) ;
#64451 = CARTESIAN_POINT ( 'NONE',  ( -90.19514101269322737, -273.1118063077031479, -219.9889447561661768 ) ) ;
#64450 = CARTESIAN_POINT ( 'NONE',  ( 35.78687109716308612, -285.3398179259469885, -252.1781898070272803 ) ) ;
#64452 = CARTESIAN_POINT ( 'NONE',  ( 32.71202783455942864, -287.1421413503600775, -238.2722378208749774 ) ) ;
#64453 = CARTESIAN_POINT ( 'NONE',  ( 39.33401220729152925, -287.1263292437990913, -262.9635165093593514 ) ) ;
#64454 = CARTESIAN_POINT ( 'NONE',  ( 7.938366319146354044, -296.4167145600439426, -330.5950152696555051 ) ) ;
#64455 = CARTESIAN_POINT ( 'NONE',  ( 20.78555917980293088, -290.9013635912927498, -223.2107013699527727 ) ) ;
#64456 = CARTESIAN_POINT ( 'NONE',  ( -38.15791405499206235, -279.2393389542459659, -193.5269288731509505 ) ) ;
#64457 = CARTESIAN_POINT ( 'NONE',  ( 21.31550574532286291, -284.4094976428775681, -223.6242672951989618 ) ) ;
#64458 = DIRECTION ( 'NONE',  ( 0.000000000000000000, 0.000000000000000000, -1.000000000000000000 ) ) ;
#64459 = CARTESIAN_POINT ( 'NONE',  ( -14.42755086092044614, -285.1507276763289269, -200.5792453577557239 ) ) ;
#64460 = CARTESIAN_POINT ( 'NONE',  ( 197.0997303688997704, 71.85475162903931334, -12.14496016938517009 ) ) ;
#64461 = CARTESIAN_POINT ( 'NONE',  ( -12.65289333048296250, -286.7309927975702522, -341.1810549110675197 ) ) ;
#64462 = CARTESIAN_POINT ( 'NONE',  ( -70.84878265057240299, -299.2026690299682059, -204.5920842196651961 ) ) ;
#64463 = CARTESIAN_POINT ( 'NONE',  ( -70.99158755597717629, -281.0420581609740793, -201.7587027806579840 ) ) ;
#64465 = CARTESIAN_POINT ( 'NONE',  ( -2.428663479340355202, -282.5766268895550297, -334.4853119061081088 ) ) ;
#64464 = CARTESIAN_POINT ( 'NONE',  ( -110.0126428132140859, -294.3171242747013707, -290.2945294859731007 ) ) ;
#64466 = CARTESIAN_POINT ( 'NONE',  ( -110.7991569379851455, -296.4282270007389570, -293.4920834983084319 ) ) ;
#64467 = CARTESIAN_POINT ( 'NONE',  ( -92.37544196934980789, -298.7664715934879496, -221.3509658476129971 ) ) ;
#64468 = CARTESIAN_POINT ( 'NONE',  ( 35.98541858618412448, -285.3995463850646956, -252.1279651401911508 ) ) ;
#64469 = CARTESIAN_POINT ( 'NONE',  ( -25.73099632562329120, -282.2002419152404968, -196.2652867665148619 ) ) ;
#64470 = CARTESIAN_POINT ( 'NONE',  ( -109.5970128993856036, -295.4538860901553790, -282.3017303933320363 ) ) ;
#64471 = ORIENTED_EDGE ( 'NONE', *, *, #10664, .T. ) ;
#64472 = CARTESIAN_POINT ( 'NONE',  ( 202.9738562182569694, 296.4636489450776367, -53.99999999999997868 ) ) ;
#64473 = CARTESIAN_POINT ( 'NONE',  ( -38.89457391577523282, -285.0515845840061502, -345.0025405317936702 ) ) ;
#64474 = DIRECTION ( 'NONE',  ( -1.000000000000000000, 0.000000000000000000, 0.000000000000000000 ) ) ;
#64475 = CARTESIAN_POINT ( 'NONE',  ( 35.78497577281001440, -284.8380690714490129, -253.7030783399848985 ) ) ;
#64476 = CARTESIAN_POINT ( 'NONE',  ( -20.17215399371378481, -276.0342699359373455, -345.3114177842048207 ) ) ;
#64477 = CARTESIAN_POINT ( 'NONE',  ( 18.47795866041701984, -292.7171004276331132, -223.3168229271128098 ) ) ;
#64478 = CARTESIAN_POINT ( 'NONE',  ( 33.77765719712441239, -282.8190653423158096, -251.0062878782554208 ) ) ;
#64479 =( GEOMETRIC_REPRESENTATION_CONTEXT ( 3 ) GLOBAL_UNCERTAINTY_ASSIGNED_CONTEXT ( ( #11310 ) ) GLOBAL_UNIT_ASSIGNED_CONTEXT ( ( #27421, #44863, #87941 ) ) REPRESENTATION_CONTEXT ( 'NONE', 'WORKASPACE' ) );
#64480 = CARTESIAN_POINT ( 'NONE',  ( 31.02676457209103233, -277.5220762985101146, -298.2855571519621094 ) ) ;
#64481 = CARTESIAN_POINT ( 'NONE',  ( 17.26732991740023948, -283.8891956746959409, -323.5806242021854473 ) ) ;
#64482 = CARTESIAN_POINT ( 'NONE',  ( 32.60507000949143475, -280.6423018395626627, -292.7656843468159877 ) ) ;
#64483 = CARTESIAN_POINT ( 'NONE',  ( -107.3911718099231365, -280.9023202273864968, -243.4186577055732243 ) ) ;
#64484 = CARTESIAN_POINT ( 'NONE',  ( -111.0377458638795218, -273.0009844524573737, -247.8653269367185885 ) ) ;
#64485 = CARTESIAN_POINT ( 'NONE',  ( -6.576650455173027154, -276.4925527313734506, -340.9622829217270805 ) ) ;
#64486 = CARTESIAN_POINT ( 'NONE',  ( 19.56186268391509486, -294.8035970298693655, -222.3684233302651876 ) ) ;
#64487 = FACE_OUTER_BOUND ( 'NONE', #69832, .T. ) ;
#64488 = EDGE_CURVE ( 'NONE', #44128, #14370, #73057, .T. ) ;
#64489 = CARTESIAN_POINT ( 'NONE',  ( 175.2296996224750103, 214.5000000000000568, 0.000000000000000000 ) ) ;
#64490 = CARTESIAN_POINT ( 'NONE',  ( 23.87406316895902947, -292.2941942965364888, -315.0252725030736656 ) ) ;
#64491 = CARTESIAN_POINT ( 'NONE',  ( -78.88491528544589926, -272.9832558776610654, -210.1985046608133416 ) ) ;
#64492 = CARTESIAN_POINT ( 'NONE',  ( 27.52682286650468413, -295.6036830218861837, -310.6447832343832829 ) ) ;
#64493 = CARTESIAN_POINT ( 'NONE',  ( 13.14571598031880839, -295.5702579669950865, -328.0424802249561935 ) ) ;
#64494 = CARTESIAN_POINT ( 'NONE',  ( -83.66159047939355276, -291.6896254579139622, -329.1360801790992809 ) ) ;
#64495 = CARTESIAN_POINT ( 'NONE',  ( -110.2787489673270755, -276.3358494421663636, -287.1576229926963038 ) ) ;
#64496 = CARTESIAN_POINT ( 'NONE',  ( -26.79376929207654712, -278.8371176923062649, -344.0500272637839316 ) ) ;
#64497 = CARTESIAN_POINT ( 'NONE',  ( -0.05748086624716639004, -292.6321896449697419, -334.8497560416354304 ) ) ;
#64498 = CARTESIAN_POINT ( 'NONE',  ( 21.89451022196698915, -282.7695589643986978, -223.1030490473544319 ) ) ;
#64499 = CARTESIAN_POINT ( 'NONE',  ( -108.6630568638028365, -283.6958636808075198, -253.3515641638277600 ) ) ;
#64500 = CARTESIAN_POINT ( 'NONE',  ( 169.7216216461204112, 230.9133231598102043, -192.0398292467810677 ) ) ;
#64501 = VERTEX_POINT ( 'NONE', #59246 ) ;
#64502 = CARTESIAN_POINT ( 'NONE',  ( 1.108834432361260003, -282.1904798437578847, -332.4978837284465953 ) ) ;
#64503 = CARTESIAN_POINT ( 'NONE',  ( 8.351297179918017122, -281.7405340506363700, -208.7025609395122672 ) ) ;
#64504 = CARTESIAN_POINT ( 'NONE',  ( -102.1742072254386500, -283.8841529935455128, -229.5597118603892284 ) ) ;
#64505 = CARTESIAN_POINT ( 'NONE',  ( -64.66980700518718095, -280.6452912524573549, -198.5694668202752382 ) ) ;
#64506 = SHAPE_REPRESENTATION_RELATIONSHIP ( 'NONE' , 'NONE' ,  #30030, #2316 ) ;
#64507 = CARTESIAN_POINT ( 'NONE',  ( -112.1103476709528053, -279.8790841208067377, -285.6688771612105597 ) ) ;
#64508 = CARTESIAN_POINT ( 'NONE',  ( 27.36219212280431989, -296.4805209788416391, -301.4846348637938149 ) ) ;
#64509 = VERTEX_POINT ( 'NONE', #9489 ) ;
#64510 = ORIENTED_EDGE ( 'NONE', *, *, #69553, .T. ) ;
#64511 = CARTESIAN_POINT ( 'NONE',  ( -85.37473520293464446, -299.3889410144918770, -212.6926992077347620 ) ) ;
#64512 = CARTESIAN_POINT ( 'NONE',  ( -102.2294517245494205, -277.0664893436626244, -233.4636046099098792 ) ) ;
#64513 = CARTESIAN_POINT ( 'NONE',  ( -112.3560681319127781, -292.1587307900924202, -282.4779908182102304 ) ) ;
#64514 = CARTESIAN_POINT ( 'NONE',  ( 30.67736333966619000, -293.2600484201256563, -297.2820263624678319 ) ) ;
#64515 = CARTESIAN_POINT ( 'NONE',  ( -40.34264086357487855, -288.5965531143997964, -347.2541037017051053 ) ) ;
#64516 = CARTESIAN_POINT ( 'NONE',  ( 175.2296996224750103, 154.6894116713782807, 0.000000000000000000 ) ) ;
#64518 = CARTESIAN_POINT ( 'NONE',  ( -41.34618498889668103, -284.4007977450286830, -196.6572040888442530 ) ) ;
#64517 = CARTESIAN_POINT ( 'NONE',  ( 23.54835874479473645, -292.7466679036244273, -316.5239496233062937 ) ) ;
#64519 = CARTESIAN_POINT ( 'NONE',  ( -6.783065363192309682, -294.3180397001498818, -202.7073278129387859 ) ) ;
#64520 = CARTESIAN_POINT ( 'NONE',  ( -4.266184045978813622, -284.9762626408649453, -204.5073558250194310 ) ) ;
#64521 = CARTESIAN_POINT ( 'NONE',  ( -65.48918402116464677, -284.7432030361666762, -338.2641479230591131 ) ) ;
#64522 = ORIENTED_EDGE ( 'NONE', *, *, #50647, .F. ) ;
#64523 = CARTESIAN_POINT ( 'NONE',  ( -74.57529698846450117, -292.5104216721237549, -203.2308008520193710 ) ) ;
#64524 = CARTESIAN_POINT ( 'NONE',  ( 23.73052652282639130, -281.4878865413351150, -230.1678779353851780 ) ) ;
#64525 = CARTESIAN_POINT ( 'NONE',  ( 30.54333382965190680, -292.8073581242786645, -305.8523969403868250 ) ) ;
#64526 = CARTESIAN_POINT ( 'NONE',  ( 36.99080631240903472, -288.5991287849770401, -289.8248613851279742 ) ) ;
#64527 = CARTESIAN_POINT ( 'NONE',  ( -31.82492592540377174, -289.4767734014784537, -347.1540520971149135 ) ) ;
#64528 = CARTESIAN_POINT ( 'NONE',  ( -42.67624737291180992, -286.1496899679098647, -197.5436669105693284 ) ) ;
#64529 = VERTEX_POINT ( 'NONE', #73457 ) ;
#64530 = CARTESIAN_POINT ( 'NONE',  ( 196.5570723171844350, 25.86847754248514875, 12.83135264428034539 ) ) ;
#64531 = CARTESIAN_POINT ( 'NONE',  ( 36.86565793160876581, -295.6068153806737087, -285.6442293638363026 ) ) ;
#64532 = CARTESIAN_POINT ( 'NONE',  ( -48.87897920895333925, -296.5931000476635973, -194.6758622879561358 ) ) ;
#64533 = CARTESIAN_POINT ( 'NONE',  ( -99.38077421114850551, -277.0740926879548169, -309.3732386908070566 ) ) ;
#64534 = CARTESIAN_POINT ( 'NONE',  ( -97.76084207921024927, -272.6974328686652598, -222.7265277202310187 ) ) ;
#64535 = CARTESIAN_POINT ( 'NONE',  ( 4.191335080983512817, -292.9608134091878355, -331.2357000134188638 ) ) ;
#64536 = CARTESIAN_POINT ( 'NONE',  ( 14.45630348962820122, -278.0719816276331358, -323.2997177924704033 ) ) ;
#64537 = CARTESIAN_POINT ( 'NONE',  ( -110.8016007932268963, -270.8350927823201459, -259.3097206377961470 ) ) ;
#64538 = CARTESIAN_POINT ( 'NONE',  ( 22.11741417325055181, -294.1582104793656072, -227.3078537129923689 ) ) ;
#64539 = CARTESIAN_POINT ( 'NONE',  ( -108.5962223563213911, -297.4047404294462353, -287.6482577032830932 ) ) ;
#64540 = CARTESIAN_POINT ( 'NONE',  ( -43.28623554199135270, -273.9965794730779862, -431.8406871970819907 ) ) ;
#64541 = CARTESIAN_POINT ( 'NONE',  ( -112.1219593623819293, -294.4544703416614766, -277.9730332437077891 ) ) ;
#64542 = CARTESIAN_POINT ( 'NONE',  ( -46.12647284233057832, -298.5949075528844787, -193.9664810320958566 ) ) ;
#64543 = CARTESIAN_POINT ( 'NONE',  ( -80.76975134200333173, -288.2288125048684719, -329.8331184021636204 ) ) ;
#64544 = CARTESIAN_POINT ( 'NONE',  ( -62.73003454730126549, -275.7218535601055009, -199.7889342030195508 ) ) ;
#64545 = CARTESIAN_POINT ( 'NONE',  ( -110.5408916181046663, -291.4464507817519916, -273.9323445476123311 ) ) ;
#64546 = CARTESIAN_POINT ( 'NONE',  ( -113.0089288195105581, -273.2223907163500485, -256.1482573837037080 ) ) ;
#64547 = ADVANCED_FACE ( 'NONE', ( #74854 ), #21696, .T. ) ;
#64548 = CARTESIAN_POINT ( 'NONE',  ( -70.48093638989848841, -297.9360267548509569, -205.2789416701664322 ) ) ;
#64549 = ADVANCED_FACE ( 'NONE', ( #31755 ), #89485, .T. ) ;
#64550 = CARTESIAN_POINT ( 'NONE',  ( -98.11658978478460824, -281.1368372258975796, -225.7880170495248819 ) ) ;
#64551 = CARTESIAN_POINT ( 'NONE',  ( 34.86783829909473553, -279.9142829084472623, -244.9227385442196123 ) ) ;
#64552 = ORIENTED_EDGE ( 'NONE', *, *, #1420, .T. ) ;
#64553 = CARTESIAN_POINT ( 'NONE',  ( -61.20792641652438704, -282.7025496030915406, -343.5174562331770289 ) ) ;
#64554 = CARTESIAN_POINT ( 'NONE',  ( 37.53755880876393292, -274.6808813665025468, -252.7992580946491614 ) ) ;
#64555 = CARTESIAN_POINT ( 'NONE',  ( 23.96040918624438021, -279.3442538865699589, -225.1008505216792344 ) ) ;
#64556 = CARTESIAN_POINT ( 'NONE',  ( -71.64682659988218916, -277.5998769855983710, -203.4649310619071514 ) ) ;
#64557 = CARTESIAN_POINT ( 'NONE',  ( -110.1631684491267436, -271.2701662084614895, -259.4111670446782796 ) ) ;
#64558 = CARTESIAN_POINT ( 'NONE',  ( 17.80331377923768343, -276.8412068593202662, -219.4533681940166048 ) ) ;
#64559 = DIRECTION ( 'NONE',  ( 0.000000000000000000, 0.000000000000000000, 1.000000000000000000 ) ) ;
#64560 = CARTESIAN_POINT ( 'NONE',  ( 12.21613416397512530, -290.7579585129442989, -213.5946854690895691 ) ) ;
#64561 = CARTESIAN_POINT ( 'NONE',  ( -103.2158433414865613, -291.0736748591506284, -230.3885635273047967 ) ) ;
#64562 = CARTESIAN_POINT ( 'NONE',  ( 22.91365519654061345, -278.1646343270953707, -315.2979690534764359 ) ) ;
#64563 = CARTESIAN_POINT ( 'NONE',  ( -52.99431040300671469, -295.8510235791123932, -197.1299019693546200 ) ) ;
#64564 = DIRECTION ( 'NONE',  ( -0.000000000000000000, 1.000000000000000000, -0.000000000000000000 ) ) ;
#64565 = DIRECTION ( 'NONE',  ( -1.000000000000000000, 0.000000000000000000, 0.000000000000000000 ) ) ;
#64566 = CARTESIAN_POINT ( 'NONE',  ( -101.0349512674058019, -283.0849446321930714, -230.6647968602192407 ) ) ;
#64567 = CARTESIAN_POINT ( 'NONE',  ( 159.4851178187871312, 17.43233815881133708, -9.000000000000000000 ) ) ;
#64568 = CARTESIAN_POINT ( 'NONE',  ( -22.64620817748919990, -291.0393836648668753, -198.4502494022380290 ) ) ;
#64569 = CARTESIAN_POINT ( 'NONE',  ( 34.26720205331995572, -285.9482259789573959, -290.1228118733554311 ) ) ;
#64570 = DIRECTION ( 'NONE',  ( 0.000000000000000000, 1.000000000000000000, 0.000000000000000000 ) ) ;
#64571 = CARTESIAN_POINT ( 'NONE',  ( 157.3811296300184210, 16.14910309754964501, -7.138650918358436570 ) ) ;
#64572 = CARTESIAN_POINT ( 'NONE',  ( -4.693292746754944567, -292.6219760205930811, -337.8962797370410271 ) ) ;
#64573 = CARTESIAN_POINT ( 'NONE',  ( -66.33094126003810231, -281.9047330050557321, -340.9608113935905180 ) ) ;
#64574 = CARTESIAN_POINT ( 'NONE',  ( -79.52868831286397722, -281.0716887577984835, -209.8078485298291014 ) ) ;
#64575 = CARTESIAN_POINT ( 'NONE',  ( -110.5511282866018803, -286.0438813836186114, -247.6349951772083955 ) ) ;
#64576 = CARTESIAN_POINT ( 'NONE',  ( -22.73866857007272557, -278.4762806424469090, -195.7373018772554474 ) ) ;
#64577 = CARTESIAN_POINT ( 'NONE',  ( 25.69604982279730976, -288.0586454351242196, -307.2746640895851442 ) ) ;
#64578 = CARTESIAN_POINT ( 'NONE',  ( -110.0716707475626208, -279.8306985265290336, -281.5738915562349689 ) ) ;
#64579 = CARTESIAN_POINT ( 'NONE',  ( -109.6501033425589213, -279.2083592788199553, -281.5009811628668217 ) ) ;
#64580 = CARTESIAN_POINT ( 'NONE',  ( -106.4284677089787152, -286.9255063519930218, -240.1402614045403254 ) ) ;
#64581 = EDGE_LOOP ( 'NONE', ( #48355, #55759, #22772, #5448 ) ) ;
#64582 = CARTESIAN_POINT ( 'NONE',  ( -36.53849372449802502, -297.8952692800526734, -193.3611399111292144 ) ) ;
#64583 = CARTESIAN_POINT ( 'NONE',  ( 27.12911087680821609, -290.0382187882592575, -308.0846482415211653 ) ) ;
#64584 = CARTESIAN_POINT ( 'NONE',  ( 197.5046084229020096, 41.86576550531665930, 12.19218485022636855 ) ) ;
#64585 = CARTESIAN_POINT ( 'NONE',  ( -88.47809603358389552, -286.1948066931273615, -334.5364918783848793 ) ) ;
#64586 = ORIENTED_EDGE ( 'NONE', *, *, #76026, .F. ) ;
#64587 = CARTESIAN_POINT ( 'NONE',  ( -5.858382873068553209, -272.4649302057649720, -202.1055016194901270 ) ) ;
#64588 = CARTESIAN_POINT ( 'NONE',  ( 36.99889954278052073, -292.1642111192376206, -287.1506240638425993 ) ) ;
#64589 = CARTESIAN_POINT ( 'NONE',  ( -50.48842863854047636, -294.7322361177944572, -342.2301097032713528 ) ) ;
#64590 = CARTESIAN_POINT ( 'NONE',  ( -35.93950333519057239, -287.5901792209469932, -196.6811234217904598 ) ) ;
#64591 = CARTESIAN_POINT ( 'NONE',  ( 9.906434995802714027, -282.4730899709544474, -213.3242661542391261 ) ) ;
#64592 = CARTESIAN_POINT ( 'NONE',  ( -5.852609018819689979, -290.0714752236990535, -339.9818292383837957 ) ) ;
#64593 = CARTESIAN_POINT ( 'NONE',  ( 39.20929316504199136, -288.8819992766459563, -271.5269508892112071 ) ) ;
#64594 = CARTESIAN_POINT ( 'NONE',  ( -56.81428319239153524, -285.3034222904404373, -342.7891453937122606 ) ) ;
#64595 = CARTESIAN_POINT ( 'NONE',  ( -87.09357517439562457, -277.8893587537450571, -329.1995019790025481 ) ) ;
#64596 = ORIENTED_EDGE ( 'NONE', *, *, #27071, .T. ) ;
#64597 = CARTESIAN_POINT ( 'NONE',  ( 36.37357847863370353, -291.8442372682825976, -287.0137689841113797 ) ) ;
#64598 = CARTESIAN_POINT ( 'NONE',  ( 38.87096376473871118, -281.5228323519633591, -281.3442808633764116 ) ) ;
#64599 = CARTESIAN_POINT ( 'NONE',  ( -92.04857262981425947, -275.1208828734801273, -220.1623814348911026 ) ) ;
#64600 = CARTESIAN_POINT ( 'NONE',  ( -110.4542110544635705, -286.8376638359844719, -287.0812184334320705 ) ) ;
#64601 = CARTESIAN_POINT ( 'NONE',  ( 33.23463610996259376, -274.1556528283517764, -298.6623260770533648 ) ) ;
#64602 = CARTESIAN_POINT ( 'NONE',  ( -37.00175247351368313, -279.5641744234774251, -197.3003701252258111 ) ) ;
#64603 = CARTESIAN_POINT ( 'NONE',  ( 32.66314985962230821, -277.1562290101872463, -301.4630422911588994 ) ) ;
#64604 = CARTESIAN_POINT ( 'NONE',  ( -106.3647712631773032, -298.3167014589556061, -244.6956008299699192 ) ) ;
#64605 = CARTESIAN_POINT ( 'NONE',  ( -94.23285773053657977, -282.9084798875504134, -321.9191117915657969 ) ) ;
#64606 = CARTESIAN_POINT ( 'NONE',  ( -84.49158020638169830, -293.1526298000211455, -213.3097129208200613 ) ) ;
#64607 = CARTESIAN_POINT ( 'NONE',  ( -113.3842125283154303, -274.2237454229970126, -264.7061221987347608 ) ) ;
#64608 = CARTESIAN_POINT ( 'NONE',  ( -52.46463686376164759, -275.1776685771734492, -195.3097228702839629 ) ) ;
#64609 = CARTESIAN_POINT ( 'NONE',  ( 21.14212687015213277, -296.1957981138944547, -317.0684954534502822 ) ) ;
#64610 = CARTESIAN_POINT ( 'NONE',  ( -90.20703009310348364, -281.8011817663539205, -323.3988218308208502 ) ) ;
#64611 = CARTESIAN_POINT ( 'NONE',  ( -113.6446014449358159, -290.3510891343242406, -259.7920564469905003 ) ) ;
#64612 = CARTESIAN_POINT ( 'NONE',  ( -0.6839831367113394789, -274.5831523463790518, -335.4431223416971761 ) ) ;
#64613 = CARTESIAN_POINT ( 'NONE',  ( -29.56505340102581059, -287.7492115842060230, -194.5589796193584107 ) ) ;
#64614 = CARTESIAN_POINT ( 'NONE',  ( -110.4320055276906913, -289.3899588975598931, -276.6427679477179709 ) ) ;
#64615 = EDGE_LOOP ( 'NONE', ( #27088, #44714, #26265, #75169 ) ) ;
#64616 = CARTESIAN_POINT ( 'NONE',  ( -97.70537402949625516, -288.4964337440296163, -317.2101645927253912 ) ) ;
#64617 = CARTESIAN_POINT ( 'NONE',  ( -85.93993655389900255, -291.0236200093633556, -215.7926150303602526 ) ) ;
#64618 = EDGE_LOOP ( 'NONE', ( #60760, #70039 ) ) ;
#64619 = CARTESIAN_POINT ( 'NONE',  ( 33.76093392611535648, -288.9997416855713368, -299.2412454452308452 ) ) ;
#64620 = CARTESIAN_POINT ( 'NONE',  ( -92.73990890969220402, -278.2083216359442872, -317.9334413505611678 ) ) ;
#64621 = CARTESIAN_POINT ( 'NONE',  ( 29.21422807408838551, -291.9754562643007034, -232.2586124192931436 ) ) ;
#64622 = CARTESIAN_POINT ( 'NONE',  ( -113.0351415636737045, -285.0301188652370570, -284.2111747879503127 ) ) ;
#64623 = CARTESIAN_POINT ( 'NONE',  ( -114.3196430519276134, -284.8901233486786282, -269.9861584539343653 ) ) ;
#64624 = CARTESIAN_POINT ( 'NONE',  ( -30.26455934443297835, -280.4772882975129846, -197.6333683028722703 ) ) ;
#64625 = CARTESIAN_POINT ( 'NONE',  ( -112.5841113068936181, -271.3072920273854152, -296.3762234298543490 ) ) ;
#64626 = CARTESIAN_POINT ( 'NONE',  ( 159.9294595360192375, 220.4978701958970078, -204.6380096544159528 ) ) ;
#64627 = CARTESIAN_POINT ( 'NONE',  ( -13.62517624662293514, -91.77141949113919850, -356.5202330857019319 ) ) ;
#64628 = CARTESIAN_POINT ( 'NONE',  ( -108.0936030651267288, -271.9969844300305226, -251.5451928909460548 ) ) ;
#64629 = CARTESIAN_POINT ( 'NONE',  ( -2.755730099628803664, -273.4411431380925706, -205.7233832493250532 ) ) ;
#64630 = CARTESIAN_POINT ( 'NONE',  ( -11.08410929350230134, -294.2266883857589619, -342.7368343112370326 ) ) ;
#64631 = CARTESIAN_POINT ( 'NONE',  ( 201.9261197471746527, 289.7920994275355042, -82.41291490543511600 ) ) ;
#64632 = CARTESIAN_POINT ( 'NONE',  ( -24.22755737512878227, -272.9009294774529053, -194.9327814821474760 ) ) ;
#64633 = CARTESIAN_POINT ( 'NONE',  ( -41.96860252685179660, -299.8536385514914855, -196.2702463755994131 ) ) ;
#64634 = CARTESIAN_POINT ( 'NONE',  ( -37.25070687912403145, -290.3661654521764603, -343.8542142568012423 ) ) ;
#64635 = CARTESIAN_POINT ( 'NONE',  ( -110.0084034461427649, -291.7639882115923911, -260.3002605963773703 ) ) ;
#64636 = ORIENTED_EDGE ( 'NONE', *, *, #68796, .T. ) ;
#64637 = CARTESIAN_POINT ( 'NONE',  ( -89.45738539644557363, -298.2808080211027573, -213.9262081998626286 ) ) ;
#64638 = CARTESIAN_POINT ( 'NONE',  ( -33.24146853771588894, -286.5973812609461788, -197.3648607540476405 ) ) ;
#64639 = CARTESIAN_POINT ( 'NONE',  ( 38.16465939731381951, -294.1764408385868705, -256.1151188210793634 ) ) ;
#64640 = CARTESIAN_POINT ( 'NONE',  ( 0.5156907188606600911, -295.0539999411656140, -337.3564686226543472 ) ) ;
#64641 = CARTESIAN_POINT ( 'NONE',  ( 33.44658187695048923, -293.9541882321916546, -288.1942090019722400 ) ) ;
#64642 = VERTEX_POINT ( 'NONE', #39291 ) ;
#64643 = CARTESIAN_POINT ( 'NONE',  ( -35.58229619559588741, -275.9941843413375864, -194.8087156026683147 ) ) ;
#64644 = EDGE_LOOP ( 'NONE', ( #9540, #1878, #69540, #85542, #41963, #48748 ) ) ;
#64645 = CARTESIAN_POINT ( 'NONE',  ( -113.9820002251451854, -278.1517710701338615, -263.0135606456025812 ) ) ;
#64646 = CARTESIAN_POINT ( 'NONE',  ( -29.88903592127486419, -272.5479225923768354, -196.9383816469575095 ) ) ;
#64647 = CARTESIAN_POINT ( 'NONE',  ( -33.80335719823045793, -299.3024927178125267, -196.9632974387495494 ) ) ;
#64648 = CARTESIAN_POINT ( 'NONE',  ( 31.33482123755863213, -276.1553232386330592, -244.9260268507880483 ) ) ;
#64649 = CARTESIAN_POINT ( 'NONE',  ( -55.11858395926975618, -275.5867060649601967, -196.4831347091606801 ) ) ;
#64650 = CARTESIAN_POINT ( 'NONE',  ( 13.74908610780818563, -274.3608453319600358, -325.8228932254388042 ) ) ;
#64651 = CARTESIAN_POINT ( 'NONE',  ( -52.66453942647950015, -298.5021706263122496, -198.8311675679265420 ) ) ;
#64652 = CARTESIAN_POINT ( 'NONE',  ( -7.768034845374670816, -293.2315518164654122, -337.7600629323433168 ) ) ;
#64653 = CARTESIAN_POINT ( 'NONE',  ( 222.8344101925596306, 0.000000000000000000, 10.00000000000000000 ) ) ;
#64654 = CARTESIAN_POINT ( 'NONE',  ( -112.3431469562897718, -279.2592208192483554, -253.2056559578821293 ) ) ;
#64655 = EDGE_CURVE ( 'NONE', #30245, #58159, #50414, .T. ) ;
#64656 = CARTESIAN_POINT ( 'NONE',  ( -24.32751793415375730, -277.0481772360093373, -342.2431409196510685 ) ) ;
#64657 = CARTESIAN_POINT ( 'NONE',  ( -49.25133195738426650, -284.5883691534731952, -194.7335325952351184 ) ) ;
#64658 = CARTESIAN_POINT ( 'NONE',  ( -62.26183845851925724, -299.7289374515877967, -199.4455686927227021 ) ) ;
#64659 = CARTESIAN_POINT ( 'NONE',  ( 82.61792974232589870, -301.9867274997020559, -195.9612250618527582 ) ) ;
#64660 = CARTESIAN_POINT ( 'NONE',  ( 16.09939010480643518, -286.0319170857039808, -220.3761228436786155 ) ) ;
#64661 = CARTESIAN_POINT ( 'NONE',  ( -95.57442760217497835, -277.4275409691693994, -224.6578702495095854 ) ) ;
#64662 = CARTESIAN_POINT ( 'NONE',  ( -87.92255680118810801, -277.9031965931899322, -216.8402512598194392 ) ) ;
#64663 = CARTESIAN_POINT ( 'NONE',  ( -108.3908751323648687, -286.2398479179511241, -294.5401914223550079 ) ) ;
#64664 = CARTESIAN_POINT ( 'NONE',  ( -29.65667141302510146, -278.1579032777492557, -343.4059370589894797 ) ) ;
#64665 = PLANE ( 'NONE',  #20061 ) ;
#64666 = CARTESIAN_POINT ( 'NONE',  ( 25.49651181853103310, -273.3769838959071876, -227.2357833895700310 ) ) ;
#64667 = CARTESIAN_POINT ( 'NONE',  ( -8.938874093622489525, -275.0850226053447614, -202.9486001580102936 ) ) ;
#64668 = CARTESIAN_POINT ( 'NONE',  ( 18.74336585502158314, -282.8570347907921132, -220.2968544067906578 ) ) ;
#64669 = PLANE ( 'NONE',  #83709 ) ;
#64670 = CARTESIAN_POINT ( 'NONE',  ( 37.13330947979401486, -289.3087279003423760, -257.5263366218349006 ) ) ;
#64671 = CARTESIAN_POINT ( 'NONE',  ( -7.618056273180739524, -290.4415798260847055, -201.4888150816176449 ) ) ;
#64672 = PLANE ( 'NONE',  #73869 ) ;
#64673 = CARTESIAN_POINT ( 'NONE',  ( -43.50690766080450800, -272.6576082382700292, -197.0759630084056653 ) ) ;
#64674 = CARTESIAN_POINT ( 'NONE',  ( 35.43199096186359043, -291.5015898185102969, -255.7031724204378236 ) ) ;
#64675 = CARTESIAN_POINT ( 'NONE',  ( 142.9247625494386114, 180.1091408837567371, -243.7470944784683127 ) ) ;
#64676 = DIRECTION ( 'NONE',  ( 0.000000000000000000, -0.000000000000000000, -1.000000000000000000 ) ) ;
#64677 = CARTESIAN_POINT ( 'NONE',  ( -51.57512821632436584, -287.7109146105174773, -345.3285594210822183 ) ) ;
#64678 = CARTESIAN_POINT ( 'NONE',  ( -89.44481840427226871, -285.4008904394593173, -322.6985455075389950 ) ) ;
#64679 = CARTESIAN_POINT ( 'NONE',  ( -15.68057846130173338, -284.5683803552137761, -197.4725982742139081 ) ) ;
#64680 = CARTESIAN_POINT ( 'NONE',  ( 3.734043674811053926, -283.9130063366745844, -331.4814122082969448 ) ) ;
#64681 = CARTESIAN_POINT ( 'NONE',  ( -84.95915126408831952, -284.5320359941491120, -325.9055153037097625 ) ) ;
#64682 = CARTESIAN_POINT ( 'NONE',  ( -110.7214783712935287, -292.7510963614427055, -253.2200867269018829 ) ) ;
#64683 = CARTESIAN_POINT ( 'NONE',  ( -3.839146081167362112, -274.8153525920508287, -201.0406029347051913 ) ) ;
#64684 = CARTESIAN_POINT ( 'NONE',  ( -112.8141733872998458, -288.5856577071867264, -273.9970464185900028 ) ) ;
#64685 = CARTESIAN_POINT ( 'NONE',  ( -9.211819363219134971, -276.6943583624274083, -342.0389374817232806 ) ) ;
#64686 = CARTESIAN_POINT ( 'NONE',  ( 2.467899391831208433, -296.4960477200129958, -333.5653794872768572 ) ) ;
#64687 = CARTESIAN_POINT ( 'NONE',  ( 185.2169494693457921, 275.0000000000000568, 22.91843887563416615 ) ) ;
#64688 = CARTESIAN_POINT ( 'NONE',  ( -54.49178911615187815, -300.3376638359845856, -195.3683826091709363 ) ) ;
#64689 = CARTESIAN_POINT ( 'NONE',  ( -92.94312924394861852, -282.5566499234737421, -318.4398684498609668 ) ) ;
#64690 = CARTESIAN_POINT ( 'NONE',  ( -8.287617366962106047, -278.4323822918511269, -201.2034140387603713 ) ) ;
#64691 = CARTESIAN_POINT ( 'NONE',  ( -15.08038611036102772, -296.7263302168457244, -194.1670541500574529 ) ) ;
#64692 = CARTESIAN_POINT ( 'NONE',  ( 35.20618119564122850, -275.0243867483887925, -279.7476395292657116 ) ) ;
#64693 = CARTESIAN_POINT ( 'NONE',  ( -33.49138783198756641, -293.6215868464246341, -196.7558249745424916 ) ) ;
#64694 = CARTESIAN_POINT ( 'NONE',  ( 33.87376742875545688, -294.2681414203026407, -253.2264326632809741 ) ) ;
#64695 = CARTESIAN_POINT ( 'NONE',  ( -5.984411523326589766, -295.9636969250614698, -340.1466374372848236 ) ) ;
#64696 = CARTESIAN_POINT ( 'NONE',  ( -104.7613973143008508, -296.7608554442849709, -242.3685397553790040 ) ) ;
#64697 = CARTESIAN_POINT ( 'NONE',  ( -110.2899331885888472, -292.3285804382922493, -287.7839749952365196 ) ) ;
#64698 = CARTESIAN_POINT ( 'NONE',  ( -61.22965565113217679, -283.5205110774961668, -343.6176596128119058 ) ) ;
#64699 = CARTESIAN_POINT ( 'NONE',  ( 15.18797384254098048, -272.9239223906698726, -215.7631433736737279 ) ) ;
#64700 = CARTESIAN_POINT ( 'NONE',  ( -7.341170417150187255, -286.2680397477288921, -199.3892431055238035 ) ) ;
#64701 = CARTESIAN_POINT ( 'NONE',  ( -15.88446999061008214, -278.7532821440228190, -341.9096210679908268 ) ) ;
#64702 = CARTESIAN_POINT ( 'NONE',  ( -52.12475683126957904, -284.9169705440760367, -198.6333710369109724 ) ) ;
#64703 = CARTESIAN_POINT ( 'NONE',  ( -2.746512316524156283, -286.5945727672310568, -336.9056416640585780 ) ) ;
#64704 = CARTESIAN_POINT ( 'NONE',  ( -82.08396892746139883, -205.6231916066184624, -355.0661004095303497 ) ) ;
#64705 = CARTESIAN_POINT ( 'NONE',  ( -42.67236761581845883, -285.4907690970902649, -197.4816688080940708 ) ) ;
#64706 = CARTESIAN_POINT ( 'NONE',  ( 38.88462032965388460, -282.8590533884334945, -278.4612095447548086 ) ) ;
#64707 = CARTESIAN_POINT ( 'NONE',  ( -87.24061519651937147, -288.7863501311317691, -328.7654861955888350 ) ) ;
#64708 = CARTESIAN_POINT ( 'NONE',  ( -104.1025956989616645, -280.6330467546099499, -233.6266214402496644 ) ) ;
#64709 = CARTESIAN_POINT ( 'NONE',  ( -111.6112618883273342, -280.0991799311533441, -251.9407611819490285 ) ) ;
#64710 = CARTESIAN_POINT ( 'NONE',  ( -16.91968232517835347, -280.1566730169467405, -200.2758756462107783 ) ) ;
#64711 = CARTESIAN_POINT ( 'NONE',  ( -82.07645398955150995, -275.4191489984258396, -210.5413387400024021 ) ) ;
#64712 = CARTESIAN_POINT ( 'NONE',  ( 37.78392580287127345, -293.7640804251029181, -287.3067295327173838 ) ) ;
#64713 = CARTESIAN_POINT ( 'NONE',  ( -45.56820836405109532, -287.1770306973840547, -344.5512208532886689 ) ) ;
#64714 = CARTESIAN_POINT ( 'NONE',  ( -30.78661262731542436, -293.7336892799484644, -194.3913786101214782 ) ) ;
#64715 = CARTESIAN_POINT ( 'NONE',  ( -101.4783850978630682, -295.9557233611561173, -234.8546155652680909 ) ) ;
#64716 = CARTESIAN_POINT ( 'NONE',  ( 28.13301183152943707, -283.9461790962319014, -305.7782930399445149 ) ) ;
#64717 = CARTESIAN_POINT ( 'NONE',  ( -104.9830836151757012, -295.8504864989470207, -297.8698570785538209 ) ) ;
#64718 = EDGE_CURVE ( 'NONE', #73473, #75506, #85040, .T. ) ;
#64719 = CARTESIAN_POINT ( 'NONE',  ( 15.21627682194673881, -293.8528386752993242, -214.4388500009942220 ) ) ;
#64720 = CARTESIAN_POINT ( 'NONE',  ( -11.71517612459890323, -281.0461312422029323, -201.8446504206062002 ) ) ;
#64721 = CARTESIAN_POINT ( 'NONE',  ( -5.201826432360350694, -273.5236673502162148, -200.6485026771076718 ) ) ;
#64722 = CARTESIAN_POINT ( 'NONE',  ( -87.31189124135524082, -290.3787590148033928, -328.8801131787508325 ) ) ;
#64723 = CARTESIAN_POINT ( 'NONE',  ( -80.87157440323589697, -281.7752299061435224, -332.4366935245436139 ) ) ;
#64724 = CARTESIAN_POINT ( 'NONE',  ( -110.7603945291620704, -290.5925957306848204, -293.6747970450525145 ) ) ;
#64725 = CARTESIAN_POINT ( 'NONE',  ( 34.03224866874087695, -288.0895464783077955, -285.8420643823129126 ) ) ;
#64726 = DIRECTION ( 'NONE',  ( -0.000000000000000000, 1.000000000000000000, 0.000000000000000000 ) ) ;
#64727 = CARTESIAN_POINT ( 'NONE',  ( -40.95418676001914093, -138.9741238729967563, -362.5036135750506219 ) ) ;
#64728 = CARTESIAN_POINT ( 'NONE',  ( -30.40625769401537326, -125.0523020468976227, -360.4922289175208903 ) ) ;
#64729 = CARTESIAN_POINT ( 'NONE',  ( -110.4683760289727132, -275.8380690714489560, -287.0191576251351080 ) ) ;
#64730 = CARTESIAN_POINT ( 'NONE',  ( -108.4441905920833449, -277.9762095854501354, -253.1263398486288168 ) ) ;
#64731 = EDGE_LOOP ( 'NONE', ( #45690, #55393, #85896, #5795 ) ) ;
#64732 = CARTESIAN_POINT ( 'NONE',  ( -30.21872262107783058, -279.0645635344039306, -197.3483040412711205 ) ) ;
#64733 = CARTESIAN_POINT ( 'NONE',  ( 37.92561291005537782, -275.0161551272126985, -254.1564242120706183 ) ) ;
#64734 = CARTESIAN_POINT ( 'NONE',  ( 190.6894252310336526, 268.2488200997306649, -138.1386062953752401 ) ) ;
#64735 = CARTESIAN_POINT ( 'NONE',  ( -28.27675326729536920, -278.7396257917655475, -194.4367416818954553 ) ) ;
#64736 = CARTESIAN_POINT ( 'NONE',  ( -105.6279316232924117, -282.1755075324275595, -300.5080479741156410 ) ) ;
#64737 = CARTESIAN_POINT ( 'NONE',  ( -106.8552173197297464, -298.7105353221991777, -239.5414464643715746 ) ) ;
#64738 = CARTESIAN_POINT ( 'NONE',  ( -17.42183542464008639, -292.8084383920509026, -200.0149024682672518 ) ) ;
#64739 = ORIENTED_EDGE ( 'NONE', *, *, #30011, .F. ) ;
#64740 = CARTESIAN_POINT ( 'NONE',  ( -61.43236756502461304, -288.0565608071930797, -339.7936983753351683 ) ) ;
#64741 = CARTESIAN_POINT ( 'NONE',  ( -49.71103001416717149, -274.5499064965100615, -194.4106607895813283 ) ) ;
#64742 = CARTESIAN_POINT ( 'NONE',  ( -96.28137092940995956, -273.1562831760284666, -227.2060860369406043 ) ) ;
#64743 = ORIENTED_EDGE ( 'NONE', *, *, #75497, .F. ) ;
#64744 = CARTESIAN_POINT ( 'NONE',  ( 200.9306832106270804, -148.7221692137691491, 0.000000000000000000 ) ) ;
#64745 = DIRECTION ( 'NONE',  ( 0.000000000000000000, 0.9681751575201842375, 0.2502735790305606889 ) ) ;
#64746 = CARTESIAN_POINT ( 'NONE',  ( -66.82358179535859222, -281.5890009728792052, -200.7900546510638264 ) ) ;
#64747 = EDGE_CURVE ( 'NONE', #93704, #38347, #26522, .T. ) ;
#64748 = DIRECTION ( 'NONE',  ( 0.9764705882352960886, 0.000000000000000000, 0.2156506209390900708 ) ) ;
#64749 = CARTESIAN_POINT ( 'NONE',  ( 32.26578842316664009, -282.3258787783213393, -247.2007033208231235 ) ) ;
#64750 = CARTESIAN_POINT ( 'NONE',  ( -14.55330129389469107, -282.1035608530683021, -197.8169053525276411 ) ) ;
#64752 = VECTOR ( 'NONE', #74815, 1000.000000000000000 ) ;
#64751 = CARTESIAN_POINT ( 'NONE',  ( -110.2273431385451090, -283.7114544507192591, -262.7136045495970507 ) ) ;
#64753 = CARTESIAN_POINT ( 'NONE',  ( -111.3924216447653350, -280.4804229353496225, -265.1308100496698898 ) ) ;
#64754 = CARTESIAN_POINT ( 'NONE',  ( 23.02274142192727524, -274.6170503720201737, -312.7197485551346290 ) ) ;
#64755 = CARTESIAN_POINT ( 'NONE',  ( 209.1021009645937738, 27.84274218592230810, 12.05941621939738084 ) ) ;
#64756 = DIRECTION ( 'NONE',  ( -0.000000000000000000, 0.000000000000000000, -1.000000000000000000 ) ) ;
#64757 = CARTESIAN_POINT ( 'NONE',  ( -82.44322468574870300, -278.4536609344096405, -332.5705328858309144 ) ) ;
#64758 = VERTEX_POINT ( 'NONE', #90413 ) ;
#64759 = CARTESIAN_POINT ( 'NONE',  ( -96.60896541417068306, -276.4745423961463189, -318.6102098068657824 ) ) ;
#64760 = ORIENTED_EDGE ( 'NONE', *, *, #34566, .F. ) ;
#64761 = CARTESIAN_POINT ( 'NONE',  ( 180.7149167944524493, -12.49482340714361506, -3.999999999999998224 ) ) ;
#64762 = CARTESIAN_POINT ( 'NONE',  ( -85.04132537923237578, -285.6866718536684857, -328.6976635664029232 ) ) ;
#64763 = CARTESIAN_POINT ( 'NONE',  ( 35.36620734229189367, -292.8622300481466141, -278.9396012712676907 ) ) ;
#64764 = ADVANCED_FACE ( 'NONE', ( #25570 ), #63003, .F. ) ;
#64765 = CARTESIAN_POINT ( 'NONE',  ( 31.59236124351189900, -287.3406237297907069, -304.5606190968654232 ) ) ;
#64766 = CARTESIAN_POINT ( 'NONE',  ( -60.27157930858084001, -283.9905997117509742, -199.9892865950615999 ) ) ;
#64768 = CARTESIAN_POINT ( 'NONE',  ( 18.57659422719453701, -286.4742968597512913, -318.9261553990029938 ) ) ;
#64767 = CARTESIAN_POINT ( 'NONE',  ( -72.64083230934006963, -284.1498186324519111, -205.7763137370687616 ) ) ;
#64769 = CARTESIAN_POINT ( 'NONE',  ( 35.96326199687488412, -282.8054648719526085, -274.0371255526139294 ) ) ;
#64770 = CARTESIAN_POINT ( 'NONE',  ( 22.06469534346717865, -272.9245274711426532, -224.5594142714235204 ) ) ;
#64771 = CARTESIAN_POINT ( 'NONE',  ( -91.32175294512047969, -283.6995970974033412, -216.5782739480239343 ) ) ;
#64772 = CARTESIAN_POINT ( 'NONE',  ( -55.55917935315227396, -297.2867801693913634, -343.1149776490763088 ) ) ;
#64773 = CARTESIAN_POINT ( 'NONE',  ( -5.526215443668818672, -284.4695189624267755, -202.2596982827882073 ) ) ;
#64774 = CARTESIAN_POINT ( 'NONE',  ( -109.2721266827422113, -279.3115620963374113, -284.1903962125614953 ) ) ;
#64775 = CARTESIAN_POINT ( 'NONE',  ( 32.15443894610123721, -289.1778863349051107, -241.5841114757561172 ) ) ;
#64776 = CARTESIAN_POINT ( 'NONE',  ( 193.6552470326849402, 275.5797763526087465, 16.89672165344822474 ) ) ;
#64777 = CARTESIAN_POINT ( 'NONE',  ( 195.4781563537916043, 27.48493576247232895, 13.99999999999999822 ) ) ;
#64778 = CARTESIAN_POINT ( 'NONE',  ( 22.89607022198499209, -296.0915531886318490, -315.9760850922224904 ) ) ;
#64779 = CARTESIAN_POINT ( 'NONE',  ( -112.1518307317253687, -276.6204681987582035, -265.0277320497596634 ) ) ;
#64780 = CARTESIAN_POINT ( 'NONE',  ( -111.0743301631594164, -290.0211409249805570, -248.7357142002668411 ) ) ;
#64781 = CARTESIAN_POINT ( 'NONE',  ( 18.56528400437992588, -292.6309045405507732, -318.5555759000557714 ) ) ;
#64782 = CARTESIAN_POINT ( 'NONE',  ( -9.042077963082315151, -279.1150146316199425, -202.5350546731747556 ) ) ;
#64783 = CARTESIAN_POINT ( 'NONE',  ( -92.16686870826306688, -271.3409231206380241, -219.9883575876487782 ) ) ;
#64784 = CARTESIAN_POINT ( 'NONE',  ( 0.1462936821208547233, -293.8778019906856116, -207.1480354904180956 ) ) ;
#64785 = CARTESIAN_POINT ( 'NONE',  ( 21.31550574532285580, -278.6948066931273615, -317.0979686699210447 ) ) ;
#64786 = CARTESIAN_POINT ( 'NONE',  ( -71.77861896020590393, -293.9788779815642670, -338.4552174061741425 ) ) ;
#64787 = CARTESIAN_POINT ( 'NONE',  ( -29.06337183588486539, -290.5456214251294114, -343.6953507472241540 ) ) ;
#64788 = CARTESIAN_POINT ( 'NONE',  ( -58.63299134959753900, -290.0203647536698668, -197.4182983922744086 ) ) ;
#64789 = CARTESIAN_POINT ( 'NONE',  ( -72.62555981011973927, -290.9543782178983520, -334.9399393092668902 ) ) ;
#64790 = CARTESIAN_POINT ( 'NONE',  ( 152.4536156746142410, 275.0000000000000568, 11.49999999999999289 ) ) ;
#64791 = CARTESIAN_POINT ( 'NONE',  ( -56.09714401786292370, -290.1026763328785023, -341.1303718904458719 ) ) ;
#64792 = CARTESIAN_POINT ( 'NONE',  ( 180.2288731078812702, 215.0000000000000568, -24.90909090909092782 ) ) ;
#64793 = CIRCLE ( 'NONE', #93474, 28.04691768583012035 ) ;
#64794 = CARTESIAN_POINT ( 'NONE',  ( -113.7925274205179420, -291.8178809281456552, -265.5362113576314869 ) ) ;
#64796 = CARTESIAN_POINT ( 'NONE',  ( -95.11439130822638788, -291.1804236143703974, -225.7369524015254569 ) ) ;
#64795 = CARTESIAN_POINT ( 'NONE',  ( 19.83491766168293680, -278.8951409268548787, -221.2574672631898807 ) ) ;
#64797 = CARTESIAN_POINT ( 'NONE',  ( -96.80381148168737582, -279.5424952283311768, -221.4529764343397744 ) ) ;
#64798 = CARTESIAN_POINT ( 'NONE',  ( 2.079664409559733418, -282.2061615606692158, -336.4799527386016393 ) ) ;
#64799 = CARTESIAN_POINT ( 'NONE',  ( 19.30299774851949834, -284.8699592232133000, -221.2044413910540470 ) ) ;
#64800 = DIRECTION ( 'NONE',  ( -0.8429829950866658539, -0.5379402104274361163, 3.232101055797385739E-15 ) ) ;
#64801 = CARTESIAN_POINT ( 'NONE',  ( 35.69654490444180084, -279.8648885396994501, -283.7092805312842643 ) ) ;
#64802 = CARTESIAN_POINT ( 'NONE',  ( -112.3553692517585318, -282.5211962451222121, -272.7591947047818053 ) ) ;
#64803 = CARTESIAN_POINT ( 'NONE',  ( 156.4851178187871596, 16.95599219719301232, 6.999999999999998224 ) ) ;
#64804 = CARTESIAN_POINT ( 'NONE',  ( -111.1616768445554158, -276.7874002616387088, -289.7339702682834854 ) ) ;
#64805 = CARTESIAN_POINT ( 'NONE',  ( -112.6919010022137684, -283.6551827870788998, -255.8078313250566964 ) ) ;
#64806 = CARTESIAN_POINT ( 'NONE',  ( -100.8630312116333130, -273.8524736366951515, -233.9598768378228328 ) ) ;
#64807 = DIRECTION ( 'NONE',  ( -0.000000000000000000, -0.000000000000000000, -1.000000000000000000 ) ) ;
#64808 = CARTESIAN_POINT ( 'NONE',  ( -104.2905159907218433, -292.5668962447462604, -239.3079946676770646 ) ) ;
#64809 = CARTESIAN_POINT ( 'NONE',  ( -27.09365417432926293, -275.6051259247636267, -194.5876656206886821 ) ) ;
#64810 = CARTESIAN_POINT ( 'NONE',  ( -5.060556969323847021, -276.2818449749674983, -335.8732203546749133 ) ) ;
#64811 = CARTESIAN_POINT ( 'NONE',  ( 19.50454607328424572, -296.2306114705191931, -319.3041680958199322 ) ) ;
#64812 = CARTESIAN_POINT ( 'NONE',  ( -36.08471351486991807, -289.2035130133343159, -347.3639678062371559 ) ) ;
#64813 = CARTESIAN_POINT ( 'NONE',  ( -6.789770406774897182, -278.5298736902030328, -201.2392684336859645 ) ) ;
#64814 = CARTESIAN_POINT ( 'NONE',  ( -73.43183545768000897, -291.4202271591936437, -202.3278228347040226 ) ) ;
#64815 = CARTESIAN_POINT ( 'NONE',  ( -47.01371349523969911, -290.9850267683520997, -197.7673124260751081 ) ) ;
#64816 = CARTESIAN_POINT ( 'NONE',  ( -28.02228166383421382, -292.9338161723024996, -344.8317667229835024 ) ) ;
#64817 = VERTEX_POINT ( 'NONE', #55410 ) ;
#64818 = CARTESIAN_POINT ( 'NONE',  ( 200.2349812190172713, 66.43136063442169359, 7.741079165001063522 ) ) ;
#64819 = CARTESIAN_POINT ( 'NONE',  ( 12.95005438590779079, -292.2853845396969632, -217.3636853140565393 ) ) ;
#64820 = FACE_OUTER_BOUND ( 'NONE', #92496, .T. ) ;
#64821 = CARTESIAN_POINT ( 'NONE',  ( 27.33386217378598815, -279.4809262143061233, -301.5434626090942629 ) ) ;
#64822 = CARTESIAN_POINT ( 'NONE',  ( -111.3683060265434790, -295.3555966267059603, -290.6806118878683378 ) ) ;
#64823 = CARTESIAN_POINT ( 'NONE',  ( -112.5168896377793715, -286.0496396853866941, -255.8728551344655671 ) ) ;
#64824 = CARTESIAN_POINT ( 'NONE',  ( 35.65515926231452681, -287.3944036716816868, -271.0382617056125127 ) ) ;
#64825 = CARTESIAN_POINT ( 'NONE',  ( 35.30591346791839413, -276.9096467825079344, -257.9156701971692769 ) ) ;
#64826 = CARTESIAN_POINT ( 'NONE',  ( 29.86471317700003070, -292.0035824842242391, -302.9632282876810336 ) ) ;
#64827 = CARTESIAN_POINT ( 'NONE',  ( 36.63343835856003494, -295.2813660653665124, -267.9835358271650989 ) ) ;
#64828 = CARTESIAN_POINT ( 'NONE',  ( 16.81382174454465073, -275.0541120063930407, -319.9208516148004833 ) ) ;
#64829 = ORIENTED_EDGE ( 'NONE', *, *, #5338, .T. ) ;
#64830 = CARTESIAN_POINT ( 'NONE',  ( 194.6889851074543287, 41.25212764115960340, 14.04815903671776312 ) ) ;
#64831 = CARTESIAN_POINT ( 'NONE',  ( -98.26032971053273002, -295.5905422204444335, -317.4213438791338717 ) ) ;
#64832 = CARTESIAN_POINT ( 'NONE',  ( 23.14579132524312044, -290.0670783776265012, -313.7497982710228825 ) ) ;
#64833 = CARTESIAN_POINT ( 'NONE',  ( 201.4659665719736097, 295.2841405640494372, -54.00000000003616663 ) ) ;
#64834 = CARTESIAN_POINT ( 'NONE',  ( -46.10824021721057875, -299.0230967147259094, -194.1729280565668034 ) ) ;
#64835 = CARTESIAN_POINT ( 'NONE',  ( 13.20405196619358534, -287.4326782644043305, -217.4801194004139120 ) ) ;
#64836 = ORIENTED_EDGE ( 'NONE', *, *, #1671, .F. ) ;
#64837 = CARTESIAN_POINT ( 'NONE',  ( -92.89516848816764139, -278.3381443315037700, -217.3075237313009609 ) ) ;
#64838 = CARTESIAN_POINT ( 'NONE',  ( 34.35944555851182969, -294.5560902270212864, -298.1506572658657319 ) ) ;
#64839 = CARTESIAN_POINT ( 'NONE',  ( -72.62008019093364908, -287.6536990479655174, -337.4259295986626057 ) ) ;
#64840 = CARTESIAN_POINT ( 'NONE',  ( -64.25481809761065222, -295.7271921037819880, -342.4820467942532218 ) ) ;
#64841 = CARTESIAN_POINT ( 'NONE',  ( 29.51111778551385356, -294.2804839683433897, -299.7343749299255364 ) ) ;
#64842 = CARTESIAN_POINT ( 'NONE',  ( 196.1825486463387165, 72.66602830303396843, -11.70860092535009045 ) ) ;
#64843 = CARTESIAN_POINT ( 'NONE',  ( 196.6877655503061533, 293.9636489450776367, -44.00000000000000000 ) ) ;
#64844 = LINE ( 'NONE', #30209, #38600 ) ;
#64845 = CARTESIAN_POINT ( 'NONE',  ( -3.811636168764664045, -288.0065628828402851, -201.8015367330476693 ) ) ;
#64846 = CARTESIAN_POINT ( 'NONE',  ( 44.71564893372296723, -285.0523547857347353, -270.3937649182068412 ) ) ;
#64847 = CARTESIAN_POINT ( 'NONE',  ( -101.8012386096887809, -278.4532664994625861, -228.3329224186558406 ) ) ;
#64848 = CARTESIAN_POINT ( 'NONE',  ( -6.474565824664024305, -284.6460189540223382, -338.5459087240757867 ) ) ;
#64849 = CARTESIAN_POINT ( 'NONE',  ( -109.6728099937270144, -282.8141203514168751, -294.9947705315508983 ) ) ;
#64850 = CARTESIAN_POINT ( 'NONE',  ( 6.676831608318957834, -286.5286358453101343, -330.4560264799730476 ) ) ;
#64851 = CARTESIAN_POINT ( 'NONE',  ( 38.47165267407766009, -277.4224054792246648, -271.1349953099904724 ) ) ;
#64852 = CARTESIAN_POINT ( 'NONE',  ( -43.48813426490022493, -274.3057975246948104, -197.5483911267091912 ) ) ;
#64853 = VERTEX_POINT ( 'NONE', #33612 ) ;
#64854 = CARTESIAN_POINT ( 'NONE',  ( -68.74315866602611891, -294.1585618424003314, -336.8218534164845437 ) ) ;
#64856 = CARTESIAN_POINT ( 'NONE',  ( -59.75701063985993500, -279.1026896116431431, -200.7272368739066337 ) ) ;
#64855 = CARTESIAN_POINT ( 'NONE',  ( -99.17509273922071600, -278.0151929862021234, -309.2580087107771760 ) ) ;
#64857 = CARTESIAN_POINT ( 'NONE',  ( -38.36712413510893782, -275.1192458227329212, -193.6770843333568166 ) ) ;
#64858 = CARTESIAN_POINT ( 'NONE',  ( -113.8363169450933015, -277.2958864952799445, -274.4332569294710993 ) ) ;
#64859 = CARTESIAN_POINT ( 'NONE',  ( -78.81524805502048991, -207.3136162032604659, -354.6738105741294476 ) ) ;
#64860 = CARTESIAN_POINT ( 'NONE',  ( -99.45325900190022139, -298.5717068622785177, -225.8553818588908371 ) ) ;
#64861 = ADVANCED_FACE ( 'NONE', ( #47328 ), #91833, .T. ) ;
#64862 = CARTESIAN_POINT ( 'NONE',  ( -106.6662871844225293, -275.4805209788417528, -237.0123917617630980 ) ) ;
#64863 = ORIENTED_EDGE ( 'NONE', *, *, #42341, .F. ) ;
#64864 = AXIS2_PLACEMENT_3D ( 'NONE', #8069, #36958, #65871 ) ;
#64865 = DIRECTION ( 'NONE',  ( 0.000000000000000000, 0.000000000000000000, -1.000000000000000000 ) ) ;
#64866 = CARTESIAN_POINT ( 'NONE',  ( -99.88016898236796237, -286.1578177189136341, -232.0130187540122790 ) ) ;
#64867 = CARTESIAN_POINT ( 'NONE',  ( -54.75445595234098306, -287.5914494448043115, -196.3964646278142254 ) ) ;
#64868 = CARTESIAN_POINT ( 'NONE',  ( 35.78256163974624826, -286.8738185703300019, -268.3178757458759947 ) ) ;
#64869 = CARTESIAN_POINT ( 'NONE',  ( -112.4663634463238537, -283.8519408983603398, -286.9687025415564108 ) ) ;
#64870 = CARTESIAN_POINT ( 'NONE',  ( -5.191769931830755525, -278.8824211001969502, -203.9320399657017902 ) ) ;
#64871 = CARTESIAN_POINT ( 'NONE',  ( -68.08042643044159092, -287.5045852517947651, -202.7889625602731201 ) ) ;
#64872 = CARTESIAN_POINT ( 'NONE',  ( 7.580146836008246680, -279.1573380924104413, -211.8779183624485256 ) ) ;
#64873 = CARTESIAN_POINT ( 'NONE',  ( -81.09967080430737951, -278.9760764028137032, -329.4075698570590589 ) ) ;
#64874 = CARTESIAN_POINT ( 'NONE',  ( 26.68743840101996057, -275.5629732485845693, -235.0668034416792977 ) ) ;
#64875 = CARTESIAN_POINT ( 'NONE',  ( -75.47937926186932600, -288.3440620631050706, -336.7954927367333653 ) ) ;
#64876 = CARTESIAN_POINT ( 'NONE',  ( -41.55004729521917284, -283.9065770576856380, -347.1365299970082674 ) ) ;
#64877 = CARTESIAN_POINT ( 'NONE',  ( 9.176584106296594712, -282.9246678125839480, -331.6438735908672584 ) ) ;
#64878 = EDGE_LOOP ( 'NONE', ( #85973, #20567, #51506, #6733 ) ) ;
#64879 = EDGE_LOOP ( 'NONE', ( #42185, #49088, #12968, #77652 ) ) ;
#64880 = CARTESIAN_POINT ( 'NONE',  ( 170.8178014930282700, 8.542400036368780647, 9.000000000000001776 ) ) ;
#64881 = CARTESIAN_POINT ( 'NONE',  ( -26.30077655663473735, -290.7734659646230853, -345.3171283168143191 ) ) ;
#64882 = CARTESIAN_POINT ( 'NONE',  ( -112.8758573263596077, -289.0839120606259485, -282.5220953043358350 ) ) ;
#64883 = CARTESIAN_POINT ( 'NONE',  ( -94.78984615908625244, -272.2498265784545310, -224.9395485849079250 ) ) ;
#64884 = EDGE_CURVE ( 'NONE', #58159, #51410, #33785, .T. ) ;
#64885 = CARTESIAN_POINT ( 'NONE',  ( 32.13436253922301944, -293.3250986967233302, -303.4456419533718190 ) ) ;
#64886 = CARTESIAN_POINT ( 'NONE',  ( -75.08750103998879410, -288.0447196432907617, -333.6686178426868992 ) ) ;
#64887 = CARTESIAN_POINT ( 'NONE',  ( 28.39671628957148997, -291.3359022868795591, -236.3547271435378150 ) ) ;
#64888 = CARTESIAN_POINT ( 'NONE',  ( 35.84913324137321666, -288.8377696663205256, -276.4993495235758587 ) ) ;
#64889 = CARTESIAN_POINT ( 'NONE',  ( 31.95455697924148097, -295.6233781216988632, -236.9535640164627637 ) ) ;
#64890 = CARTESIAN_POINT ( 'NONE',  ( -26.41023446725840174, -290.9131880085710122, -344.5601995478144772 ) ) ;
#64891 = CARTESIAN_POINT ( 'NONE',  ( -73.76761629400313325, -289.5694842315243704, -204.6102163961794815 ) ) ;
#64892 = CARTESIAN_POINT ( 'NONE',  ( -5.161021176193295368, -294.4758340443110569, -202.6020382514811615 ) ) ;
#64893 = CARTESIAN_POINT ( 'NONE',  ( -105.7890882556549172, -285.8400331174468647, -244.3157055993873712 ) ) ;
#64894 = CARTESIAN_POINT ( 'NONE',  ( 27.87211595891487903, -295.0547921746466500, -232.9821584515795507 ) ) ;
#64895 = CARTESIAN_POINT ( 'NONE',  ( 208.4306832106271088, 1.000000000000000888, 0.000000000000000000 ) ) ;
#64896 = CARTESIAN_POINT ( 'NONE',  ( 153.9133111279456045, 20.47222690886501795, -13.06183683676589524 ) ) ;
#64897 = CARTESIAN_POINT ( 'NONE',  ( -112.6978367782134711, -274.5675873361152526, -267.5800565663478778 ) ) ;
#64898 = CARTESIAN_POINT ( 'NONE',  ( 35.51415487905948964, -280.6543400406660567, -263.1455633865182904 ) ) ;
#64899 = CARTESIAN_POINT ( 'NONE',  ( -67.38345437760226275, -281.4459563558073683, -339.0954654058396613 ) ) ;
#64900 = CARTESIAN_POINT ( 'NONE',  ( -108.7347667244529390, -296.1120958670094865, -241.8071133479353989 ) ) ;
#64901 = CARTESIAN_POINT ( 'NONE',  ( 33.03221910872545664, -273.4900587956998379, -247.2726227099493883 ) ) ;
#64902 = CARTESIAN_POINT ( 'NONE',  ( -108.5986083724690729, -276.9116082142066944, -248.8258625606869714 ) ) ;
#64903 = CARTESIAN_POINT ( 'NONE',  ( -105.2240762792772557, -298.2424709397903371, -242.1968412317631021 ) ) ;
#64904 = CARTESIAN_POINT ( 'NONE',  ( 35.48831257374818904, -294.8394577455441095, -259.8176760795727205 ) ) ;
#64905 = CARTESIAN_POINT ( 'NONE',  ( 199.0061125298537377, 215.0000000000000568, -7.725424859374024678 ) ) ;
#64906 = CARTESIAN_POINT ( 'NONE',  ( 3.915857296505884211, -295.2833938693804043, -330.7797879609530582 ) ) ;
#64907 = DIRECTION ( 'NONE',  ( -0.000000000000000000, -1.000000000000000000, -0.000000000000000000 ) ) ;
#64909 = CARTESIAN_POINT ( 'NONE',  ( -88.50184912708041907, -295.7937764394198439, -322.5055587534849337 ) ) ;
#64908 = CARTESIAN_POINT ( 'NONE',  ( 36.49155210934362259, -285.7648286151041361, -285.4295508892598718 ) ) ;
#64910 = CARTESIAN_POINT ( 'NONE',  ( -88.32153722872978108, -283.7429556742942509, -328.1389503967723726 ) ) ;
#64911 = CARTESIAN_POINT ( 'NONE',  ( 19.60574515177151511, -287.9231784482374792, -322.1758544495715455 ) ) ;
#64912 = CARTESIAN_POINT ( 'NONE',  ( -91.49703810126871417, -297.7984831134086789, -322.7596501309698738 ) ) ;
#64913 = CARTESIAN_POINT ( 'NONE',  ( 19.89487193438722556, -290.8839165013578167, -222.1532011199816452 ) ) ;
#64914 = CARTESIAN_POINT ( 'NONE',  ( -109.4510998821137520, -278.0871982139832426, -243.6671527312089722 ) ) ;
#64915 = CARTESIAN_POINT ( 'NONE',  ( -106.6379572354042153, -282.4809262143061233, -236.9535640164627068 ) ) ;
#64916 = CARTESIAN_POINT ( 'NONE',  ( 154.9842916688210153, 128.0000000000000568, 12.88888888888890349 ) ) ;
#64917 = CARTESIAN_POINT ( 'NONE',  ( 36.02619794885956139, -286.3921050236789370, -273.7936192847289476 ) ) ;
#64918 = CARTESIAN_POINT ( 'NONE',  ( 197.7156983550588052, 70.58049492527801760, -11.36724305494472453 ) ) ;
#64919 = CARTESIAN_POINT ( 'NONE',  ( 0.000000000000000000, 15.00000000000000000, 15.00000000000000000 ) ) ;
#64920 = CARTESIAN_POINT ( 'NONE',  ( -108.3672566232775978, -297.8901709505469171, -290.4063353878182738 ) ) ;
#64921 = CARTESIAN_POINT ( 'NONE',  ( 24.10700271430414432, -282.3691655434998893, -224.9445657891542680 ) ) ;
#64923 = CARTESIAN_POINT ( 'NONE',  ( 34.72374258919094814, -281.3741612913639756, -282.1364928288355713 ) ) ;
#64922 = CARTESIAN_POINT ( 'NONE',  ( -106.8674499587810516, -294.1930234440782783, -299.5578819612953794 ) ) ;
#64924 = CARTESIAN_POINT ( 'NONE',  ( -94.65015683057279716, -296.0208832418985025, -321.8078052166281395 ) ) ;
#64925 = CARTESIAN_POINT ( 'NONE',  ( -96.66990747832352326, -298.6793800730595194, -226.6262897259971680 ) ) ;
#64926 = CARTESIAN_POINT ( 'NONE',  ( 34.48791835814993334, -285.3294554416447113, -246.7453767825517730 ) ) ;
#64927 = CARTESIAN_POINT ( 'NONE',  ( -111.0941241552230139, -280.3764921216308608, -284.0543474257601702 ) ) ;
#64929 = CARTESIAN_POINT ( 'NONE',  ( -108.4003396995335180, -295.8446261396671275, -252.5875608071127090 ) ) ;
#64928 = AXIS2_PLACEMENT_3D ( 'NONE', #52728, #89632, #38535 ) ;
#64930 = VERTEX_POINT ( 'NONE', #4270 ) ;
#64931 = PLANE ( 'NONE',  #68055 ) ;
#64932 = CARTESIAN_POINT ( 'NONE',  ( -6.552508724816060948, -284.6257539362730995, -338.3742056111131546 ) ) ;
#64933 = LINE ( 'NONE', #42633, #79192 ) ;
#64934 = CARTESIAN_POINT ( 'NONE',  ( -114.2704648735229114, -288.0523547857346784, -270.3284710469133074 ) ) ;
#64935 = CARTESIAN_POINT ( 'NONE',  ( -11.92925525884559335, -275.9269183552944469, -342.9315191208891065 ) ) ;
#64936 = CARTESIAN_POINT ( 'NONE',  ( -3.634370182412778760, -292.3433983063298456, -205.6091611591530466 ) ) ;
#64937 = CARTESIAN_POINT ( 'NONE',  ( 35.17112336764623848, -283.2448801671390015, -283.5695907963116156 ) ) ;
#64938 = CARTESIAN_POINT ( 'NONE',  ( -5.917680616117033665, -278.2321655745086559, -337.1505696092807511 ) ) ;
#64939 = CARTESIAN_POINT ( 'NONE',  ( -41.50483637870826215, -284.7037441069567762, -346.4990941667554125 ) ) ;
#64940 = CARTESIAN_POINT ( 'NONE',  ( 3.599051426031238066, -281.2830818832589443, -331.3404451276120426 ) ) ;
#64941 = CARTESIAN_POINT ( 'NONE',  ( -112.2774090673670173, -280.5124506605142187, -273.4659805666461807 ) ) ;
#64942 = CARTESIAN_POINT ( 'NONE',  ( -112.4437553364018214, -272.9313224066769408, -253.3704938614554862 ) ) ;
#64943 = CARTESIAN_POINT ( 'NONE',  ( 3.499701719940560452, -276.3527600724881950, -335.7000626932079967 ) ) ;
#64944 = CARTESIAN_POINT ( 'NONE',  ( -3.663725490660570738, -296.5243944182886935, -336.7614487047821399 ) ) ;
#64945 = CARTESIAN_POINT ( 'NONE',  ( 219.8344101925596021, 35.72494958537217968, 7.000000000000000000 ) ) ;
#64946 = EDGE_CURVE ( 'NONE', #14859, #92829, #30750, .T. ) ;
#64947 = DIRECTION ( 'NONE',  ( 1.000000000000000000, 0.000000000000000000, 0.000000000000000000 ) ) ;
#64948 = CARTESIAN_POINT ( 'NONE',  ( -58.52898931017722362, -293.4626745613730350, -343.1578428536843148 ) ) ;
#64949 = CARTESIAN_POINT ( 'NONE',  ( -19.25032703536248135, -273.7987968974132968, -199.5224133838598846 ) ) ;
#64950 = CARTESIAN_POINT ( 'NONE',  ( -11.40726733078074950, -293.9039586015770738, -198.5413036611478788 ) ) ;
#64952 = CARTESIAN_POINT ( 'NONE',  ( -1.005805344258491107, -293.7286398533959755, -202.9243960164357929 ) ) ;
#64951 = CARTESIAN_POINT ( 'NONE',  ( -37.30987171927208124, -279.5519495502701943, -345.3611179825600175 ) ) ;
#64953 = CARTESIAN_POINT ( 'NONE',  ( -87.95096575868657851, -291.7615039333078926, -325.5560745152930053 ) ) ;
#64954 = CARTESIAN_POINT ( 'NONE',  ( -110.0654507216758304, -276.7790754417439416, -252.7178606251402755 ) ) ;
#64955 = CARTESIAN_POINT ( 'NONE',  ( -72.30940717321766442, -279.4386687504831457, -336.0913492280743640 ) ) ;
#64956 = CARTESIAN_POINT ( 'NONE',  ( -20.54659779827102994, -292.9147970178929086, -342.9348551313277085 ) ) ;
#64957 = CARTESIAN_POINT ( 'NONE',  ( 21.00409251012510126, -282.7521936363731925, -222.0281689178572435 ) ) ;
#64958 = CARTESIAN_POINT ( 'NONE',  ( -96.17801707996994764, -282.8616657493402613, -314.0934159086996829 ) ) ;
#64959 = ORIENTED_EDGE ( 'NONE', *, *, #50161, .T. ) ;
#64960 = CARTESIAN_POINT ( 'NONE',  ( -95.94124855122180406, -283.6079352944829566, -313.9292303062280780 ) ) ;
#64961 = CARTESIAN_POINT ( 'NONE',  ( -17.08691519550920290, -281.3873889154195354, -196.3933128490536717 ) ) ;
#64962 = CARTESIAN_POINT ( 'NONE',  ( -97.74086255970986770, -282.7143024068138857, -317.4774622581012409 ) ) ;
#64963 = CARTESIAN_POINT ( 'NONE',  ( -110.4389182992568124, -279.1957884895527400, -293.9760891873529545 ) ) ;
#64964 =( LENGTH_UNIT ( ) NAMED_UNIT ( * ) SI_UNIT ( .MILLI., .METRE. ) );
#64965 = CARTESIAN_POINT ( 'NONE',  ( -17.51918670569879311, -278.3210280942863619, -344.0481298137309523 ) ) ;
#64966 = CARTESIAN_POINT ( 'NONE',  ( -67.68488546085839630, -297.9805209788416391, -333.4427485647536855 ) ) ;
#64967 = ORIENTED_EDGE ( 'NONE', *, *, #26330, .T. ) ;
#64968 = ORIENTED_EDGE ( 'NONE', *, *, #56487, .F. ) ;
#64969 = CARTESIAN_POINT ( 'NONE',  ( -91.50745806583132946, -299.2815941995204980, -218.4112298104505498 ) ) ;
#64970 = CARTESIAN_POINT ( 'NONE',  ( -92.19326688385801560, -275.8605346611529399, -321.0639181143576479 ) ) ;
#64971 = CARTESIAN_POINT ( 'NONE',  ( -98.40384439313966425, -292.9217435012909050, -225.1133407510679092 ) ) ;
#64972 = CARTESIAN_POINT ( 'NONE',  ( 35.00981012005320281, -292.7631073201330878, -259.9135520915473307 ) ) ;
#64973 = CARTESIAN_POINT ( 'NONE',  ( -31.83744570529959717, -288.4922379185161958, -347.1549512748050574 ) ) ;
#64974 = CARTESIAN_POINT ( 'NONE',  ( 208.4306832106270804, -147.7221692137691775, 0.000000000000000000 ) ) ;
#64976 = CARTESIAN_POINT ( 'NONE',  ( -5.434517483399896598, -284.8788800529824812, -203.8011664787330517 ) ) ;
#64975 = CARTESIAN_POINT ( 'NONE',  ( 27.59552342027188487, -292.6587633879446457, -310.7316096564471763 ) ) ;
#64977 = CARTESIAN_POINT ( 'NONE',  ( -93.50628927240444455, -293.0927038958209323, -221.8183079224989456 ) ) ;
#64978 = CARTESIAN_POINT ( 'NONE',  ( -67.97475640748461956, -284.7781563470576316, -337.1657536181999717 ) ) ;
#64979 = CARTESIAN_POINT ( 'NONE',  ( -31.83166314781207262, -289.9256057536100002, -346.9802141575967767 ) ) ;
#64980 = CARTESIAN_POINT ( 'NONE',  ( -9.229457628856597040, -280.9222438678889375, -202.9245532462947779 ) ) ;
#64981 = CARTESIAN_POINT ( 'NONE',  ( 37.39312980538593223, -292.5591998034622634, -287.2343709391707307 ) ) ;
#64982 = CARTESIAN_POINT ( 'NONE',  ( -45.99740481066345410, -289.9619579705826595, -346.7635770091013114 ) ) ;
#64983 = CARTESIAN_POINT ( 'NONE',  ( -110.7212541379692965, -290.7516360884237656, -293.6644971242484417 ) ) ;
#64984 = CARTESIAN_POINT ( 'NONE',  ( -41.32505135933491403, -286.1673207976138542, -197.4573793176499521 ) ) ;
#64985 = VERTEX_POINT ( 'NONE', #26036 ) ;
#64986 = DIRECTION ( 'NONE',  ( 0.000000000000000000, 0.000000000000000000, 1.000000000000000000 ) ) ;
#64987 = CARTESIAN_POINT ( 'NONE',  ( 21.34514669769989936, -296.0664174347120934, -318.2997516510645823 ) ) ;
#64988 = CARTESIAN_POINT ( 'NONE',  ( -113.8446720159697065, -295.2466769315292936, -269.5906871005794301 ) ) ;
#64989 = CARTESIAN_POINT ( 'NONE',  ( -108.8338383194471248, -277.8204406134950091, -254.4203464208620744 ) ) ;
#64990 = CARTESIAN_POINT ( 'NONE',  ( -110.9763953039622493, -272.3420635680531063, -247.8752727268632725 ) ) ;
#64991 = CIRCLE ( 'NONE', #30139, 5.343514653206204557 ) ;
#64992 = CARTESIAN_POINT ( 'NONE',  ( -26.12075352961271335, -293.3865705447582855, -343.1951629649485653 ) ) ;
#64993 = CARTESIAN_POINT ( 'NONE',  ( 36.61569684423406557, -277.3641370944048958, -274.3451360666684877 ) ) ;
#64994 = CARTESIAN_POINT ( 'NONE',  ( -46.30481724080509309, -272.0768071443362146, -196.6690016424053908 ) ) ;
#64995 = CARTESIAN_POINT ( 'NONE',  ( 20.48630558546545544, -294.1233050671763181, -225.1406403916678869 ) ) ;
#64996 = CARTESIAN_POINT ( 'NONE',  ( -98.98580949401275575, -297.0839198735492346, -310.1306523387345919 ) ) ;
#64997 = CARTESIAN_POINT ( 'NONE',  ( -43.49969339204867680, -252.6666589713051394, -448.1074777562126314 ) ) ;
#64998 = CARTESIAN_POINT ( 'NONE',  ( -91.39672056065612082, -293.8190723162027211, -322.5921738032370172 ) ) ;
#64999 = VECTOR ( 'NONE', #69282, 1000.000000000000000 ) ;
#65000 = CARTESIAN_POINT ( 'NONE',  ( -68.14425835412929189, -298.3097102831461598, -199.8450762957822633 ) ) ;
#65001 = CARTESIAN_POINT ( 'NONE',  ( -93.53304422316939792, -275.2430403383432918, -220.6868439636174912 ) ) ;
#65002 = CARTESIAN_POINT ( 'NONE',  ( -110.5721908646213052, -291.4823795916028075, -271.1999706868085696 ) ) ;
#65003 = CARTESIAN_POINT ( 'NONE',  ( -15.58248214811220222, -295.0960941066388727, -340.1181356406543159 ) ) ;
#65004 = CARTESIAN_POINT ( 'NONE',  ( -97.28365527322517892, -281.1542781798481201, -224.6742512743268207 ) ) ;
#65005 = CARTESIAN_POINT ( 'NONE',  ( -35.33208881341227681, -278.7616817725262877, -193.8676121899182760 ) ) ;
#65006 = EDGE_CURVE ( 'NONE', #52785, #48386, #91206, .T. ) ;
#65007 = CARTESIAN_POINT ( 'NONE',  ( -67.84855252307130513, -282.7907836758585631, -340.9489692303662309 ) ) ;
#65008 = CARTESIAN_POINT ( 'NONE',  ( 35.63585796778031067, -274.5933015986652208, -245.9529804386882859 ) ) ;
#65009 = CARTESIAN_POINT ( 'NONE',  ( -102.7146785439990140, -277.4690871465581949, -231.1073970538200228 ) ) ;
#65010 = CARTESIAN_POINT ( 'NONE',  ( 20.57479640587767378, -278.8922418235802638, -222.4475723026494620 ) ) ;
#65011 = EDGE_CURVE ( 'NONE', #9610, #10831, #80607, .T. ) ;
#65012 = CARTESIAN_POINT ( 'NONE',  ( -55.39873258125298605, -296.4998840667466311, -199.0681103036263835 ) ) ;
#65013 = CARTESIAN_POINT ( 'NONE',  ( 9.701507942140940699, -276.6992781592539359, -211.8834195356988346 ) ) ;
#65014 = CARTESIAN_POINT ( 'NONE',  ( 201.2104617360081704, 15.00000000000000000, -10.00000000000000000 ) ) ;
#65015 = CARTESIAN_POINT ( 'NONE',  ( 23.50164100436456849, -290.9691743327213658, -225.9033330078058270 ) ) ;
#65016 = CARTESIAN_POINT ( 'NONE',  ( -89.49148258356979113, -289.7631774190076044, -327.0126862736960902 ) ) ;
#65017 = CARTESIAN_POINT ( 'NONE',  ( -8.420109569228346302, -276.4298878480741450, -200.9259816152268741 ) ) ;
#65018 = CARTESIAN_POINT ( 'NONE',  ( -40.57224733803614924, -296.0112990370118951, -195.5846799292339426 ) ) ;
#65019 = CARTESIAN_POINT ( 'NONE',  ( -76.01658475944793736, -284.7468072085644621, -203.9039765725950986 ) ) ;
#65020 = CARTESIAN_POINT ( 'NONE',  ( -112.3924214805754360, -282.5558719554007325, -270.0585568334979030 ) ) ;
#65021 = CARTESIAN_POINT ( 'NONE',  ( 197.0327713505838290, 40.95653769364759711, 12.25939981568760295 ) ) ;
#65022 = CARTESIAN_POINT ( 'NONE',  ( 23.67985290077372795, -291.7837456107552612, -229.5750839650057173 ) ) ;
#65023 = CARTESIAN_POINT ( 'NONE',  ( -75.33222439773294354, -283.6794072767269199, -206.5834922356388574 ) ) ;
#65024 = CARTESIAN_POINT ( 'NONE',  ( 154.1415209985679269, 20.37991841447902175, -11.45812909362557619 ) ) ;
#65025 = FACE_OUTER_BOUND ( 'NONE', #16719, .T. ) ;
#65026 = CARTESIAN_POINT ( 'NONE',  ( 26.56504906341792349, -291.0241908038734664, -231.0078170028048703 ) ) ;
#65027 = CARTESIAN_POINT ( 'NONE',  ( -95.75219581073891106, -282.3647043226262099, -319.4824796599507977 ) ) ;
#65028 = CARTESIAN_POINT ( 'NONE',  ( -93.32029419791268765, -279.4749640461055264, -318.4530863628002066 ) ) ;
#65029 = CARTESIAN_POINT ( 'NONE',  ( -40.81391583870370710, -287.2145928977079166, -193.7849995979883033 ) ) ;
#65030 = CARTESIAN_POINT ( 'NONE',  ( -7.016504831150768062, -286.4614861796586638, -203.9442095719910810 ) ) ;
#65031 = CARTESIAN_POINT ( 'NONE',  ( -95.72954365407453281, -279.3522802100104059, -315.1521287678070280 ) ) ;
#65032 = CARTESIAN_POINT ( 'NONE',  ( -110.1278571766150378, -279.4588069847839620, -262.4737467759662195 ) ) ;
#65033 = CARTESIAN_POINT ( 'NONE',  ( -112.3281035586150409, -286.5925953445448613, -267.2241425472863057 ) ) ;
#65034 = VERTEX_POINT ( 'NONE', #40686 ) ;
#65035 = CARTESIAN_POINT ( 'NONE',  ( -40.43813179861543006, -297.8476904058522337, -193.3712755926543707 ) ) ;
#65036 = CARTESIAN_POINT ( 'NONE',  ( 30.93962469985678965, -289.9304453970094642, -300.6474983243394377 ) ) ;
#65037 = LINE ( 'NONE', #21447, #4964 ) ;
#65038 = CARTESIAN_POINT ( 'NONE',  ( -55.56934967048406548, -279.7662352645559736, -350.3683826091709648 ) ) ;
#65039 = ORIENTED_EDGE ( 'NONE', *, *, #80951, .T. ) ;
#65040 = CARTESIAN_POINT ( 'NONE',  ( 33.69823470673961197, -292.3049112733814923, -297.9250087201768338 ) ) ;
#65041 = CARTESIAN_POINT ( 'NONE',  ( -4.300892196741418871, -288.0160145898828432, -204.4899348624456650 ) ) ;
#65042 = CARTESIAN_POINT ( 'NONE',  ( 34.31008639629446577, -283.5543844227261729, -288.9587766495695291 ) ) ;
#65043 = CARTESIAN_POINT ( 'NONE',  ( 33.30764423547869768, -288.6030906802274103, -241.1149580787556488 ) ) ;
#65044 = CARTESIAN_POINT ( 'NONE',  ( -4.529283412413871446, -289.9439969738307923, -339.4887728749631606 ) ) ;
#65045 = CARTESIAN_POINT ( 'NONE',  ( -111.3999709160549827, -286.7054854849619119, -258.4316797885995243 ) ) ;
#65046 = CARTESIAN_POINT ( 'NONE',  ( -114.2318936896619306, -278.6674214187959819, -274.4718525336907646 ) ) ;
#65047 = ORIENTED_EDGE ( 'NONE', *, *, #45328, .F. ) ;
#65048 = CARTESIAN_POINT ( 'NONE',  ( 37.38868045229116888, -291.7743100003077075, -281.5273356325625400 ) ) ;
#65049 = CARTESIAN_POINT ( 'NONE',  ( 36.60031376267445324, -281.1155184187628038, -248.8294644994108467 ) ) ;
#65050 = CARTESIAN_POINT ( 'NONE',  ( -88.19644433264322458, -275.1919163534752215, -216.2105846099405255 ) ) ;
#65051 = CARTESIAN_POINT ( 'NONE',  ( -83.63170945779077670, -373.0521521680024648, -413.1172536214571096 ) ) ;
#65052 = CARTESIAN_POINT ( 'NONE',  ( -69.91165696735023971, -294.1233781216987495, -202.8022627189028810 ) ) ;
#65053 = VECTOR ( 'NONE', #24115, 1000.000000000000000 ) ;
#65054 = CARTESIAN_POINT ( 'NONE',  ( -31.31774836845783838, -272.3670796898460367, -194.6004963957727227 ) ) ;
#65055 = DIRECTION ( 'NONE',  ( 0.000000000000000000, 0.000000000000000000, 1.000000000000000000 ) ) ;
#65056 = CARTESIAN_POINT ( 'NONE',  ( -9.217869101949890620, -279.9377085392704885, -202.9293853177581184 ) ) ;
#65057 = CARTESIAN_POINT ( 'NONE',  ( 32.18618075494870112, -276.3422755766988530, -238.0808119201695376 ) ) ;
#65058 = VECTOR ( 'NONE', #61564, 1000.000000000000000 ) ;
#65059 = CARTESIAN_POINT ( 'NONE',  ( -94.07940219535004189, -298.6366098499015038, -223.4777913896885764 ) ) ;
#65060 = CARTESIAN_POINT ( 'NONE',  ( -10.79468827121161212, -281.7731639034983004, -342.4458900911664614 ) ) ;
#65061 = CARTESIAN_POINT ( 'NONE',  ( -110.9833490451023295, -292.4086881721431723, -262.9529092179504346 ) ) ;
#65062 = CARTESIAN_POINT ( 'NONE',  ( -87.02563648856381917, -298.8954524125682610, -212.3758685898957594 ) ) ;
#65063 = EDGE_CURVE ( 'NONE', #20922, #15791, #90541, .T. ) ;
#65064 = CARTESIAN_POINT ( 'NONE',  ( -107.4160447862182224, -298.1555591537640453, -239.2848801264625536 ) ) ;
#65065 = EDGE_CURVE ( 'NONE', #24040, #21372, #46867, .T. ) ;
#65066 = CARTESIAN_POINT ( 'NONE',  ( -36.96127528485158109, -297.0475027567128450, -345.2062253746649390 ) ) ;
#65067 = CARTESIAN_POINT ( 'NONE',  ( -94.84683218277757533, -281.8891917127844522, -318.2483628126325357 ) ) ;
#65068 = CARTESIAN_POINT ( 'NONE',  ( -112.9033874417387722, -290.4036621701820877, -255.5895546998198142 ) ) ;
#65069 = CARTESIAN_POINT ( 'NONE',  ( -18.84009304870927082, -272.3114912752647570, -197.9919650025553324 ) ) ;
#65070 = CARTESIAN_POINT ( 'NONE',  ( -5.130836386093802659, -288.0692251549377261, -201.3038904441487205 ) ) ;
#65071 = CARTESIAN_POINT ( 'NONE',  ( -105.9953054164847543, -289.8157181324237399, -244.5090069921172358 ) ) ;
#65072 = CARTESIAN_POINT ( 'NONE',  ( 203.6388754965839496, 292.3982009288597510, -83.13072119195177834 ) ) ;
#65073 = EDGE_LOOP ( 'NONE', ( #59613, #35353, #49189, #78344 ) ) ;
#65074 = CARTESIAN_POINT ( 'NONE',  ( -108.9154855428094208, -289.4695772829470002, -243.4559990169177865 ) ) ;
#65075 = CARTESIAN_POINT ( 'NONE',  ( -15.84947658711131169, -288.4332023146716324, -340.2005736601225863 ) ) ;
#65076 = VERTEX_POINT ( 'NONE', #18469 ) ;
#65077 = CARTESIAN_POINT ( 'NONE',  ( -91.69365165870306100, -286.3789648975975979, -216.2560546872649354 ) ) ;
#65078 = CARTESIAN_POINT ( 'NONE',  ( -72.84857431343088763, -277.8696201891085025, -334.1826298475584736 ) ) ;
#65079 = CARTESIAN_POINT ( 'NONE',  ( 38.50878463611227431, -292.6146570230254724, -281.6835060179772654 ) ) ;
#65080 = CARTESIAN_POINT ( 'NONE',  ( -47.23502070177807610, -283.8261319082021714, -346.6201174148558266 ) ) ;
#65081 = CARTESIAN_POINT ( 'NONE',  ( -1.640176690575162910, -282.9253304198406909, -338.5604252799167284 ) ) ;
#65082 = CARTESIAN_POINT ( 'NONE',  ( 34.35419165398938190, -281.7019315727233106, -256.4465613549074874 ) ) ;
#65083 = CARTESIAN_POINT ( 'NONE',  ( -113.5232974181574832, -274.0039250406831002, -284.1871152304669863 ) ) ;
#65084 = CARTESIAN_POINT ( 'NONE',  ( -14.01029086911824173, -91.12319595120793281, -359.2282198501130210 ) ) ;
#65085 = CARTESIAN_POINT ( 'NONE',  ( 43.91850979000791000, 11.98664398100423334, -328.7862006914569406 ) ) ;
#65086 = CARTESIAN_POINT ( 'NONE',  ( -19.22176515920261508, -273.4883614712646249, -199.4264900984424003 ) ) ;
#65087 = CARTESIAN_POINT ( 'NONE',  ( -6.386002136165075171, -273.3889597544974208, -203.9083465094957148 ) ) ;
#65088 = CARTESIAN_POINT ( 'NONE',  ( -84.15273514929729970, -295.1837198053062821, -331.4877232771656281 ) ) ;
#65089 = CARTESIAN_POINT ( 'NONE',  ( 174.4399942972555664, 240.3132199972240812, -177.3433689288450239 ) ) ;
#65090 = CARTESIAN_POINT ( 'NONE',  ( -96.54373969401257227, -271.8920344201064268, -221.8802134396371741 ) ) ;
#65091 = CARTESIAN_POINT ( 'NONE',  ( -68.58868350556366522, -299.4975491971368342, -203.0085875688419605 ) ) ;
#65092 = CARTESIAN_POINT ( 'NONE',  ( 35.76323752387585131, -288.7684825108344739, -262.8171423497376509 ) ) ;
#65093 = VERTEX_POINT ( 'NONE', #75771 ) ;
#65094 = CARTESIAN_POINT ( 'NONE',  ( -92.51952278498072246, -296.7600104201015938, -323.7299112949729079 ) ) ;
#65095 = CARTESIAN_POINT ( 'NONE',  ( 13.17758103872245634, -287.2736378670214776, -217.5107354965741138 ) ) ;
#65096 = CARTESIAN_POINT ( 'NONE',  ( -2.684880912629829197, -273.4198537449718742, -201.9330432040923711 ) ) ;
#65097 = CARTESIAN_POINT ( 'NONE',  ( 32.08850876903645144, -294.7791104785487732, -303.4033397123219515 ) ) ;
#65098 = CARTESIAN_POINT ( 'NONE',  ( 11.16437903475552496, -294.8935698847126332, -330.1515266224271841 ) ) ;
#65099 = CARTESIAN_POINT ( 'NONE',  ( -110.3061898342085811, -290.6720034923824869, -273.9110735125584597 ) ) ;
#65100 = ORIENTED_EDGE ( 'NONE', *, *, #78211, .F. ) ;
#65101 = CARTESIAN_POINT ( 'NONE',  ( -100.0278427780952626, -275.0397281648495209, -228.0807042868414669 ) ) ;
#65102 = CARTESIAN_POINT ( 'NONE',  ( 37.83205994756009005, -274.1619325833966627, -255.6330999294527260 ) ) ;
#65103 = ORIENTED_EDGE ( 'NONE', *, *, #13330, .F. ) ;
#65104 = CARTESIAN_POINT ( 'NONE',  ( -106.2930175166307833, -277.6193899738753430, -304.6166555712545119 ) ) ;
#65105 = CARTESIAN_POINT ( 'NONE',  ( 19.62928128541905437, -273.2944252534488214, -223.4489906150918728 ) ) ;
#65106 = CARTESIAN_POINT ( 'NONE',  ( -87.55500195373751637, -274.4112975495216915, -216.8795211431189784 ) ) ;
#65107 = CARTESIAN_POINT ( 'NONE',  ( 34.85559791110665628, -276.3308703026121407, -258.0001815018592879 ) ) ;
#65108 = CARTESIAN_POINT ( 'NONE',  ( 22.81667247092959983, -276.6842207497820709, -223.9185696319567569 ) ) ;
#65109 = CARTESIAN_POINT ( 'NONE',  ( -12.43415599607835631, -274.7500484461702399, -341.5356077846250287 ) ) ;
#65110 = CARTESIAN_POINT ( 'NONE',  ( -98.81453139608339598, -296.6557307269824264, -310.0137088135516592 ) ) ;
#65111 = CARTESIAN_POINT ( 'NONE',  ( -18.08363902885875518, -293.3737114736645708, -341.3857756605856366 ) ) ;
#65112 = DIRECTION ( 'NONE',  ( 0.000000000000000000, 0.000000000000000000, -1.000000000000000000 ) ) ;
#65113 = CARTESIAN_POINT ( 'NONE',  ( -84.53413555049628769, -279.9145575383950586, -209.5285641413592543 ) ) ;
#65114 = CARTESIAN_POINT ( 'NONE',  ( 7.582063831993099967, -276.5864368085204887, -327.9655645340899355 ) ) ;
#65115 = CARTESIAN_POINT ( 'NONE',  ( -2.432881682194780737, -285.1889901072894986, -202.2680281996405540 ) ) ;
#65116 = CARTESIAN_POINT ( 'NONE',  ( -102.2791239241788190, -299.0580786976456693, -232.4013933698420544 ) ) ;
#65117 = FACE_OUTER_BOUND ( 'NONE', #37875, .T. ) ;
#65118 = CARTESIAN_POINT ( 'NONE',  ( 28.96059536483316776, -286.3326073100376448, -239.4320485042985069 ) ) ;
#65119 = CARTESIAN_POINT ( 'NONE',  ( -64.72866823324253005, -275.6544579564328501, -339.1754837789096655 ) ) ;
#65120 = CARTESIAN_POINT ( 'NONE',  ( -26.95615195961621069, -275.4922301760327628, -343.2138139198715407 ) ) ;
#65121 = CARTESIAN_POINT ( 'NONE',  ( 7.324271778399890742, -284.4439115841490207, -330.6739603698275118 ) ) ;
#65122 = CARTESIAN_POINT ( 'NONE',  ( -41.86581010639052636, -278.3154721361077009, -343.6312940505091547 ) ) ;
#65123 = CARTESIAN_POINT ( 'NONE',  ( 156.4947056272797852, 20.00000000000000000, 15.00000000000000000 ) ) ;
#65124 = CARTESIAN_POINT ( 'NONE',  ( 12.16920554484783068, -274.7763778477155938, -328.2844348155628040 ) ) ;
#65125 = AXIS2_PLACEMENT_3D ( 'NONE', #25279, #89650, #31461 ) ;
#65126 = CARTESIAN_POINT ( 'NONE',  ( 9.544111777519209028, -275.3681175020474257, -214.2090685116437498 ) ) ;
#65127 = CARTESIAN_POINT ( 'NONE',  ( -5.738539955507913959, -282.4668990882411777, -202.1609075887422193 ) ) ;
#65128 = DIRECTION ( 'NONE',  ( 0.000000000000000000, 0.000000000000000000, 1.000000000000000000 ) ) ;
#65129 = CARTESIAN_POINT ( 'NONE',  ( 36.42457180151981078, -289.6816367715828733, -286.7864351565069114 ) ) ;
#65130 = CARTESIAN_POINT ( 'NONE',  ( -3.883691926935517902, -290.4932518030722122, -203.2235449730465291 ) ) ;
#65131 = ADVANCED_FACE ( 'NONE', ( #19413 ), #42839, .F. ) ;
#65132 = DIRECTION ( 'NONE',  ( 0.000000000000000000, 1.000000000000000000, 0.000000000000000000 ) ) ;
#65133 = CARTESIAN_POINT ( 'NONE',  ( -89.58101486556216742, -271.9812776523679645, -218.6668487309374882 ) ) ;
#65134 = CARTESIAN_POINT ( 'NONE',  ( -77.91070366289109472, -289.6402465910668980, -208.1918214527433406 ) ) ;
#65135 = CARTESIAN_POINT ( 'NONE',  ( -26.16130516772507875, -127.9538472306148122, -363.7897947155308884 ) ) ;
#65136 = CARTESIAN_POINT ( 'NONE',  ( 194.7453183674699915, 20.99999999999998934, -15.62500000000000355 ) ) ;
#65137 = CARTESIAN_POINT ( 'NONE',  ( -26.26450177189316904, -287.3934725382138708, -345.8594850372799669 ) ) ;
#65138 = CARTESIAN_POINT ( 'NONE',  ( -112.5990238542928807, -282.6541898128947423, -281.2363657905976311 ) ) ;
#65139 = CARTESIAN_POINT ( 'NONE',  ( -32.08564707325928822, -284.4098255744436301, -343.7624042370968027 ) ) ;
#65140 = CARTESIAN_POINT ( 'NONE',  ( -94.40454644069204448, -284.7091484574964397, -316.1678678109452107 ) ) ;
#65141 = CARTESIAN_POINT ( 'NONE',  ( -112.7241150043125515, -292.5568186285869388, -268.4227295041262096 ) ) ;
#65142 = CARTESIAN_POINT ( 'NONE',  ( -34.10833172957043047, -274.4250556067377147, -193.4501979491883787 ) ) ;
#65143 = CARTESIAN_POINT ( 'NONE',  ( -84.28946036545470122, -287.7716662728972210, -329.6328064005700753 ) ) ;
#65144 = CARTESIAN_POINT ( 'NONE',  ( -5.284774995942194131, -276.6418342691904968, -340.3707855369228810 ) ) ;
#65145 = CARTESIAN_POINT ( 'NONE',  ( 33.35079023463672598, -295.2187334143389990, -246.2333469219663300 ) ) ;
#65146 = CARTESIAN_POINT ( 'NONE',  ( -48.18343439339133027, -283.1093320178187582, -435.6442049081568939 ) ) ;
#65147 = CARTESIAN_POINT ( 'NONE',  ( -37.30987171927208124, -297.5519495502701943, -345.3611179825600175 ) ) ;
#65148 = CARTESIAN_POINT ( 'NONE',  ( -64.25142883712764785, -282.0956160253958274, -338.7505175933482064 ) ) ;
#65149 = CARTESIAN_POINT ( 'NONE',  ( -64.00680458375488513, -277.7043532314712593, -200.2066226660132600 ) ) ;
#65150 = CARTESIAN_POINT ( 'NONE',  ( -30.55260384793811568, -296.5356852809806014, -194.1629249112967273 ) ) ;
#65151 = CARTESIAN_POINT ( 'NONE',  ( 35.80068761150581480, -274.9169883601151696, -271.5949533400335554 ) ) ;
#65152 = CARTESIAN_POINT ( 'NONE',  ( 17.23878343649675671, -294.3687364833986067, -220.7718707143359893 ) ) ;
#65153 = CARTESIAN_POINT ( 'NONE',  ( 21.17460470564320119, -293.8769766968659383, -226.3241957769065209 ) ) ;
#65154 = CARTESIAN_POINT ( 'NONE',  ( -22.32746989708762086, -293.6659271199785053, -195.3860566328398249 ) ) ;
#65155 = CARTESIAN_POINT ( 'NONE',  ( 38.36141589626591042, -294.7236355228316143, -258.9455975846146885 ) ) ;
#65156 = CARTESIAN_POINT ( 'NONE',  ( -105.9879126152182351, -296.0528879423655439, -295.3431607320734997 ) ) ;
#65157 = CARTESIAN_POINT ( 'NONE',  ( -59.24966273850005649, -291.3357502855076859, -342.1443089059626459 ) ) ;
#65158 = CARTESIAN_POINT ( 'NONE',  ( -93.43008208074299148, -283.9986009193834207, -323.1354793585153971 ) ) ;
#65159 = CARTESIAN_POINT ( 'NONE',  ( -75.78521302646608149, -271.6847189406719281, -205.0134351872038394 ) ) ;
#65160 = CARTESIAN_POINT ( 'NONE',  ( 26.35855866060897057, -286.8148656126384139, -227.0793037278084796 ) ) ;
#65161 = CARTESIAN_POINT ( 'NONE',  ( -98.99342632410547083, -279.9594347785156288, -312.4433168352484245 ) ) ;
#65162 = CARTESIAN_POINT ( 'NONE',  ( 4.870741441887367351, -285.6965666009664915, -210.4532670905252303 ) ) ;
#65163 = CARTESIAN_POINT ( 'NONE',  ( -83.94245381970371511, -287.6916727200556352, -329.1927813444013964 ) ) ;
#65164 = CARTESIAN_POINT ( 'NONE',  ( -113.1493912600846841, -276.6764366587346444, -271.5647438394866526 ) ) ;
#65165 = CARTESIAN_POINT ( 'NONE',  ( 193.6056169066500274, 279.7126221763799094, -126.0203154767880989 ) ) ;
#65166 = CARTESIAN_POINT ( 'NONE',  ( -104.1721159660569498, -283.6628130992014007, -299.8854123922799886 ) ) ;
#65167 = CARTESIAN_POINT ( 'NONE',  ( 22.22424236409775844, -283.4066006951380245, -318.5472345616836947 ) ) ;
#65168 = CARTESIAN_POINT ( 'NONE',  ( -8.333189791669957103, -287.7402746410861027, -341.4480244741359343 ) ) ;
#65169 = CARTESIAN_POINT ( 'NONE',  ( -112.5066536882135324, -279.9940931680806671, -282.8779135936555917 ) ) ;
#65170 = EDGE_CURVE ( 'NONE', #41385, #71100, #77178, .T. ) ;
#65171 = CARTESIAN_POINT ( 'NONE',  ( -51.20670599493102770, -278.5410160725589890, -345.6011331594845615 ) ) ;
#65172 = CARTESIAN_POINT ( 'NONE',  ( -83.43609499822072451, -279.2333319198467620, -213.6890966540365753 ) ) ;
#65173 = CARTESIAN_POINT ( 'NONE',  ( 1.446102869352315023, -276.5531448027190891, -206.5853142570784939 ) ) ;
#65174 = CARTESIAN_POINT ( 'NONE',  ( 36.70416314821815718, -293.2868168420667416, -249.1893879345943503 ) ) ;
#65175 = CARTESIAN_POINT ( 'NONE',  ( 15.22418897315582775, -286.3254863203099490, -323.3580434076228585 ) ) ;
#65176 =( BOUNDED_CURVE ( )  B_SPLINE_CURVE ( 3, ( #34491, #62926, #41078, #33534 ),
 .UNSPECIFIED., .F., .F. ) 
 B_SPLINE_CURVE_WITH_KNOTS ( ( 4, 4 ),
 ( 0.000000000000000000, 1.570796326794896336 ),
 .UNSPECIFIED. ) 
 CURVE ( )  GEOMETRIC_REPRESENTATION_ITEM ( )  RATIONAL_B_SPLINE_CURVE ( ( 1.000000000000000000, 0.8047378541243650485, 0.8047378541243650485, 1.000000000000000000 ) ) 
 REPRESENTATION_ITEM ( '' )  );
#65177 = CARTESIAN_POINT ( 'NONE',  ( -14.12974226088500806, -293.9482980068891607, -197.7271830719465413 ) ) ;
#65178 = CARTESIAN_POINT ( 'NONE',  ( -92.43201502191433860, -294.7849934341749076, -318.7272557142741789 ) ) ;
#65179 = CARTESIAN_POINT ( 'NONE',  ( 6.458736340335631709, -284.3719295228690953, -330.5511168226627774 ) ) ;
#65180 = CARTESIAN_POINT ( 'NONE',  ( -42.39542323054588024, -294.7843599771210847, -343.2071705152927734 ) ) ;
#65181 =( BOUNDED_SURFACE ( )  B_SPLINE_SURFACE ( 3, 2, ( 
 ( #10688, #83585, #60907 ),
 ( #69396, #39087, #25829 ),
 ( #4528, #19209, #47124 ),
 ( #47607, #17809, #91631 ) ),
 .UNSPECIFIED., .F., .F., .F. ) 
 B_SPLINE_SURFACE_WITH_KNOTS ( ( 4, 4 ),
 ( 3, 3 ),
 ( 0.000000000000000000, 0.0009300155619514785879 ),
 ( 0.000000000000000000, 1.000000000000000000 ),
 .UNSPECIFIED. ) 
 GEOMETRIC_REPRESENTATION_ITEM ( )  RATIONAL_B_SPLINE_SURFACE ( (
 ( 1.000000000000000000, 0.8255171224912133399, 1.000000000000000000),
 ( 1.000000000000000000, 0.8158797882023690606, 1.000000000000000000),
 ( 1.000000000000000000, 0.8010468905540648610, 1.000000000000000000),
 ( 1.000000000000000000, 0.7827533893365004047, 1.000000000000000000) ) ) 
 REPRESENTATION_ITEM ( '' )  SURFACE ( )  );
#65182 = CARTESIAN_POINT ( 'NONE',  ( -90.58128421845070477, -292.3990351916302188, -215.0874091386716884 ) ) ;
#65183 = CARTESIAN_POINT ( 'NONE',  ( 33.55240461913435723, -281.9679774520059823, -252.4800128018499095 ) ) ;
#65184 = CARTESIAN_POINT ( 'NONE',  ( -14.90865016549609123, -297.2471622246442848, -193.6742277851535334 ) ) ;
#65185 = CARTESIAN_POINT ( 'NONE',  ( -98.94249613682718802, -290.5901195295340358, -316.4117367138375130 ) ) ;
#65186 = CARTESIAN_POINT ( 'NONE',  ( -94.42004502758976514, -282.0069648683203241, -320.1844862526012889 ) ) ;
#65187 = CARTESIAN_POINT ( 'NONE',  ( -103.1999545804094822, -291.4069023456658556, -230.4031657631257985 ) ) ;
#65188 = CARTESIAN_POINT ( 'NONE',  ( -12.01862849265304689, -286.7243167846764322, -201.8714871636321107 ) ) ;
#65189 = DIRECTION ( 'NONE',  ( 1.124465274301078034E-16, 1.000000000000000000, 0.000000000000000000 ) ) ;
#65190 = CARTESIAN_POINT ( 'NONE',  ( -104.7172394706867067, -254.0594188280566073, -325.1787590629403439 ) ) ;
#65191 = CARTESIAN_POINT ( 'NONE',  ( -30.80187348468898278, -124.8376641225716810, -360.4214517073238540 ) ) ;
#65192 = AXIS2_PLACEMENT_3D ( 'NONE', #35687, #86783, #80605 ) ;
#65193 = CARTESIAN_POINT ( 'NONE',  ( -107.3787478736263381, -278.0287493317208600, -249.2089627681827722 ) ) ;
#65194 = CARTESIAN_POINT ( 'NONE',  ( -49.17833494354143653, -278.8180749322415295, -198.0138986226862130 ) ) ;
#65195 = CARTESIAN_POINT ( 'NONE',  ( 29.93112004619106159, -274.7324711801586545, -232.8334263006657352 ) ) ;
#65196 = CARTESIAN_POINT ( 'NONE',  ( -87.43311609469282075, -230.8234426471767335, -345.6592249140303466 ) ) ;
#65197 = CARTESIAN_POINT ( 'NONE',  ( -84.19123524391571323, -277.9972466238668858, -209.9308771834095069 ) ) ;
#65198 = CARTESIAN_POINT ( 'NONE',  ( -74.64004911659841923, -281.5707601945397300, -335.0782071112436711 ) ) ;
#65199 = CARTESIAN_POINT ( 'NONE',  ( -108.9041640195071921, -298.6390941300284112, -244.8114061582887473 ) ) ;
#65200 = CARTESIAN_POINT ( 'NONE',  ( -91.72315337734127638, -291.7423674553141382, -221.5505395597147924 ) ) ;
#65201 = CARTESIAN_POINT ( 'NONE',  ( 23.14632853441941762, -286.8147105643434998, -312.1258601944918496 ) ) ;
#65202 = CARTESIAN_POINT ( 'NONE',  ( -60.84786326694463554, -274.4064754819924019, -197.0882588120444723 ) ) ;
#65203 = CARTESIAN_POINT ( 'NONE',  ( -68.04945934711490452, -297.8040878391975070, -204.1203174720320419 ) ) ;
#65204 = EDGE_LOOP ( 'NONE', ( #65909, #19637, #61125 ) ) ;
#65205 = FACE_BOUND ( 'NONE', #64644, .T. ) ;
#65206 = CARTESIAN_POINT ( 'NONE',  ( -112.9376460530305479, -280.4923435262941211, -268.7890723547576499 ) ) ;
#65207 = CARTESIAN_POINT ( 'NONE',  ( 17.28400562998450241, -281.9352794054693163, -221.4708495797858632 ) ) ;
#65208 = CARTESIAN_POINT ( 'NONE',  ( 14.45399818341865839, -282.5284725036201507, -214.6908314395851107 ) ) ;
#65209 = CARTESIAN_POINT ( 'NONE',  ( -4.733128820885818655, -281.6704210381087705, -335.9361858527531126 ) ) ;
#65210 = CARTESIAN_POINT ( 'NONE',  ( -94.30205790202462879, -271.6883720718137738, -223.5843032265325405 ) ) ;
#65211 = CARTESIAN_POINT ( 'NONE',  ( 208.9602656640649627, 27.80679762345980421, 14.02415587114433393 ) ) ;
#65212 = FACE_OUTER_BOUND ( 'NONE', #18360, .T. ) ;
#65213 = CARTESIAN_POINT ( 'NONE',  ( 36.34153287223616502, -276.6294867409338849, -292.2006793715371487 ) ) ;
#65214 = CYLINDRICAL_SURFACE ( 'NONE', #5117, 0.5000000000000004441 ) ;
#65215 = CARTESIAN_POINT ( 'NONE',  ( 21.09904473890400567, -278.1992681471870128, -317.3886747927066381 ) ) ;
#65216 = ORIENTED_EDGE ( 'NONE', *, *, #45526, .F. ) ;
#65217 = CARTESIAN_POINT ( 'NONE',  ( 219.8344101925596021, 3.000000000000000000, 10.00000000000000000 ) ) ;
#65218 = CARTESIAN_POINT ( 'NONE',  ( -112.1889198146302817, -286.6436728857402727, -261.6261018402218497 ) ) ;
#65219 = CARTESIAN_POINT ( 'NONE',  ( 11.04524603365648971, -291.9392154306532916, -215.4181474100658988 ) ) ;
#65220 = CARTESIAN_POINT ( 'NONE',  ( 31.33448909104350477, -286.4549800450564021, -235.7649647193582894 ) ) ;
#65221 = CARTESIAN_POINT ( 'NONE',  ( -99.89936526694434349, -282.2517912348295113, -310.0110284162740868 ) ) ;
#65223 = CARTESIAN_POINT ( 'NONE',  ( -6.396000258704246377, -284.5416427496026586, -202.6442533920717040 ) ) ;
#65222 = CARTESIAN_POINT ( 'NONE',  ( -37.56035519588864702, -281.6297034834774990, -343.9625541587451494 ) ) ;
#65224 = CARTESIAN_POINT ( 'NONE',  ( 18.80798210020796546, -283.4252345427393607, -317.6494779816167693 ) ) ;
#65225 = CARTESIAN_POINT ( 'NONE',  ( 6.097897530510628883, -272.6409561375065778, -209.1581660333129946 ) ) ;
#65226 = CARTESIAN_POINT ( 'NONE',  ( -96.56366273370623787, -282.3019913221716592, -318.3315984847617983 ) ) ;
#65227 = CARTESIAN_POINT ( 'NONE',  ( -96.67617012817308364, -297.9236062913669230, -316.2350901513532335 ) ) ;
#65228 = CARTESIAN_POINT ( 'NONE',  ( -38.72497260189452817, -281.0693086095133708, -345.5150599128980957 ) ) ;
#65229 = CARTESIAN_POINT ( 'NONE',  ( -101.0222944009613713, -279.9871631521448876, -234.1922036964794529 ) ) ;
#65230 = CARTESIAN_POINT ( 'NONE',  ( -4.318342954073128404, -288.4865236154905688, -202.8229703995945385 ) ) ;
#65231 = CARTESIAN_POINT ( 'NONE',  ( -113.5000000000000568, -190.7866584945343504, -447.4016117689005796 ) ) ;
#65232 = CARTESIAN_POINT ( 'NONE',  ( 139.6925840978351516, 15.36528803885690664, 22.50000000000000000 ) ) ;
#65233 = CARTESIAN_POINT ( 'NONE',  ( 29.61140071008724917, -295.0105238006773334, -235.2257490199197889 ) ) ;
#65234 = CARTESIAN_POINT ( 'NONE',  ( -43.39317789852498919, -275.1284415250990492, -345.1165877877641037 ) ) ;
#65235 = CARTESIAN_POINT ( 'NONE',  ( -95.34314436489886191, -289.0666914581544233, -320.7594442174558367 ) ) ;
#65236 = CARTESIAN_POINT ( 'NONE',  ( -6.448379707811984218, -293.0393336729117664, -337.3838243644204908 ) ) ;
#65237 = CARTESIAN_POINT ( 'NONE',  ( -102.3005725409951623, -276.7719005310091802, -304.7353579236955738 ) ) ;
#65238 = CARTESIAN_POINT ( 'NONE',  ( -63.49278125137783491, -295.8474215252201134, -200.8302244428391532 ) ) ;
#65239 = CARTESIAN_POINT ( 'NONE',  ( -88.28441468808671289, -292.6359381462440865, -217.3182943505541118 ) ) ;
#65240 = CARTESIAN_POINT ( 'NONE',  ( 31.98288692825981272, -278.4805209788416960, -303.7098442033570223 ) ) ;
#65241 = CARTESIAN_POINT ( 'NONE',  ( -37.70528027253799053, -293.5364763835182202, -346.6798812815856650 ) ) ;
#65242 = CARTESIAN_POINT ( 'NONE',  ( -95.56931727681921984, -291.5201046115790291, -315.7244980839562345 ) ) ;
#65243 = CARTESIAN_POINT ( 'NONE',  ( -102.3373091727066679, -289.3138171906371667, -230.8954603941162986 ) ) ;
#65244 = CARTESIAN_POINT ( 'NONE',  ( 32.88132104499118213, -289.2686986845671981, -292.5331746625878964 ) ) ;
#65245 = DIRECTION ( 'NONE',  ( 1.000000000000000000, 0.000000000000000000, 0.000000000000000000 ) ) ;
#65246 = CARTESIAN_POINT ( 'NONE',  ( -74.78979084820221601, -290.3672994908432088, -333.2267886346736532 ) ) ;
#65247 = DIRECTION ( 'NONE',  ( 0.000000000000000000, 1.000000000000000000, 0.000000000000000000 ) ) ;
#65248 = CARTESIAN_POINT ( 'NONE',  ( 9.994689702989733249, -289.6217089147236265, -330.6554725855314132 ) ) ;
#65249 = CARTESIAN_POINT ( 'NONE',  ( -36.73981503967894469, -278.0797941285628667, -194.9955501459691902 ) ) ;
#65250 = CARTESIAN_POINT ( 'NONE',  ( -99.41333535821576106, -279.4904923352523838, -224.8102370885552546 ) ) ;
#65251 = VECTOR ( 'NONE', #31144, 1000.000000000000000 ) ;
#65252 = CARTESIAN_POINT ( 'NONE',  ( -8.050863683924232461, -282.3456749241018429, -341.6060604817206467 ) ) ;
#65253 = CARTESIAN_POINT ( 'NONE',  ( 18.39350502213383720, -284.8524379805000990, -220.1564059311868391 ) ) ;
#65254 = DIRECTION ( 'NONE',  ( -0.5379402104274313423, 0.8429829950866690735, 0.000000000000000000 ) ) ;
#65255 = CARTESIAN_POINT ( 'NONE',  ( 30.10467596667838208, -279.2788590299093130, -239.2241039801153022 ) ) ;
#65256 = CARTESIAN_POINT ( 'NONE',  ( -77.43133059580873123, -283.5141286244143544, -206.9748246967708951 ) ) ;
#65257 = CYLINDRICAL_SURFACE ( 'NONE', #51747, 0.5000000000000004441 ) ;
#65258 = CARTESIAN_POINT ( 'NONE',  ( -110.0123771794569620, -276.7348115156170252, -293.8054116256126349 ) ) ;
#65259 = CARTESIAN_POINT ( 'NONE',  ( -78.34553825622769807, -284.4344693475500776, -205.5523395024503372 ) ) ;
#65260 = CARTESIAN_POINT ( 'NONE',  ( -48.91102973045033053, -274.7039797872561167, -198.0688979670926528 ) ) ;
#65261 = CARTESIAN_POINT ( 'NONE',  ( -94.92781295653404072, -292.7976773254404748, -224.1860736833043859 ) ) ;
#65262 = CARTESIAN_POINT ( 'NONE',  ( -96.49158625621031149, -274.6320366496418046, -221.9682102769503445 ) ) ;
#65263 = CARTESIAN_POINT ( 'NONE',  ( 32.08324031743266858, -274.9166887491608691, -247.5651547900818059 ) ) ;
#65264 = CARTESIAN_POINT ( 'NONE',  ( -89.88532584151985816, -297.7936146557994448, -323.9520009522315149 ) ) ;
#65265 = CARTESIAN_POINT ( 'NONE',  ( -48.86690013912242847, -289.3616203337568322, -346.5476423584430563 ) ) ;
#65266 = CARTESIAN_POINT ( 'NONE',  ( 34.23693760936082953, -279.9445444868468371, -294.7271313253883136 ) ) ;
#65267 = CARTESIAN_POINT ( 'NONE',  ( 34.46359639662605190, -293.0316000634022089, -242.4108932434071164 ) ) ;
#65268 = EDGE_CURVE ( 'NONE', #12757, #88799, #39313, .T. ) ;
#65269 = CARTESIAN_POINT ( 'NONE',  ( -28.06469952927296418, -291.2313997091950455, -197.6648636932714282 ) ) ;
#65270 = CARTESIAN_POINT ( 'NONE',  ( -68.71512544582297721, -293.4643346632063867, -338.4979271635406803 ) ) ;
#65271 = ORIENTED_EDGE ( 'NONE', *, *, #66484, .T. ) ;
#65272 = CARTESIAN_POINT ( 'NONE',  ( -22.78264641048746597, -118.9815703160634541, -21.50000000000000000 ) ) ;
#65273 = CARTESIAN_POINT ( 'NONE',  ( -87.96871709012607710, -290.8287080751878193, -217.6139481118029266 ) ) ;
#65274 = DIRECTION ( 'NONE',  ( -1.000000000000000000, 0.000000000000000000, 0.000000000000000000 ) ) ;
#65275 = CARTESIAN_POINT ( 'NONE',  ( -85.37503908990142065, -286.3477934072787434, -210.4810832426212244 ) ) ;
#65276 = CARTESIAN_POINT ( 'NONE',  ( -67.68488546085839630, -277.1237833571632905, -207.2794874003663779 ) ) ;
#65277 = CARTESIAN_POINT ( 'NONE',  ( -8.487635440209615467, -293.7424562988702519, -341.5529492560272615 ) ) ;
#65278 = CARTESIAN_POINT ( 'NONE',  ( -110.6307208814372416, -285.5895087055593535, -292.3614778708202380 ) ) ;
#65279 = CARTESIAN_POINT ( 'NONE',  ( -108.0937498912920205, -284.1482066015774990, -288.3374206845554681 ) ) ;
#65280 = CARTESIAN_POINT ( 'NONE',  ( -10.98818745746989123, -278.2223672120250626, -339.1811740889316980 ) ) ;
#65281 = CARTESIAN_POINT ( 'NONE',  ( -17.81395034317745996, -292.8191808624181931, -342.4063384220154944 ) ) ;
#65282 = CARTESIAN_POINT ( 'NONE',  ( 28.06391368486297111, -295.7790183553920542, -305.1128627020493127 ) ) ;
#65283 = CARTESIAN_POINT ( 'NONE',  ( 33.62220002145524234, -274.5932161043384667, -289.1029263621664995 ) ) ;
#65284 = EDGE_LOOP ( 'NONE', ( #78236, #91934, #23000, #61976, #37561, #89102, #80768, #92166, #63203, #28283, #76542 ) ) ;
#65285 = DIRECTION ( 'NONE',  ( 0.6056179655966478226, -0.7957555401921982963, -0.000000000000000000 ) ) ;
#65286 = CARTESIAN_POINT ( 'NONE',  ( 17.54349167034347801, -293.9607932386921334, -324.4124800443496497 ) ) ;
#65287 = CARTESIAN_POINT ( 'NONE',  ( 35.10812308401312265, -289.6935031966906990, -287.4589926538305349 ) ) ;
#65288 = CARTESIAN_POINT ( 'NONE',  ( -62.87401853368009341, -295.7197317415770499, -199.7869639662973782 ) ) ;
#65289 = CARTESIAN_POINT ( 'NONE',  ( -90.48791314293045218, -296.8629919621058093, -325.7241135776966416 ) ) ;
#65290 = EDGE_CURVE ( 'NONE', #69004, #49537, #47205, .T. ) ;
#65291 = CARTESIAN_POINT ( 'NONE',  ( -6.981729361334126693, -287.1127940008456108, -203.8480131727205276 ) ) ;
#65292 = CARTESIAN_POINT ( 'NONE',  ( -113.9752608163959877, -277.6671682581188634, -265.8758544900713332 ) ) ;
#65293 = CARTESIAN_POINT ( 'NONE',  ( -39.09718666489686711, -295.7250506077480736, -347.2391451034936836 ) ) ;
#65294 = CARTESIAN_POINT ( 'NONE',  ( -4.884056993510368372, -286.7689211001621175, -338.8356203455598461 ) ) ;
#65295 = CARTESIAN_POINT ( 'NONE',  ( -34.85107514289681774, -295.3549434226244443, -347.2996718991996659 ) ) ;
#65296 = CARTESIAN_POINT ( 'NONE',  ( -103.5772793547167510, -291.3002529119239057, -239.6213142878302165 ) ) ;
#65297 = FACE_OUTER_BOUND ( 'NONE', #59295, .T. ) ;
#65298 = CARTESIAN_POINT ( 'NONE',  ( -23.68628624284178130, -43.55766379199612004, 21.50000000000000000 ) ) ;
#65299 = CARTESIAN_POINT ( 'NONE',  ( 139.3042675124528103, 178.0593506815302192, -238.4361927325643080 ) ) ;
#65300 = CARTESIAN_POINT ( 'NONE',  ( 34.19743212384639719, -288.7335508957171442, -243.8119125668313529 ) ) ;
#65301 = CARTESIAN_POINT ( 'NONE',  ( 44.71564893372296723, -291.0523547857347353, -270.3937649182068412 ) ) ;
#65302 = EDGE_LOOP ( 'NONE', ( #46725, #69362, #11057, #26408 ) ) ;
#65303 = CARTESIAN_POINT ( 'NONE',  ( -88.85700406090930414, -278.6992749847294135, -213.2692074608133339 ) ) ;
#65304 = CARTESIAN_POINT ( 'NONE',  ( -3.987709938743091875, -284.6113574507634212, -337.3502198503776413 ) ) ;
#65305 = CARTESIAN_POINT ( 'NONE',  ( -109.4154064952325740, -283.4494917522649189, -244.9842162286564644 ) ) ;
#65306 = CARTESIAN_POINT ( 'NONE',  ( 26.92719267051030840, -286.1388005868269602, -308.0238995172038017 ) ) ;
#65307 = CARTESIAN_POINT ( 'NONE',  ( 37.51911326793244683, -277.5650742851277641, -282.3599795284450806 ) ) ;
#65308 = CARTESIAN_POINT ( 'NONE',  ( -110.3027966657351868, -296.9940245040288005, -274.1908481967466855 ) ) ;
#65309 = EDGE_CURVE ( 'NONE', #34178, #87468, #90148, .T. ) ;
#65310 = EDGE_LOOP ( 'NONE', ( #77485, #62885, #47889, #81880 ) ) ;
#65311 = CARTESIAN_POINT ( 'NONE',  ( -35.65598151951728312, -293.7154211559209216, -343.8475160310974275 ) ) ;
#65312 = CARTESIAN_POINT ( 'NONE',  ( -33.92810822136723203, -280.7454502061456196, -193.5388544315613899 ) ) ;
#65314 = CARTESIAN_POINT ( 'NONE',  ( -70.98120153764955376, -278.9445994371603206, -205.4449574988954907 ) ) ;
#65313 = CARTESIAN_POINT ( 'NONE',  ( -72.84200492444578856, -277.5363928325469374, -334.1620842169902517 ) ) ;
#65315 = CARTESIAN_POINT ( 'NONE',  ( 25.06731933576267579, -276.0387618071033557, -225.7672903536730189 ) ) ;
#65316 = CARTESIAN_POINT ( 'NONE',  ( -72.71040477222277332, -276.4297021520570752, -338.4238882509869768 ) ) ;
#65317 = CARTESIAN_POINT ( 'NONE',  ( 165.9745577554829197, 231.6962457589320081, -190.8271905442535967 ) ) ;
#65318 = CARTESIAN_POINT ( 'NONE',  ( -83.81235696716545647, -297.1010307119714753, -331.0832728325123639 ) ) ;
#65319 = CARTESIAN_POINT ( 'NONE',  ( -54.42813229853333468, -279.7662352645560304, -345.3683826091709648 ) ) ;
#65320 = TOROIDAL_SURFACE ( 'NONE', #10851, 4.499999999999990230, 0.5000000000000000000 ) ;
#65321 = CARTESIAN_POINT ( 'NONE',  ( 133.0872704186301405, -299.5541904835127980, -189.7068768330456123 ) ) ;
#65322 = MECHANICAL_DESIGN_GEOMETRIC_PRESENTATION_REPRESENTATION (  '', ( #53240 ), #13939 ) ;
#65323 = CARTESIAN_POINT ( 'NONE',  ( -103.7713686059891103, -286.0501616071703097, -239.2354874074904103 ) ) ;
#65324 = CARTESIAN_POINT ( 'NONE',  ( -66.81695248463182679, -287.4313318652025373, -200.3241026729481575 ) ) ;
#65325 = CARTESIAN_POINT ( 'NONE',  ( 25.77988533533015669, -287.4073371202152885, -307.3333584263721150 ) ) ;
#65326 = CARTESIAN_POINT ( 'NONE',  ( 13.63532040421435809, -281.8683679172942220, -328.0590206876794923 ) ) ;
#65327 = EDGE_CURVE ( 'NONE', #60755, #78077, #9562, .T. ) ;
#65328 = CARTESIAN_POINT ( 'NONE',  ( -108.3829322212403241, -277.2139407260935400, -250.3247359912301704 ) ) ;
#65329 = CARTESIAN_POINT ( 'NONE',  ( -107.3304754579055640, -286.0869041655930687, -295.2615113610546587 ) ) ;
#65330 = CARTESIAN_POINT ( 'NONE',  ( -79.43519188038939660, -277.9519408077896969, -209.8727248557343898 ) ) ;
#65331 = CARTESIAN_POINT ( 'NONE',  ( -29.64523733348267953, -278.2679838115481630, -343.5014096827242156 ) ) ;
#65332 = CARTESIAN_POINT ( 'NONE',  ( 32.95878180429987481, -276.3078446760085285, -290.3024096635724618 ) ) ;
#65333 = CARTESIAN_POINT ( 'NONE',  ( -15.08237165917536515, -287.5651763040362425, -343.7141293351393756 ) ) ;
#65334 = AXIS2_PLACEMENT_3D ( 'NONE', #29238, #50544, #78502 ) ;
#65335 = CARTESIAN_POINT ( 'NONE',  ( -93.30690372224447060, -284.6346508238265756, -323.0307112219816759 ) ) ;
#65336 = CARTESIAN_POINT ( 'NONE',  ( 6.894755563222777717, -282.9605139220510637, -333.3759554415153730 ) ) ;
#65337 = ORIENTED_EDGE ( 'NONE', *, *, #12869, .T. ) ;
#65338 = EDGE_LOOP ( 'NONE', ( #50110, #12265, #21040 ) ) ;
#65339 = DIRECTION ( 'NONE',  ( -0.000000000000000000, -0.000000000000000000, 1.000000000000000000 ) ) ;
#65340 = CARTESIAN_POINT ( 'NONE',  ( 9.483457504974088792, -290.2769436734733404, -329.9905349023028975 ) ) ;
#65341 = CARTESIAN_POINT ( 'NONE',  ( -112.0871577655630631, -289.0315367282999546, -286.6833371162832123 ) ) ;
#65342 = CARTESIAN_POINT ( 'NONE',  ( -109.3588762503709688, -271.7893684176930833, -256.7884039423370268 ) ) ;
#65343 = CARTESIAN_POINT ( 'NONE',  ( 24.73707529807938954, -292.2974386107674718, -224.9789802143407940 ) ) ;
#65344 = CARTESIAN_POINT ( 'NONE',  ( -109.6225427432049884, -288.8435428208294411, -284.7849789324421295 ) ) ;
#65345 = CARTESIAN_POINT ( 'NONE',  ( 33.40795021036746704, -288.5004923088713440, -250.8260857948762066 ) ) ;
#65346 = CARTESIAN_POINT ( 'NONE',  ( 39.58706461736021254, -290.0519495502703080, -270.3284710469133074 ) ) ;
#65347 = CARTESIAN_POINT ( 'NONE',  ( 36.15364725900674614, -289.7442375073393350, -285.3088457246223584 ) ) ;
#65348 = CARTESIAN_POINT ( 'NONE',  ( -97.71646255462998454, -289.1620496503210802, -225.5632716339396495 ) ) ;
#65349 = CARTESIAN_POINT ( 'NONE',  ( -105.5938252097688661, -292.9617544598418704, -239.1466366034793793 ) ) ;
#65350 = CARTESIAN_POINT ( 'NONE',  ( -100.5983573168092704, -284.9885127014148338, -307.2664532196525897 ) ) ;
#65351 = CARTESIAN_POINT ( 'NONE',  ( 37.40023289792614491, -295.4439952151730608, -261.9062163768480787 ) ) ;
#65352 = CARTESIAN_POINT ( 'NONE',  ( 139.1539576904058606, 250.0000000000000568, -10.49999999999999822 ) ) ;
#65353 = CARTESIAN_POINT ( 'NONE',  ( 164.6329196456214277, 214.9910457053126720, 23.09031830825856346 ) ) ;
#65354 = CARTESIAN_POINT ( 'NONE',  ( -75.61943636027299931, -275.5244075809591777, -205.3914795370817785 ) ) ;
#65355 = CARTESIAN_POINT ( 'NONE',  ( -18.70434817123013360, -282.0032343908314942, -341.1614331494340036 ) ) ;
#65356 = CARTESIAN_POINT ( 'NONE',  ( -109.3182940398453411, -282.2800102402512721, -291.4871252058547952 ) ) ;
#65357 = CARTESIAN_POINT ( 'NONE',  ( -114.1763943722265680, -295.7589359101915534, -269.5939280421946478 ) ) ;
#65358 = CARTESIAN_POINT ( 'NONE',  ( 27.53542775735564518, -273.3108473875230402, -234.6321674303209477 ) ) ;
#65359 = CARTESIAN_POINT ( 'NONE',  ( -104.6618806824832575, -277.0543968831531174, -238.4704458353679399 ) ) ;
#65360 = CARTESIAN_POINT ( 'NONE',  ( -37.84257380046856412, -299.3609248413384307, -196.8696721863768744 ) ) ;
#65361 = CARTESIAN_POINT ( 'NONE',  ( -41.14513951141092463, -272.5800319411375199, -193.9932032119276926 ) ) ;
#65362 = CARTESIAN_POINT ( 'NONE',  ( -36.97452510621791077, -296.4727076717618388, -343.9619577581739236 ) ) ;
#65363 = CARTESIAN_POINT ( 'NONE',  ( 82.64890176555634582, -299.5541904835127980, -197.2570935515975918 ) ) ;
#65364 = CARTESIAN_POINT ( 'NONE',  ( 8.336942482371544116, -295.2116025256293028, -327.5757169327271185 ) ) ;
#65365 = CARTESIAN_POINT ( 'NONE',  ( 202.8019728163925492, 61.40723988820080592, 6.999999999999999112 ) ) ;
#65367 = CARTESIAN_POINT ( 'NONE',  ( -90.40723577949991352, -295.8293950681012348, -320.5642352078342583 ) ) ;
#65366 = CARTESIAN_POINT ( 'NONE',  ( -112.5681479059690986, -282.5055862939886993, -275.5782373613286609 ) ) ;
#65368 = CARTESIAN_POINT ( 'NONE',  ( -112.5250916142391588, -284.3442083940905718, -286.9881334886314335 ) ) ;
#65369 = CARTESIAN_POINT ( 'NONE',  ( 36.76290506810964587, -287.4806353782450401, -291.2481577722910515 ) ) ;
#65370 = CARTESIAN_POINT ( 'NONE',  ( 3.255966963356850208, -290.5984256847651181, -207.4359178264753893 ) ) ;
#65371 = CARTESIAN_POINT ( 'NONE',  ( -88.81568146028622834, -278.5478799972228217, -213.3121209197132941 ) ) ;
#65372 = CARTESIAN_POINT ( 'NONE',  ( -110.4683760289727132, -281.8380690714489560, -287.0191576251351080 ) ) ;
#65373 = DIRECTION ( 'NONE',  ( 1.000000000000000000, 0.000000000000000000, 5.880589007913310608E-16 ) ) ;
#65374 = CARTESIAN_POINT ( 'NONE',  ( 28.01868723161029706, -285.8945006358876526, -236.8551474084490280 ) ) ;
#65376 = CARTESIAN_POINT ( 'NONE',  ( 185.4166944662832179, 250.0000000000000568, 23.37680765314684095 ) ) ;
#65375 = CARTESIAN_POINT ( 'NONE',  ( -57.22407212948342448, -288.2230547760084391, -344.4847823251547538 ) ) ;
#65377 = CARTESIAN_POINT ( 'NONE',  ( 169.7306087885279453, 275.0000000000000568, -24.89999999999999147 ) ) ;
#65378 = CARTESIAN_POINT ( 'NONE',  ( -107.4733429672123890, -298.4558471392887782, -247.2208665155737890 ) ) ;
#65379 = CARTESIAN_POINT ( 'NONE',  ( -84.21986526421866870, -280.8473325187399041, -209.9530847315107849 ) ) ;
#65381 = CARTESIAN_POINT ( 'NONE',  ( 33.34290817062729673, -281.4613005348429056, -288.7350392704406659 ) ) ;
#65380 = CARTESIAN_POINT ( 'NONE',  ( -112.6644134575226133, -294.6179247553872642, -266.7875873619102549 ) ) ;
#65382 = CARTESIAN_POINT ( 'NONE',  ( 26.51292985971861782, -294.2857643577708586, -313.3911799582067488 ) ) ;
#65383 = CARTESIAN_POINT ( 'NONE',  ( -64.05444240837543646, -281.7040289382188121, -200.2247446144436367 ) ) ;
#65384 = ADVANCED_FACE ( 'NONE', ( #93706 ), #36826, .T. ) ;
#65385 = CARTESIAN_POINT ( 'NONE',  ( -107.8325320897626227, -295.3492011492169809, -290.2219099575742121 ) ) ;
#65386 = AXIS2_PLACEMENT_3D ( 'NONE', #46076, #2074, #67874 ) ;
#65387 = EDGE_LOOP ( 'NONE', ( #90983, #6722, #3922, #54974 ) ) ;
#65388 = DIRECTION ( 'NONE',  ( 1.000000000000000000, 0.000000000000000000, -0.000000000000000000 ) ) ;
#65389 = CARTESIAN_POINT ( 'NONE',  ( -4.071915125946985903, -284.5910924343277770, -337.1815356145591522 ) ) ;
#65390 = CARTESIAN_POINT ( 'NONE',  ( 82.17440492340898572, -297.5479941798179766, -195.4018648718562758 ) ) ;
#65391 = CARTESIAN_POINT ( 'NONE',  ( -95.95921662488163406, -282.6952119285918457, -223.5744983911110353 ) ) ;
#65392 = CARTESIAN_POINT ( 'NONE',  ( -5.172536408195755442, -273.6620643650621219, -200.5807215467368394 ) ) ;
#65393 = CARTESIAN_POINT ( 'NONE',  ( -101.1226439263710546, -290.8722681356970270, -234.7468604560795313 ) ) ;
#65394 = CIRCLE ( 'NONE', #32105, 7.910944475430059519 ) ;
#65395 = CARTESIAN_POINT ( 'NONE',  ( 30.65384604593693751, -282.6947087488522357, -241.9478560911747991 ) ) ;
#65396 = CARTESIAN_POINT ( 'NONE',  ( -19.09330153368558669, -275.8909357807982019, -198.7998241819788632 ) ) ;
#65397 = CARTESIAN_POINT ( 'NONE',  ( -5.768207181670216954, -284.2440025502988306, -339.7120729934683254 ) ) ;
#65398 = CARTESIAN_POINT ( 'NONE',  ( 35.74926881489287922, -280.2521616892001362, -263.1273887159953802 ) ) ;
#65399 = CARTESIAN_POINT ( 'NONE',  ( -111.8890924574281769, -280.4408017308335843, -279.0460350030853078 ) ) ;
#65400 = CARTESIAN_POINT ( 'NONE',  ( 7.989098699796488567, -298.6050200815838025, -193.3611049961748733 ) ) ;
#65401 = CARTESIAN_POINT ( 'NONE',  ( -32.68048220623310129, -273.9426626004316176, -193.4891809416664330 ) ) ;
#65402 = CARTESIAN_POINT ( 'NONE',  ( 32.90695643179160612, -295.7954077118255896, -295.1416201410072517 ) ) ;
#65403 = FACE_OUTER_BOUND ( 'NONE', #22215, .T. ) ;
#65404 = ADVANCED_FACE ( 'NONE', ( #42580 ), #79529, .T. ) ;
#65405 = CARTESIAN_POINT ( 'NONE',  ( 185.4166944662832179, 275.0000000000000568, 23.37680765314684450 ) ) ;
#65406 = CARTESIAN_POINT ( 'NONE',  ( -14.18249961170248952, -292.8945004373529173, -342.4995745099487294 ) ) ;
#65407 = CARTESIAN_POINT ( 'NONE',  ( -81.10285726640799453, -272.9473074455739834, -211.7916604016508018 ) ) ;
#65408 = EDGE_CURVE ( 'NONE', #36970, #49439, #22216, .T. ) ;
#65409 = CARTESIAN_POINT ( 'NONE',  ( 31.55158653322001072, -294.6464949850137600, -237.4295049089770941 ) ) ;
#65411 = CARTESIAN_POINT ( 'NONE',  ( -64.26370223029951489, -292.9137546359443149, -198.5890211695690368 ) ) ;
#65410 = CARTESIAN_POINT ( 'NONE',  ( -111.2869819898779866, -299.4805209788416391, -234.7871824221999191 ) ) ;
#65412 = CARTESIAN_POINT ( 'NONE',  ( -23.41972997224582187, -290.8740657442138513, -343.9410331998058155 ) ) ;
#65413 = CARTESIAN_POINT ( 'NONE',  ( -111.4333763521071745, -276.6918485243790542, -259.4928026283280360 ) ) ;
#65414 = CARTESIAN_POINT ( 'NONE',  ( -67.36138853243748770, -279.3691165322459824, -338.4796360849477423 ) ) ;
#65415 = CARTESIAN_POINT ( 'NONE',  ( 22.46917672270312494, -292.2413821474057158, -314.6778553463686308 ) ) ;
#65416 = CARTESIAN_POINT ( 'NONE',  ( 34.15408124983567717, -283.0893611010644690, -245.1314981090466176 ) ) ;
#65417 = CARTESIAN_POINT ( 'NONE',  ( -100.4215314072840357, -283.7141848003756195, -307.1445704102478658 ) ) ;
#65418 = CARTESIAN_POINT ( 'NONE',  ( -45.25520502765089503, -281.0339476568632904, -194.0268289148439180 ) ) ;
#65419 = CARTESIAN_POINT ( 'NONE',  ( -67.02097820176535947, -284.4665939125920886, -199.7413674011825151 ) ) ;
#65420 = CARTESIAN_POINT ( 'NONE',  ( -82.39846438558102193, -278.5920580619810494, -332.5118074958356829 ) ) ;
#65421 =( LENGTH_UNIT ( ) NAMED_UNIT ( * ) SI_UNIT ( .MILLI., .METRE. ) );
#65422 = CARTESIAN_POINT ( 'NONE',  ( 30.62389622713492088, -276.6214235350834656, -235.6712712979976061 ) ) ;
#65423 = CARTESIAN_POINT ( 'NONE',  ( 27.33386217378599881, -289.6233781216987495, -239.1787733560258573 ) ) ;
#65424 = ORIENTED_EDGE ( 'NONE', *, *, #89197, .F. ) ;
#65425 = CARTESIAN_POINT ( 'NONE',  ( -102.3220523543144083, -275.0496087516776811, -233.1410596474597980 ) ) ;
#65426 = CARTESIAN_POINT ( 'NONE',  ( -62.36443268595444778, -275.3992213541168894, -340.7418164892691834 ) ) ;
#65427 = CARTESIAN_POINT ( 'NONE',  ( -111.6537581266353385, -292.5140871069919513, -254.4348366466839764 ) ) ;
#65428 = CARTESIAN_POINT ( 'NONE',  ( 35.30725766619008965, -293.0136250102835334, -278.9307132030334628 ) ) ;
#65429 = CARTESIAN_POINT ( 'NONE',  ( 35.79249968725556386, -286.7570320682622196, -246.2968497567650843 ) ) ;
#65430 = CARTESIAN_POINT ( 'NONE',  ( 184.7149167944524493, -12.49482340714361506, 10.00000000000000000 ) ) ;
#65432 = CARTESIAN_POINT ( 'NONE',  ( -65.64110728933360406, -281.8283714908260436, -338.5333883263651273 ) ) ;
#65431 = CARTESIAN_POINT ( 'NONE',  ( -55.94453029314470882, -293.8618986950617114, -344.4727972318981415 ) ) ;
#65433 = CARTESIAN_POINT ( 'NONE',  ( -95.04978968866063838, -291.7630146487596221, -317.0584614092593938 ) ) ;
#65434 = CARTESIAN_POINT ( 'NONE',  ( -93.77367295465313646, -283.6987636910453716, -222.9676564391809279 ) ) ;
#65435 = CARTESIAN_POINT ( 'NONE',  ( -29.37465881075294760, -284.2644416329409296, -343.4720051016085449 ) ) ;
#65436 = CARTESIAN_POINT ( 'NONE',  ( -85.00915919480364380, -290.6326118990021996, -330.6006312189260825 ) ) ;
#65437 = CARTESIAN_POINT ( 'NONE',  ( 32.03306184477783347, -281.7386492707062757, -247.2859726534441904 ) ) ;
#65438 = CARTESIAN_POINT ( 'NONE',  ( 26.17388718873376519, -292.9142299230162507, -313.1837625335593884 ) ) ;
#65439 = CARTESIAN_POINT ( 'NONE',  ( 27.31446838273954114, -288.9018811909086253, -311.9771757873883189 ) ) ;
#65440 = CARTESIAN_POINT ( 'NONE',  ( 37.76624037033315773, -288.2540610654318129, -287.1043363598174665 ) ) ;
#65441 = CARTESIAN_POINT ( 'NONE',  ( -44.02648922586983105, -286.1319602043271857, -197.6678335663120265 ) ) ;
#65442 = ORIENTED_EDGE ( 'NONE', *, *, #22580, .F. ) ;
#65443 = CARTESIAN_POINT ( 'NONE',  ( 195.5206343625570753, 25.57665861450641742, 12.82293366630988629 ) ) ;
#65444 = CARTESIAN_POINT ( 'NONE',  ( -37.65962831952445100, -296.9164669897316458, -346.1381236568839768 ) ) ;
#65445 = CARTESIAN_POINT ( 'NONE',  ( -55.96654247815905592, -293.9719792569031824, -344.5663301908441554 ) ) ;
#65446 = CARTESIAN_POINT ( 'NONE',  ( -81.41996954108472551, -278.4948988909398508, -211.8122817654414405 ) ) ;
#65447 = CARTESIAN_POINT ( 'NONE',  ( -87.99114111674450101, -272.8738213400088739, -212.3751713304318400 ) ) ;
#65448 = CARTESIAN_POINT ( 'NONE',  ( -2.836089684496048147, -293.0671690360529169, -335.4769424931977824 ) ) ;
#65449 = CARTESIAN_POINT ( 'NONE',  ( 35.84028343590882315, -277.1672602316328948, -259.2138574475316091 ) ) ;
#65450 = CARTESIAN_POINT ( 'NONE',  ( -34.40743603492575886, -296.3292324131429609, -196.3486720200830860 ) ) ;
#65451 = CARTESIAN_POINT ( 'NONE',  ( 25.17809604026358272, -294.2289105848749386, -231.8146238006975750 ) ) ;
#65452 = CARTESIAN_POINT ( 'NONE',  ( 18.21564661652627137, -295.3102711596413883, -318.2092005615400012 ) ) ;
#65453 = CARTESIAN_POINT ( 'NONE',  ( 29.33919985515026596, -212.1443419142231051, 22.50000000000000000 ) ) ;
#65454 = CARTESIAN_POINT ( 'NONE',  ( -112.5329910453490925, -294.5259416621192372, -272.3941710822987829 ) ) ;
#65455 = CARTESIAN_POINT ( 'NONE',  ( -106.7018606971562633, -273.7797540816976039, -237.2956231907605229 ) ) ;
#65456 = CARTESIAN_POINT ( 'NONE',  ( 156.4947056272797852, 21.00000000000000000, 15.00000000000000000 ) ) ;
#65457 = CARTESIAN_POINT ( 'NONE',  ( -108.5765029324005297, -291.2698433297636598, -287.3614508714329077 ) ) ;
#65459 = CARTESIAN_POINT ( 'NONE',  ( -63.57262629906725238, -295.7368371833783272, -338.5617810344954250 ) ) ;
#65458 = AXIS2_PLACEMENT_3D ( 'NONE', #37252, #45260, #73711 ) ;
#65460 = CARTESIAN_POINT ( 'NONE',  ( -94.87668091974316553, -279.8618483902931757, -319.0444902304431594 ) ) ;
#65461 = CARTESIAN_POINT ( 'NONE',  ( -113.5891559565257580, -277.1500210284460195, -277.2697733443259267 ) ) ;
#65462 = CARTESIAN_POINT ( 'NONE',  ( 17.74745361342931105, -281.6380170796243192, -324.0888299054577146 ) ) ;
#65463 = CARTESIAN_POINT ( 'NONE',  ( 26.06522289078438348, -274.3255459448911893, -226.8305931864368574 ) ) ;
#65464 = CARTESIAN_POINT ( 'NONE',  ( -110.9255369692004081, -282.4820745524079371, -281.9501052623288047 ) ) ;
#65465 = CARTESIAN_POINT ( 'NONE',  ( -39.54351107313486580, -278.4248479933576732, -194.1800173669438436 ) ) ;
#65466 = CARTESIAN_POINT ( 'NONE',  ( -87.68424627207404853, -277.3507448703946352, -214.5430521636019989 ) ) ;
#65467 = ADVANCED_FACE ( 'NONE', ( #21764 ), #7089, .F. ) ;
#65468 = CARTESIAN_POINT ( 'NONE',  ( -73.07208807262840367, -296.2527589669163604, -206.1382026333387216 ) ) ;
#65469 = CARTESIAN_POINT ( 'NONE',  ( 35.00224187855551605, -277.8072619752724677, -290.1918125183523216 ) ) ;
#65470 = CARTESIAN_POINT ( 'NONE',  ( 195.6096107219261171, 24.54133239209091499, 12.68062660795851571 ) ) ;
#65471 = CARTESIAN_POINT ( 'NONE',  ( -17.04487854568082739, -290.3330541484819491, -197.7908359538226080 ) ) ;
#65472 = CARTESIAN_POINT ( 'NONE',  ( -113.6661420330862597, -290.6843165575915577, -259.7933605849357264 ) ) ;
#65473 = CARTESIAN_POINT ( 'NONE',  ( -31.43026629616741019, -276.1267746477807350, -195.4142928862090969 ) ) ;
#65474 = CARTESIAN_POINT ( 'NONE',  ( -50.24562860623797889, -295.8868865773580410, -196.6487238169881664 ) ) ;
#65475 = CARTESIAN_POINT ( 'NONE',  ( -105.2845240311445565, -284.2149525763747988, -234.3594596461950630 ) ) ;
#65476 = DIRECTION ( 'NONE',  ( 0.000000000000000000, -1.000000000000000000, 0.000000000000000000 ) ) ;
#65477 = CARTESIAN_POINT ( 'NONE',  ( -89.27099874892783760, -281.7823620416045856, -324.5464073047963893 ) ) ;
#65478 = AXIS2_PLACEMENT_3D ( 'NONE', #26571, #55459, #47859 ) ;
#65479 = DIRECTION ( 'NONE',  ( 0.000000000000000000, 1.000000000000000000, 0.000000000000000000 ) ) ;
#65480 = CARTESIAN_POINT ( 'NONE',  ( -30.75614646379407802, -290.9321736974778219, -197.2600852417377268 ) ) ;
#65481 = CARTESIAN_POINT ( 'NONE',  ( -98.35791083786813260, -283.2713305277754330, -228.0552393574312759 ) ) ;
#65482 = DIRECTION ( 'NONE',  ( 0.000000000000000000, 1.000000000000000000, 0.000000000000000000 ) ) ;
#65483 = CARTESIAN_POINT ( 'NONE',  ( 157.1544330182169347, 16.98551211945809669, -7.440913067426857985 ) ) ;
#65484 = CARTESIAN_POINT ( 'NONE',  ( 34.24848929151041688, -291.8403679683247560, -292.7183411551075096 ) ) ;
#65485 = CARTESIAN_POINT ( 'NONE',  ( -96.64590069198710864, -282.3819847786404580, -318.3995661443665881 ) ) ;
#65486 = CARTESIAN_POINT ( 'NONE',  ( -24.16698785917438386, -278.4813948826387673, -343.0276467161061760 ) ) ;
#65487 = CARTESIAN_POINT ( 'NONE',  ( -69.63947779557744866, -286.8414734742384553, -200.8855970613653881 ) ) ;
#65488 = CARTESIAN_POINT ( 'NONE',  ( -103.4854645873572423, -284.9706639195849220, -239.3543580956023789 ) ) ;
#65489 = CARTESIAN_POINT ( 'NONE',  ( -41.87489294667201278, -278.5356331447423486, -343.8232890791103387 ) ) ;
#65490 = CARTESIAN_POINT ( 'NONE',  ( -104.5945117932865855, -279.7410652754268199, -241.5572805714275546 ) ) ;
#65491 = CARTESIAN_POINT ( 'NONE',  ( -88.54005977374177405, -287.3348173336079867, -215.4841763608947929 ) ) ;
#65492 = EDGE_LOOP ( 'NONE', ( #57174, #68774 ) ) ;
#65493 = CARTESIAN_POINT ( 'NONE',  ( -70.80979128418196922, -295.3147306903626941, -339.7217663970918693 ) ) ;
#65494 = CARTESIAN_POINT ( 'NONE',  ( -31.72293498328045658, -290.9609173104047386, -344.8459143688191375 ) ) ;
#65495 = CARTESIAN_POINT ( 'NONE',  ( 197.0539037881910929, 24.40160077877072098, 12.19936955022341607 ) ) ;
#65496 = CARTESIAN_POINT ( 'NONE',  ( 13.79469577742117714, -283.1948066931273615, -206.1857440867352693 ) ) ;
#65497 = VERTEX_POINT ( 'NONE', #79974 ) ;
#65498 = CARTESIAN_POINT ( 'NONE',  ( 23.37902115964356753, -292.5718400968868877, -316.3984335418881528 ) ) ;
#65499 = CARTESIAN_POINT ( 'NONE',  ( 34.05552348880730307, -288.8330223627122564, -252.0579997104457846 ) ) ;
#65500 = CARTESIAN_POINT ( 'NONE',  ( -92.06089399243730043, -281.0171072878628138, -220.5235434321706975 ) ) ;
#65501 = CARTESIAN_POINT ( 'NONE',  ( 25.37852856722543748, -289.5596237458603923, -314.0957705816539374 ) ) ;
#65502 = CARTESIAN_POINT ( 'NONE',  ( -99.16696148391430654, -285.9759625279380089, -312.9090712521626756 ) ) ;
#65503 = CARTESIAN_POINT ( 'NONE',  ( -112.0864308805788454, -278.9508717504500623, -251.8076854871989951 ) ) ;
#65504 = ORIENTED_EDGE ( 'NONE', *, *, #67502, .T. ) ;
#65505 = CARTESIAN_POINT ( 'NONE',  ( -2.650793769281881040, -292.6768713481646955, -337.4867853306007532 ) ) ;
#65506 = CARTESIAN_POINT ( 'NONE',  ( -3.655691844096808918, -280.3177541915674738, -201.1060561584997686 ) ) ;
#65508 = CARTESIAN_POINT ( 'NONE',  ( -65.05148502367389085, -275.5466795367907480, -201.4777244248728607 ) ) ;
#65507 = CIRCLE ( 'NONE', #18635, 0.9999999999999985567 ) ;
#65509 = CARTESIAN_POINT ( 'NONE',  ( 200.1087902362374678, 299.5637500031161267, -5.714653251563827752 ) ) ;
#65510 = CARTESIAN_POINT ( 'NONE',  ( -37.37352853689063892, -288.5519495502701943, -195.3611179825600175 ) ) ;
#65511 = CARTESIAN_POINT ( 'NONE',  ( -65.82628503182380086, -271.9244892412024797, -199.9013952259350617 ) ) ;
#65513 = CIRCLE ( 'NONE', #44312, 25.00000000000000355 ) ;
#65512 = DIRECTION ( 'NONE',  ( 0.000000000000000000, 0.9681751575201845705, 0.2502735790305594676 ) ) ;
#65514 = CARTESIAN_POINT ( 'NONE',  ( -105.5695062337035495, -278.4102139373451337, -244.0860417251003582 ) ) ;
#65515 = CIRCLE ( 'NONE', #3425, 7.500000000000012434 ) ;
#65516 = CARTESIAN_POINT ( 'NONE',  ( -4.152925742680994681, -277.8293433113927335, -339.4154884680469308 ) ) ;
#65517 = CARTESIAN_POINT ( 'NONE',  ( -110.8348508120440101, -273.8671145409825840, -270.3778243577502280 ) ) ;
#65518 = CARTESIAN_POINT ( 'NONE',  ( -85.96262405029688125, -282.7659978014171429, -329.7650401529969599 ) ) ;
#65519 = CARTESIAN_POINT ( 'NONE',  ( -111.1310151358370888, -292.2293141695091094, -276.7392357874032314 ) ) ;
#65520 = CARTESIAN_POINT ( 'NONE',  ( -9.445442236418003290, -299.9155321296868237, -194.0473822636144519 ) ) ;
#65521 = CIRCLE ( 'NONE', #24661, 7.500000000000012434 ) ;
#65522 = CARTESIAN_POINT ( 'NONE',  ( -60.04512324328197082, -298.9694991932984180, -197.1446637508538515 ) ) ;
#65523 = CARTESIAN_POINT ( 'NONE',  ( 4.871037225636397849, -296.4805289426475383, -332.1520010429561580 ) ) ;
#65524 = CARTESIAN_POINT ( 'NONE',  ( -108.7425469832865872, -282.2623234403394576, -292.7653027514992345 ) ) ;
#65525 = CIRCLE ( 'NONE', #18650, 5.103083949679981579 ) ;
#65526 = CARTESIAN_POINT ( 'NONE',  ( -105.8801740222697561, -270.9623925700839209, -240.6612547418662871 ) ) ;
#65527 = CARTESIAN_POINT ( 'NONE',  ( 34.09706668135849839, -288.8135444252168327, -243.8480455293226896 ) ) ;
#65528 = ADVANCED_FACE ( 'NONE', ( #51086, #15112 ), #6626, .T. ) ;
#65529 = CARTESIAN_POINT ( 'NONE',  ( -10.62420498176592965, -287.6157347416850030, -338.6826924085395945 ) ) ;
#65530 = CARTESIAN_POINT ( 'NONE',  ( -110.9628874742100777, -271.9671495687064748, -296.3246994010440858 ) ) ;
#65531 = EDGE_LOOP ( 'NONE', ( #47544, #80171, #58562, #66012 ) ) ;
#65532 = CARTESIAN_POINT ( 'NONE',  ( -113.5265521581347201, -289.0446614328807868, -276.8850786413128731 ) ) ;
#65533 = CARTESIAN_POINT ( 'NONE',  ( 16.02351505426820566, -287.9362158221861705, -320.2772619269998131 ) ) ;
#65534 = ORIENTED_EDGE ( 'NONE', *, *, #28465, .T. ) ;
#65535 = CARTESIAN_POINT ( 'NONE',  ( -69.67509314950392252, -286.7160894653333685, -200.8051369070755641 ) ) ;
#65536 = VECTOR ( 'NONE', #17226, 1000.000000000000000 ) ;
#65537 = CARTESIAN_POINT ( 'NONE',  ( -64.33701090352067808, -277.7475424969254050, -338.2627374946621330 ) ) ;
#65538 = EDGE_CURVE ( 'NONE', #41863, #29328, #5067, .T. ) ;
#65539 = CARTESIAN_POINT ( 'NONE',  ( 36.79421480341117956, -292.7192364340471613, -289.9916714093535575 ) ) ;
#65540 = CARTESIAN_POINT ( 'NONE',  ( -30.21606924908947533, -283.6156446163547571, -346.9283314038112280 ) ) ;
#65541 = CARTESIAN_POINT ( 'NONE',  ( 37.46966477689971242, -283.2619751327841300, -285.3933312492559935 ) ) ;
#65542 = CARTESIAN_POINT ( 'NONE',  ( -52.90918733402959617, -283.5795723328850499, -345.8039067124552730 ) ) ;
#65543 = CARTESIAN_POINT ( 'NONE',  ( 27.79833626442015415, -281.4361868750625604, -237.2510877576574160 ) ) ;
#65544 = CARTESIAN_POINT ( 'NONE',  ( 121.9602794296661017, 149.5214840255910360, -263.6741255141749889 ) ) ;
#65545 = CARTESIAN_POINT ( 'NONE',  ( -111.3001811514157851, -280.4054939237981330, -281.7703910497300512 ) ) ;
#65546 = CARTESIAN_POINT ( 'NONE',  ( -108.4282835402909200, -261.3898650898953520, -317.1797982494042003 ) ) ;
#65547 = CARTESIAN_POINT ( 'NONE',  ( -108.9999068415822450, -263.8798383989249601, -305.4964869628947781 ) ) ;
#65548 = CIRCLE ( 'NONE', #14167, 7.999999999999992895 ) ;
#65549 = CARTESIAN_POINT ( 'NONE',  ( -35.37576289747776315, -273.2745857515132570, -197.2135263685501627 ) ) ;
#65550 = CARTESIAN_POINT ( 'NONE',  ( -16.52955750363717868, -294.2980092150471023, -344.4864180480755635 ) ) ;
#65551 = CARTESIAN_POINT ( 'NONE',  ( 139.3042675125565211, 178.0593506817157561, -238.4361927324221995 ) ) ;
#65552 = CARTESIAN_POINT ( 'NONE',  ( -80.95542691221804432, -272.1587295010256184, -207.4388264342572654 ) ) ;
#65553 = CARTESIAN_POINT ( 'NONE',  ( -100.9674855778340685, -298.9311831010950300, -232.0168203863419478 ) ) ;
#65554 = CARTESIAN_POINT ( 'NONE',  ( 30.94959958044641724, -289.2298844993276248, -297.6561756056091781 ) ) ;
#65555 = ORIENTED_EDGE ( 'NONE', *, *, #49649, .T. ) ;
#65556 = CARTESIAN_POINT ( 'NONE',  ( -61.50609399691204260, -296.2996758059447302, -343.2788974716046368 ) ) ;
#65557 = CARTESIAN_POINT ( 'NONE',  ( -38.63227807983282958, -286.5279199974649487, -197.2984865787412332 ) ) ;
#65558 = CARTESIAN_POINT ( 'NONE',  ( -49.65599822687256193, -272.8191005767642423, -194.6117532226535616 ) ) ;
#65559 = CIRCLE ( 'NONE', #21655, 4.025000000000000355 ) ;
#65560 = CARTESIAN_POINT ( 'NONE',  ( 37.90169481907362581, -294.1589728779382540, -254.7213592204973338 ) ) ;
#65561 = CARTESIAN_POINT ( 'NONE',  ( -0.8385869307530524619, -293.0160264751180534, -202.6333568335425070 ) ) ;
#65562 = CARTESIAN_POINT ( 'NONE',  ( -64.07358651758011092, -291.8601918360130298, -202.4181636152756880 ) ) ;
#65563 = ORIENTED_EDGE ( 'NONE', *, *, #2379, .F. ) ;
#65564 = CARTESIAN_POINT ( 'NONE',  ( -27.21419690957961279, -276.0999279833812352, -195.4304681298480375 ) ) ;
#65565 = CARTESIAN_POINT ( 'NONE',  ( 39.15877469630972030, -274.2857222915546913, -265.4804497280269970 ) ) ;
#65566 = ORIENTED_EDGE ( 'NONE', *, *, #33379, .F. ) ;
#65567 = CARTESIAN_POINT ( 'NONE',  ( -99.60365762841171033, -277.4593997588095817, -315.5828097142248225 ) ) ;
#65568 = UNCERTAINTY_MEASURE_WITH_UNIT (LENGTH_MEASURE( 1.000000000000000082E-05 ), #41729, 'distance_accuracy_value', 'NONE');
#65569 = CARTESIAN_POINT ( 'NONE',  ( -3.722251669737950408, -272.9032473839519071, -204.6493414318743476 ) ) ;
#65570 = CARTESIAN_POINT ( 'NONE',  ( -51.63513270364259000, -274.9448179925313980, -198.4069245620116817 ) ) ;
#65571 = CARTESIAN_POINT ( 'NONE',  ( 30.38786864103631657, -276.1196300856387325, -242.3691887509122012 ) ) ;
#65572 = CARTESIAN_POINT ( 'NONE',  ( -101.8704918431633786, -274.8441914698143478, -230.2361998846719757 ) ) ;
#65573 = CARTESIAN_POINT ( 'NONE',  ( -3.487147892860260168, -274.6276798500598488, -337.6976617855184486 ) ) ;
#65574 = CARTESIAN_POINT ( 'NONE',  ( -94.01631526056149823, -296.5506896284615550, -316.5530822314275383 ) ) ;
#65575 = CARTESIAN_POINT ( 'NONE',  ( 31.12717615511658664, -292.4863139314028331, -297.4705808300105332 ) ) ;
#65576 = CARTESIAN_POINT ( 'NONE',  ( 198.2695878509457543, 40.57393790395538247, 11.03083405179679666 ) ) ;
#65577 = CARTESIAN_POINT ( 'NONE',  ( -106.2874478220169863, -278.6039259086215907, -304.6278647257012722 ) ) ;
#65578 = CARTESIAN_POINT ( 'NONE',  ( -2.915533270563619883, -274.6872931473909603, -205.9884604327900774 ) ) ;
#65579 = CARTESIAN_POINT ( 'NONE',  ( -111.8754825022579951, -283.4542770260279667, -253.0980487261579981 ) ) ;
#65580 = CARTESIAN_POINT ( 'NONE',  ( -94.17814276327253253, -297.8715440682574922, -319.5510276953405651 ) ) ;
#65581 = DIRECTION ( 'NONE',  ( 0.5877852522924685852, 0.000000000000000000, -0.8090169943749507819 ) ) ;
#65582 = AXIS2_PLACEMENT_3D ( 'NONE', #92552, #42842, #71278 ) ;
#65583 = CARTESIAN_POINT ( 'NONE',  ( -41.32151313304918006, -285.1979647738228323, -197.2954412939511144 ) ) ;
#65584 = CARTESIAN_POINT ( 'NONE',  ( -87.80255211493745549, -276.0089338905548857, -324.5060755362359828 ) ) ;
#65585 = CARTESIAN_POINT ( 'NONE',  ( -94.07177930449284986, -276.4675461529768086, -317.2538134764875508 ) ) ;
#65586 = CARTESIAN_POINT ( 'NONE',  ( -112.3502763745730562, -286.5198263715149096, -272.8915676756419657 ) ) ;
#65587 = CARTESIAN_POINT ( 'NONE',  ( 23.37220969433365525, -276.1864920688550455, -229.0959857785408360 ) ) ;
#65588 = CARTESIAN_POINT ( 'NONE',  ( 208.4306832106270804, -199.2391364535880882, 0.000000000000000000 ) ) ;
#65589 = AXIS2_PLACEMENT_3D ( 'NONE', #74280, #81841, #61030 ) ;
#65590 = CARTESIAN_POINT ( 'NONE',  ( 33.43356009749853541, -274.3156399060009107, -298.7398347481271230 ) ) ;
#65591 = AXIS2_PLACEMENT_3D ( 'NONE', #27457, #71020, #64422 ) ;
#65592 = CARTESIAN_POINT ( 'NONE',  ( -50.64088620623854098, -281.8828257183184292, -196.3803091640184562 ) ) ;
#65593 = CARTESIAN_POINT ( 'NONE',  ( 38.26201954786014880, -289.4868819838978311, -271.5046274318437440 ) ) ;
#65594 = CIRCLE ( 'NONE', #38304, 3.000000000000000000 ) ;
#65595 = CARTESIAN_POINT ( 'NONE',  ( 34.91680843867518291, -291.8126063833635726, -290.6402828075584353 ) ) ;
#65596 = CARTESIAN_POINT ( 'NONE',  ( 82.17160520760587872, -297.7678833447943703, -196.2839431741979297 ) ) ;
#65597 = CARTESIAN_POINT ( 'NONE',  ( -102.4596836479148863, -271.6988677413764321, -236.1790809474917125 ) ) ;
#65598 = CARTESIAN_POINT ( 'NONE',  ( -93.47523585989389971, -289.3724734215381318, -221.7824019793234527 ) ) ;
#65599 = CARTESIAN_POINT ( 'NONE',  ( 30.52007695399996479, -26.23604800832216100, -343.5755449821854768 ) ) ;
#65600 = CARTESIAN_POINT ( 'NONE',  ( -70.10895070716225064, -295.6202805390466324, -202.8977357441297613 ) ) ;
#65601 = CARTESIAN_POINT ( 'NONE',  ( -8.513175731833138471, -287.1614981346177160, -341.0266796032209413 ) ) ;
#65602 = CARTESIAN_POINT ( 'NONE',  ( -112.8105724428530010, -282.9042424062359942, -261.5054235241709648 ) ) ;
#65603 = CIRCLE ( 'NONE', #24739, 2.000000000000007105 ) ;
#65604 = CARTESIAN_POINT ( 'NONE',  ( -83.14742077496897821, -285.1184776164806181, -328.0217259743778868 ) ) ;
#65605 = CARTESIAN_POINT ( 'NONE',  ( -97.65969248434043948, -284.7788278585090325, -311.8540038671407615 ) ) ;
#65606 = CARTESIAN_POINT ( 'NONE',  ( -51.35419568960561776, -291.2103653891529689, -344.4020307813381123 ) ) ;
#65607 = CARTESIAN_POINT ( 'NONE',  ( -63.55388432643461982, -274.0529384340632078, -197.9824906741909842 ) ) ;
#65608 = AXIS2_PLACEMENT_3D ( 'NONE', #18047, #70128, #5264 ) ;
#65609 = CARTESIAN_POINT ( 'NONE',  ( 30.38564262801431681, -286.0720870260548736, -303.9801053340400472 ) ) ;
#65610 = CARTESIAN_POINT ( 'NONE',  ( 29.94753258409132712, -275.0656987043681738, -232.8194162944809307 ) ) ;
#65611 = CARTESIAN_POINT ( 'NONE',  ( 35.68180583284402729, -295.7324524997122239, -285.8955450662704152 ) ) ;
#65612 = DIRECTION ( 'NONE',  ( 0.000000000000000000, -0.000000000000000000, 1.000000000000000000 ) ) ;
#65613 = CARTESIAN_POINT ( 'NONE',  ( -69.85430415644619018, -297.9805209788416391, -337.9475929042657754 ) ) ;
#65614 = CARTESIAN_POINT ( 'NONE',  ( -40.27066669121460052, -281.7745612761715392, -343.7958824602116579 ) ) ;
#65615 = CARTESIAN_POINT ( 'NONE',  ( -93.84978376405879885, -275.8649272231995155, -319.9278902430459652 ) ) ;
#65616 = CARTESIAN_POINT ( 'NONE',  ( -46.77591700506830819, -272.4143134296629114, -194.6398970231161627 ) ) ;
#65617 = CARTESIAN_POINT ( 'NONE',  ( -6.240783130062105499, -275.9809884557118380, -336.5309750321059141 ) ) ;
#65618 = B_SPLINE_CURVE_WITH_KNOTS ( 'NONE', 3,
 ( #37890, #36515, #79618, #16598, #14760, #66795, #38363, #58317 ),
 .UNSPECIFIED., .F., .F.,
 ( 4, 2, 2, 4 ),
 ( 0.000000000000000000, 0.001028958187123778451, 0.001543437280685668002, 0.002057916374247557769 ),
 .UNSPECIFIED. ) ;
#65619 = CARTESIAN_POINT ( 'NONE',  ( 2.600182152513579759, -294.1181409809346405, -208.3704448016505637 ) ) ;
#65620 = VECTOR ( 'NONE', #6566, 1000.000000000000000 ) ;
#65621 = CARTESIAN_POINT ( 'NONE',  ( 34.30024907722243910, -294.6939803633845258, -285.6147210171870938 ) ) ;
#65622 = CARTESIAN_POINT ( 'NONE',  ( 34.88961699931628857, -294.6589912247051188, -245.2763189657629823 ) ) ;
#65623 = CARTESIAN_POINT ( 'NONE',  ( 19.99791316113373085, -294.1767997048375491, -219.6908910885088346 ) ) ;
#65624 = CARTESIAN_POINT ( 'NONE',  ( -107.4587765877218288, -296.6541364877508045, -250.0486687637107934 ) ) ;
#65625 = CARTESIAN_POINT ( 'NONE',  ( -111.5996612287716090, -292.4160058654288150, -280.9770965847881712 ) ) ;
#65626 = CARTESIAN_POINT ( 'NONE',  ( -96.26894314102001715, -284.0512335491926024, -319.9454166209545178 ) ) ;
#65627 = CARTESIAN_POINT ( 'NONE',  ( -93.21803652644112503, -271.3992645476581629, -219.1742014041453785 ) ) ;
#65628 = CARTESIAN_POINT ( 'NONE',  ( -20.98189734052662558, -286.0898370103569164, -195.1191293243878988 ) ) ;
#65629 = CARTESIAN_POINT ( 'NONE',  ( -26.76406421823233472, -278.8968461953814426, -344.2526629606987854 ) ) ;
#65630 = CARTESIAN_POINT ( 'NONE',  ( -105.9305712482647834, -283.6940511114416950, -244.2326418962472871 ) ) ;
#65631 = CARTESIAN_POINT ( 'NONE',  ( 23.92640212349585127, -284.9640712534156819, -227.0813618578237367 ) ) ;
#65632 = CARTESIAN_POINT ( 'NONE',  ( -90.17949863009447142, -277.4547054888250273, -215.9881621528031701 ) ) ;
#65633 = CARTESIAN_POINT ( 'NONE',  ( -117.0946091816712453, -269.6096274233381109, -270.3236525939013859 ) ) ;
#65634 = CARTESIAN_POINT ( 'NONE',  ( 30.73134748356642376, -283.2123812505230376, -305.4904348895843214 ) ) ;
#65635 = AXIS2_PLACEMENT_3D ( 'NONE', #41835, #26715, #62728 ) ;
#65636 = CARTESIAN_POINT ( 'NONE',  ( 10.07317217267784137, -287.4757265666959256, -330.7996713298073814 ) ) ;
#65637 = CARTESIAN_POINT ( 'NONE',  ( -94.59609192810681577, -279.4646343958065700, -320.6440677386422635 ) ) ;
#65638 = CARTESIAN_POINT ( 'NONE',  ( -2.931808993251968865, -277.9222129484760444, -338.7076699259418433 ) ) ;
#65639 = CARTESIAN_POINT ( 'NONE',  ( -68.52136485102623453, -279.4639430213114224, -204.3548416726315509 ) ) ;
#65640 = CARTESIAN_POINT ( 'NONE',  ( 34.46282722726831338, -293.1982532621263999, -242.4089174557115598 ) ) ;
#65641 = CARTESIAN_POINT ( 'NONE',  ( 4.516562378373683018, -286.5048284922152675, -332.2274174111881280 ) ) ;
#65642 = CARTESIAN_POINT ( 'NONE',  ( -97.72692606006464189, -292.7791532713339961, -223.8634983215192165 ) ) ;
#65643 = CARTESIAN_POINT ( 'NONE',  ( -18.15277336290058585, -293.7192567396938898, -341.1142886700226313 ) ) ;
#65644 = CARTESIAN_POINT ( 'NONE',  ( 22.94804982942261873, -293.7930158145457540, -311.6470271200916500 ) ) ;
#65645 = CARTESIAN_POINT ( 'NONE',  ( -111.3381887744287013, -291.8857677029655520, -250.1615096632381778 ) ) ;
#65646 = CARTESIAN_POINT ( 'NONE',  ( 29.41092191300931802, -282.6057562661483189, -300.2844335558414173 ) ) ;
#65647 = EDGE_CURVE ( 'NONE', #34882, #17985, #43971, .T. ) ;
#65648 = CARTESIAN_POINT ( 'NONE',  ( -114.1059607011668362, -271.6469132745270940, -267.4904571022046866 ) ) ;
#65649 = CARTESIAN_POINT ( 'NONE',  ( -43.16628952759693050, -289.7752909140342013, -347.0382784994224039 ) ) ;
#65650 = CARTESIAN_POINT ( 'NONE',  ( -63.50801472316615559, -281.5291653128440430, -341.4640677133127724 ) ) ;
#65651 = CARTESIAN_POINT ( 'NONE',  ( -41.75510213338536403, -289.4395742089017745, -347.2265725225928463 ) ) ;
#65652 = CARTESIAN_POINT ( 'NONE',  ( -46.73179300374368239, -286.2630749785448643, -197.8954559741196988 ) ) ;
#65653 = CARTESIAN_POINT ( 'NONE',  ( 104.2209783822911646, -299.5541904835127980, -195.3611179825600175 ) ) ;
#65654 = VECTOR ( 'NONE', #18844, 1000.000000000000000 ) ;
#65655 = CARTESIAN_POINT ( 'NONE',  ( 101.4506851708696473, 116.4004253888254112, -281.2237119222594970 ) ) ;
#65656 = CARTESIAN_POINT ( 'NONE',  ( -109.9537836488778026, -268.4403653933277383, -295.2708550661919276 ) ) ;
#65657 = CARTESIAN_POINT ( 'NONE',  ( -94.05924625524917815, -278.4020502465177174, -224.1472489729320614 ) ) ;
#65658 = CARTESIAN_POINT ( 'NONE',  ( -19.44584356988162810, -279.2079903894094741, -199.2173638768322235 ) ) ;
#65659 = CARTESIAN_POINT ( 'NONE',  ( -46.87417256749950667, -273.6009629694686396, -193.9747562373963490 ) ) ;
#65660 = CARTESIAN_POINT ( 'NONE',  ( 198.3562286197148410, 281.9606030181009828, -110.7138469406835100 ) ) ;
#65661 = CARTESIAN_POINT ( 'NONE',  ( -97.22372735001258093, -277.7669456291655479, -222.8979837474010139 ) ) ;
#65663 = CARTESIAN_POINT ( 'NONE',  ( -103.2347835030742402, -282.1036022958002150, -305.5418156893044284 ) ) ;
#65662 = AXIS2_PLACEMENT_3D ( 'NONE', #57775, #21791, #21311 ) ;
#65664 = CARTESIAN_POINT ( 'NONE',  ( -39.06212939791685557, -296.8335992799869132, -346.3283091877803486 ) ) ;
#65665 = CARTESIAN_POINT ( 'NONE',  ( -25.40520933008716753, -292.7006154623310294, -198.2297198930030504 ) ) ;
#65666 = CARTESIAN_POINT ( 'NONE',  ( -96.96846295032291607, -288.6401845323081830, -313.3249706284229319 ) ) ;
#65667 = CARTESIAN_POINT ( 'NONE',  ( -36.54771265828082960, -298.5541877098402210, -193.4225916368854996 ) ) ;
#65668 = CARTESIAN_POINT ( 'NONE',  ( -110.2124125022334056, -296.7761210569072432, -266.0183904329023790 ) ) ;
#65669 = ORIENTED_EDGE ( 'NONE', *, *, #17385, .T. ) ;
#65670 = DIRECTION ( 'NONE',  ( -0.01818181818182024526, 0.000000000000000000, -0.9998346970812742596 ) ) ;
#65671 = VECTOR ( 'NONE', #54834, 1000.000000000000000 ) ;
#65672 = AXIS2_PLACEMENT_3D ( 'NONE', #49547, #93553, #6002 ) ;
#65673 = CARTESIAN_POINT ( 'NONE',  ( -109.1882311765221658, -280.7741451873852156, -246.7985140577095819 ) ) ;
#65674 = CIRCLE ( 'NONE', #52051, 4.999999999999990230 ) ;
#65675 = CARTESIAN_POINT ( 'NONE',  ( -32.95821086214761664, -281.1883489703806163, -197.1831766622930218 ) ) ;
#65676 = CARTESIAN_POINT ( 'NONE',  ( -102.7223172990467219, -279.7999245629074494, -309.1856785222297503 ) ) ;
#65677 = CARTESIAN_POINT ( 'NONE',  ( 14.08138906443866389, -281.3674728372805021, -322.5772519283208908 ) ) ;
#65678 = CARTESIAN_POINT ( 'NONE',  ( 7.770473463442780115, -273.1610053400829088, -212.0893448470239377 ) ) ;
#65679 = CARTESIAN_POINT ( 'NONE',  ( 183.0442525570908288, 264.6571197653884155, -7.500000000000000000 ) ) ;
#65680 = CARTESIAN_POINT ( 'NONE',  ( 31.10181793048083776, -275.9042495949026943, -235.4377210147539188 ) ) ;
#65681 = VECTOR ( 'NONE', #19941, 1000.000000000000000 ) ;
#65682 = DIRECTION ( 'NONE',  ( 1.000000000000000000, 0.000000000000000000, 0.000000000000000000 ) ) ;
#65683 = CARTESIAN_POINT ( 'NONE',  ( 21.18132166857535736, -276.9069961144561489, -223.4360010145438764 ) ) ;
#65684 = CARTESIAN_POINT ( 'NONE',  ( -105.8254036949802810, -276.6866149929853691, -304.3710524893692764 ) ) ;
#65685 = EDGE_LOOP ( 'NONE', ( #89224, #10969, #30356, #50008 ) ) ;
#65686 = FACE_OUTER_BOUND ( 'NONE', #57704, .T. ) ;
#65687 = CARTESIAN_POINT ( 'NONE',  ( 8.234473884295582025, -284.4119733970817947, -330.3712768076471207 ) ) ;
#65688 = CARTESIAN_POINT ( 'NONE',  ( -94.41045300740755408, -290.3951056187565314, -224.5617513141136499 ) ) ;
#65689 = CARTESIAN_POINT ( 'NONE',  ( 20.21597755516480532, -286.2083622571286696, -219.2881259666707194 ) ) ;
#65690 = CARTESIAN_POINT ( 'NONE',  ( -106.1643664325362977, -282.4311266026384715, -297.7296655066767812 ) ) ;
#65692 = CARTESIAN_POINT ( 'NONE',  ( 36.42649006824807856, -285.4980268198166868, -260.0053142912898920 ) ) ;
#65691 = CARTESIAN_POINT ( 'NONE',  ( -64.28789304075455391, -281.9855355132146997, -338.8394182314698355 ) ) ;
#65693 = CARTESIAN_POINT ( 'NONE',  ( 36.08423256897204823, -282.7335852743458418, -268.5585956335388005 ) ) ;
#65694 = CARTESIAN_POINT ( 'NONE',  ( -70.49517678076114180, -271.6148902126982421, -203.0866975912457519 ) ) ;
#65695 = CARTESIAN_POINT ( 'NONE',  ( -78.07740889624230363, -283.9140962488267519, -205.9635835141338873 ) ) ;
#65696 = CARTESIAN_POINT ( 'NONE',  ( -50.10153223322036098, -297.2150176968947335, -344.3202717463917679 ) ) ;
#65697 = CARTESIAN_POINT ( 'NONE',  ( -109.8565215871018097, -279.6327864380735377, -259.7614434809553927 ) ) ;
#65698 = CARTESIAN_POINT ( 'NONE',  ( -97.88314763658974016, -287.1595758941229519, -225.7247776145287901 ) ) ;
#65699 = LINE ( 'NONE', #89625, #45813 ) ;
#65700 = EDGE_CURVE ( 'NONE', #60383, #34864, #53448, .T. ) ;
#65701 = ADVANCED_FACE ( 'NONE', ( #43066, #56835 ), #63471, .T. ) ;
#65702 = DIRECTION ( 'NONE',  ( 0.000000000000000000, 0.000000000000000000, 1.000000000000000000 ) ) ;
#65703 = CARTESIAN_POINT ( 'NONE',  ( 36.66523498722360586, -295.6665438404938300, -285.6021073289408037 ) ) ;
#65704 = CARTESIAN_POINT ( 'NONE',  ( -109.5367807850850994, -276.8139732431921516, -249.9943505465527380 ) ) ;
#65705 = CARTESIAN_POINT ( 'NONE',  ( 5.458883239541190591, -287.6857301087448491, -334.1754493158779269 ) ) ;
#65706 = CARTESIAN_POINT ( 'NONE',  ( 20.82589295685690800, -291.3185550414207228, -224.9207061888733961 ) ) ;
#65707 = CARTESIAN_POINT ( 'NONE',  ( -110.1076733507587875, -277.3767244782780494, -259.6956278307153525 ) ) ;
#65708 = CARTESIAN_POINT ( 'NONE',  ( -109.0222737768553714, -294.9430807871445381, -251.0051783274368518 ) ) ;
#65709 = CARTESIAN_POINT ( 'NONE',  ( -28.06056005679196730, -293.4874622176997150, -197.4052683278934808 ) ) ;
#65710 = DIRECTION ( 'NONE',  ( 0.000000000000000000, 1.000000000000000000, 0.000000000000000000 ) ) ;
#65711 = CARTESIAN_POINT ( 'NONE',  ( 185.0172044724083946, 249.5000000000000568, 22.46007009812148425 ) ) ;
#65712 = CARTESIAN_POINT ( 'NONE',  ( -96.87874999216938932, -294.3865439936605526, -318.1106985191667036 ) ) ;
#65713 = CARTESIAN_POINT ( 'NONE',  ( 35.07305991042505866, -289.3388423106831624, -284.6582934687115198 ) ) ;
#65714 = CARTESIAN_POINT ( 'NONE',  ( -105.6130552401944698, -288.3565481772901080, -303.8423876487195230 ) ) ;
#65715 = CARTESIAN_POINT ( 'NONE',  ( -82.89692537335099587, -291.1148297998149133, -328.1546848241031284 ) ) ;
#65716 = CARTESIAN_POINT ( 'NONE',  ( 222.8344101925596306, 0.000000000000000000, 21.50000000000000000 ) ) ;
#65717 = CARTESIAN_POINT ( 'NONE',  ( -61.29825842609412945, -290.1742260355367762, -339.4891516687136459 ) ) ;
#65718 = DIRECTION ( 'NONE',  ( 0.000000000000000000, 0.000000000000000000, -1.000000000000000000 ) ) ;
#65719 = CARTESIAN_POINT ( 'NONE',  ( -45.96574628048999500, -290.3641362977431868, -346.5298986650830102 ) ) ;
#65720 = CARTESIAN_POINT ( 'NONE',  ( -3.114213563330051393, -278.5220781646007708, -203.2133581906317659 ) ) ;
#65721 = AXIS2_PLACEMENT_3D ( 'NONE', #25248, #60320, #32820 ) ;
#65722 = CARTESIAN_POINT ( 'NONE',  ( -100.2341611294646242, -279.4729289279294449, -225.9732520647272622 ) ) ;
#65723 = CARTESIAN_POINT ( 'NONE',  ( 27.83571258969580597, -280.6812965225213929, -229.3020978850011034 ) ) ;
#65724 = CARTESIAN_POINT ( 'NONE',  ( 1.218207418715790968, -284.5664680352350047, -205.9722292622062128 ) ) ;
#65725 = CARTESIAN_POINT ( 'NONE',  ( -111.9369532652702759, -274.5219144271438836, -270.3861977745045237 ) ) ;
#65726 = CARTESIAN_POINT ( 'NONE',  ( -75.11421913820873897, -277.6831422793591173, -206.3950612263149935 ) ) ;
#65727 = CARTESIAN_POINT ( 'NONE',  ( -108.3398298335461192, -282.2393248531168410, -294.5327175635376875 ) ) ;
#65728 = CARTESIAN_POINT ( 'NONE',  ( -110.6395987583250218, -271.3322271344074466, -283.6871842494841758 ) ) ;
#65729 = CARTESIAN_POINT ( 'NONE',  ( -88.75933643169038589, -276.2385731889982594, -326.7431579257748240 ) ) ;
#65730 =( BOUNDED_SURFACE ( )  B_SPLINE_SURFACE ( 3, 2, ( 
 ( #1378, #60092, #81369 ),
 ( #88931, #32126, #52955 ),
 ( #38749, #59152, #60552 ),
 ( #89390, #39198, #68110 ),
 ( #3236, #89868, #25028 ),
 ( #80442, #19315, #12209 ) ),
 .UNSPECIFIED., .F., .F., .F. ) 
 B_SPLINE_SURFACE_WITH_KNOTS ( ( 4, 2, 4 ),
 ( 3, 3 ),
 ( 0.000000000000000000, 0.001526582434089621522, 0.003053164868179243045 ),
 ( 0.000000000000000000, 1.000000000000000000 ),
 .UNSPECIFIED. ) 
 GEOMETRIC_REPRESENTATION_ITEM ( )  RATIONAL_B_SPLINE_SURFACE ( (
 ( 1.000000000000000000, 0.7071067811865483499, 1.000000000000000000),
 ( 1.000000000000000000, 0.7219865977747251806, 1.000000000000000000),
 ( 1.000000000000000000, 0.7353530398653037592, 1.000000000000000000),
 ( 1.000000000000000000, 0.7593109839641446479, 1.000000000000000000),
 ( 1.000000000000000000, 0.7699014431358679467, 1.000000000000000000),
 ( 1.000000000000000000, 0.7791885400064305633, 1.000000000000000000) ) ) 
 REPRESENTATION_ITEM ( '' )  SURFACE ( )  );
#65731 = CARTESIAN_POINT ( 'NONE',  ( -99.54585721581733537, -282.8743313558071009, -315.3067171856280311 ) ) ;
#65732 = CARTESIAN_POINT ( 'NONE',  ( -62.09392073361606634, -274.5247187052497679, -201.5139735104079364 ) ) ;
#65733 = CARTESIAN_POINT ( 'NONE',  ( -94.06769170125781443, -292.8149470727479979, -223.1333081359151151 ) ) ;
#65734 = CARTESIAN_POINT ( 'NONE',  ( -106.3191677418332262, -274.4020936240484048, -237.4868841074855936 ) ) ;
#65735 = CARTESIAN_POINT ( 'NONE',  ( 33.53072730108748800, -274.9869032304191592, -252.7774176564259108 ) ) ;
#65736 = CARTESIAN_POINT ( 'NONE',  ( -71.82837730128250087, -297.5080765006804882, -336.9763073938436264 ) ) ;
#65737 = CARTESIAN_POINT ( 'NONE',  ( -3.058825391129794458, -288.7784952172309545, -339.3227154887462689 ) ) ;
#65738 =( BOUNDED_CURVE ( )  B_SPLINE_CURVE ( 3, ( #69278, #3953, #26661, #10566 ),
 .UNSPECIFIED., .F., .F. ) 
 B_SPLINE_CURVE_WITH_KNOTS ( ( 4, 4 ),
 ( 4.712388980384689674, 6.283185307179586232 ),
 .UNSPECIFIED. ) 
 CURVE ( )  GEOMETRIC_REPRESENTATION_ITEM ( )  RATIONAL_B_SPLINE_CURVE ( ( 1.000000000000000000, 0.8047378541243649375, 0.8047378541243649375, 1.000000000000000000 ) ) 
 REPRESENTATION_ITEM ( '' )  );
#65739 = CARTESIAN_POINT ( 'NONE',  ( 7.707977552399481347, -278.7411913623584496, -209.6343727137316648 ) ) ;
#65740 = CONICAL_SURFACE ( 'NONE', #86850, 4.000000000000003553, 1.029744258676654534 ) ;
#65741 = CARTESIAN_POINT ( 'NONE',  ( -44.89493376068840291, -291.7924912679493445, -193.6795543714625012 ) ) ;
#65742 = CARTESIAN_POINT ( 'NONE',  ( -80.55598004052031058, -288.7127549137894107, -329.5506581157301866 ) ) ;
#65743 = CARTESIAN_POINT ( 'NONE',  ( 0.7316197033791036475, -292.5442274642832103, -334.9786308242219661 ) ) ;
#65744 = ORIENTED_EDGE ( 'NONE', *, *, #88395, .T. ) ;
#65745 = CARTESIAN_POINT ( 'NONE',  ( 197.8641554550088131, 70.83050013377537368, 10.83773308182944106 ) ) ;
#65746 = CARTESIAN_POINT ( 'NONE',  ( -97.40306850759695578, -289.4804311648698558, -311.9838270009958023 ) ) ;
#65747 = DIRECTION ( 'NONE',  ( 0.000000000000000000, 0.000000000000000000, -1.000000000000000000 ) ) ;
#65748 = CARTESIAN_POINT ( 'NONE',  ( -10.08874079242265864, -287.3405109877057271, -198.5403222640659351 ) ) ;
#65749 = CARTESIAN_POINT ( 'NONE',  ( -53.28691492658256834, -291.7662352645559167, -340.3683826091709079 ) ) ;
#65750 = CARTESIAN_POINT ( 'NONE',  ( -3.343807019167917005, -293.6730350296325582, -339.2012783089644472 ) ) ;
#65751 = CARTESIAN_POINT ( 'NONE',  ( -37.29761397685438595, -284.3667421951370216, -346.8809382987477647 ) ) ;
#65752 = CARTESIAN_POINT ( 'NONE',  ( -107.3925195957829999, -284.1131946362799567, -290.9455367621443429 ) ) ;
#65753 = CARTESIAN_POINT ( 'NONE',  ( 36.19254153326932766, -276.8832591651515713, -271.5765208383338063 ) ) ;
#65754 = CARTESIAN_POINT ( 'NONE',  ( 7.020668168854167668, -292.4653329778913644, -330.4574020605629698 ) ) ;
#65755 = CIRCLE ( 'NONE', #12822, 4.999999999999990230 ) ;
#65756 = CARTESIAN_POINT ( 'NONE',  ( 34.76645693901235035, -274.1673948292336149, -256.6664405452803521 ) ) ;
#65757 = ORIENTED_EDGE ( 'NONE', *, *, #87153, .F. ) ;
#65758 = CARTESIAN_POINT ( 'NONE',  ( 202.9738562182569694, 296.4636489450776367, -53.99999999999997868 ) ) ;
#65759 = CARTESIAN_POINT ( 'NONE',  ( 6.598450208492826263, -294.1397526369988213, -333.6321373547042413 ) ) ;
#65760 = CARTESIAN_POINT ( 'NONE',  ( 21.46346364243232685, -288.8418198304104862, -224.7182991022280021 ) ) ;
#65761 = CARTESIAN_POINT ( 'NONE',  ( -114.0566262001358808, -297.6052779302710292, -272.4750473502695058 ) ) ;
#65762 = CARTESIAN_POINT ( 'NONE',  ( 28.89882605107830926, -287.7866190791410759, -239.4404879867815623 ) ) ;
#65763 = CARTESIAN_POINT ( 'NONE',  ( -75.23052950073038403, -276.6031842415533788, -337.1238083256711207 ) ) ;
#65764 = CARTESIAN_POINT ( 'NONE',  ( 17.49468440942154146, -294.9453288962300803, -324.3468227384097986 ) ) ;
#65765 = CARTESIAN_POINT ( 'NONE',  ( -20.78970478231500607, -286.9816053300080512, -344.3495844638194967 ) ) ;
#65766 = CARTESIAN_POINT ( 'NONE',  ( 17.54944698480496612, -294.6272481452900251, -324.4064325299128200 ) ) ;
#65767 = CARTESIAN_POINT ( 'NONE',  ( -64.08330407746979063, -292.0267660864091113, -202.3992612715831854 ) ) ;
#65768 = CARTESIAN_POINT ( 'NONE',  ( 209.7513585654923816, 282.2246705312486483, -40.00000000000000711 ) ) ;
#65769 = LINE ( 'NONE', #9340, #38727 ) ;
#65770 = CARTESIAN_POINT ( 'NONE',  ( 197.1939414079469941, 281.6276418468785323, -110.3312364698208228 ) ) ;
#65771 = CARTESIAN_POINT ( 'NONE',  ( 38.88388837170287360, -289.0152164241742980, -265.8400043962846553 ) ) ;
#65772 = CARTESIAN_POINT ( 'NONE',  ( -115.3288506153726871, -282.2666405000203440, -252.5284128619063608 ) ) ;
#65773 = VERTEX_POINT ( 'NONE', #63938 ) ;
#65774 = CARTESIAN_POINT ( 'NONE',  ( -42.41503485917646543, -279.3383343500467504, -193.6305891080372987 ) ) ;
#65775 = CARTESIAN_POINT ( 'NONE',  ( 20.79197628991754954, -284.2028694440267600, -317.5035491278106292 ) ) ;
#65776 = CARTESIAN_POINT ( 'NONE',  ( -82.90982830526120040, -284.0175113988842099, -208.9587649944826637 ) ) ;
#65777 = CARTESIAN_POINT ( 'NONE',  ( 23.92137006911448793, -286.2098281693962463, -312.6701039471620902 ) ) ;
#65778 = CARTESIAN_POINT ( 'NONE',  ( -18.87435577062038305, -276.1477190557915833, -196.8272996567008022 ) ) ;
#65779 = CARTESIAN_POINT ( 'NONE',  ( -37.82921519546573563, -298.5382312439015209, -197.3012057807513315 ) ) ;
#65780 = CARTESIAN_POINT ( 'NONE',  ( 1.818531145371408364, -293.2015125376300944, -332.6123761224383202 ) ) ;
#65781 = CARTESIAN_POINT ( 'NONE',  ( -56.53923668610484299, -280.4625498478460486, -195.8429940424889537 ) ) ;
#65783 = CARTESIAN_POINT ( 'NONE',  ( -110.4939669181725606, -277.8971905212325169, -270.6301615191002838 ) ) ;
#65782 = CARTESIAN_POINT ( 'NONE',  ( 25.37557032388277634, -276.0657500860480695, -307.7180984153411600 ) ) ;
#65784 = CARTESIAN_POINT ( 'NONE',  ( -55.27472808253266834, -274.9063457531331665, -195.7963875984286517 ) ) ;
#65785 = CARTESIAN_POINT ( 'NONE',  ( -2.876395262564094057, -275.5277549784264011, -338.8858466805365310 ) ) ;
#65786 = CARTESIAN_POINT ( 'NONE',  ( 173.6393091185710489, 243.4999469643735210, -179.6212980619924622 ) ) ;
#65787 = CARTESIAN_POINT ( 'NONE',  ( 16.76155902123706198, -274.2824089246178687, -322.3749276737877949 ) ) ;
#65788 = CARTESIAN_POINT ( 'NONE',  ( -112.0284649023453198, -298.1815470323154500, -254.1601685751500668 ) ) ;
#65789 = CARTESIAN_POINT ( 'NONE',  ( 39.58706461736021254, -278.0519495502701943, -270.3284710469133074 ) ) ;
#65790 = CARTESIAN_POINT ( 'NONE',  ( -92.83893396777953910, -239.1568807800618686, -338.3566629249717153 ) ) ;
#65791 = CARTESIAN_POINT ( 'NONE',  ( -94.37114856999372137, -286.2807001801144793, -224.2774780387568114 ) ) ;
#65792 = CARTESIAN_POINT ( 'NONE',  ( -13.04916144716970194, -288.1236820990559409, -198.3621834290005097 ) ) ;
#65793 = CARTESIAN_POINT ( 'NONE',  ( -39.96928640252048126, -285.3668521753272103, -197.3064230012119538 ) ) ;
#65794 = CARTESIAN_POINT ( 'NONE',  ( -108.9532641653668037, -276.7185518354165765, -288.2521160139815493 ) ) ;
#65795 = CARTESIAN_POINT ( 'NONE',  ( -109.5727850814231488, -286.6354750945367869, -253.1734081941833665 ) ) ;
#65796 = CARTESIAN_POINT ( 'NONE',  ( -110.3055038760450799, -277.1718095932899359, -259.6640377211767259 ) ) ;
#65797 = CARTESIAN_POINT ( 'NONE',  ( 24.25153651951646694, -277.1809694172739569, -310.2102383099570488 ) ) ;
#65798 = CARTESIAN_POINT ( 'NONE',  ( 23.09971970921002793, -275.4738785465905266, -229.2920820922656446 ) ) ;
#65799 = CARTESIAN_POINT ( 'NONE',  ( 39.30493128313072049, -286.3621550812214878, -271.5604674432495358 ) ) ;
#65800 = CARTESIAN_POINT ( 'NONE',  ( 37.98926664671574116, -282.5448017530379730, -285.5072153618228867 ) ) ;
#65801 = CARTESIAN_POINT ( 'NONE',  ( -50.07714253274934180, -283.7027095863974182, -346.2920567947306267 ) ) ;
#65802 = VERTEX_POINT ( 'NONE', #92776 ) ;
#65803 = ORIENTED_EDGE ( 'NONE', *, *, #42272, .F. ) ;
#65804 = CARTESIAN_POINT ( 'NONE',  ( 197.1285099842352508, 19.08195175179129066, -12.05325424581438121 ) ) ;
#65805 = CARTESIAN_POINT ( 'NONE',  ( -72.57804810807863305, -291.3739294491061855, -337.4480240295351336 ) ) ;
#65806 = CARTESIAN_POINT ( 'NONE',  ( -113.5141541007331085, -289.3337913093113798, -262.6697758023958045 ) ) ;
#65807 = AXIS2_PLACEMENT_3D ( 'NONE', #53981, #83312, #82850 ) ;
#65808 = CARTESIAN_POINT ( 'NONE',  ( -108.7517081852593464, -295.5398667591188655, -286.2737694533433910 ) ) ;
#65809 = CARTESIAN_POINT ( 'NONE',  ( -42.03943701922745646, -291.3429867301673539, -193.6066780146360600 ) ) ;
#65810 = CARTESIAN_POINT ( 'NONE',  ( 19.20612184350011375, -285.3674413547179256, -223.0862767112967333 ) ) ;
#65811 = EDGE_CURVE ( 'NONE', #89245, #46265, #86594, .T. ) ;
#65812 = CARTESIAN_POINT ( 'NONE',  ( 34.38077034015644529, -288.5526976312329452, -254.7720918403955750 ) ) ;
#65813 = CARTESIAN_POINT ( 'NONE',  ( -37.30987171927208124, -297.5519495502701943, -345.3611179825600175 ) ) ;
#65814 = CARTESIAN_POINT ( 'NONE',  ( -40.23541020264898549, -291.0886579432597614, -345.3180200138587566 ) ) ;
#65815 = CARTESIAN_POINT ( 'NONE',  ( -92.27090468178320748, -287.8345793505854431, -321.7470851548818018 ) ) ;
#65816 = AXIS2_PLACEMENT_3D ( 'NONE', #43605, #22301, #1000 ) ;
#65817 = CARTESIAN_POINT ( 'NONE',  ( -100.6623538141222696, -292.0104403931363777, -310.6489867038565649 ) ) ;
#65818 = CARTESIAN_POINT ( 'NONE',  ( -109.1620598710921115, -285.6817880712897590, -256.0347655112273060 ) ) ;
#65819 = CARTESIAN_POINT ( 'NONE',  ( -93.36237009153266797, -293.2486548185485162, -220.2441252074445686 ) ) ;
#65820 = CARTESIAN_POINT ( 'NONE',  ( 82.15113745099867515, -299.3754171896197818, -193.3637965294381900 ) ) ;
#65821 = EDGE_CURVE ( 'NONE', #3069, #80198, #22411, .T. ) ;
#65822 = FACE_OUTER_BOUND ( 'NONE', #51193, .T. ) ;
#65823 = CARTESIAN_POINT ( 'NONE',  ( -30.66838526091325789, -300.0552191073463177, -194.7989468035448510 ) ) ;
#65824 = VECTOR ( 'NONE', #42448, 1000.000000000000000 ) ;
#65825 = CARTESIAN_POINT ( 'NONE',  ( 1.177652195100557853, -281.7210041291835410, -332.6204407054860894 ) ) ;
#65826 = CARTESIAN_POINT ( 'NONE',  ( -81.83249319231074992, -281.6575907635549356, -330.8043033774057449 ) ) ;
#65827 = CARTESIAN_POINT ( 'NONE',  ( 35.33034868849125587, -293.0663844995115710, -295.4827128101073868 ) ) ;
#65828 = CARTESIAN_POINT ( 'NONE',  ( -69.91703860872395637, -271.8569159029796651, -203.9019475137396853 ) ) ;
#65829 = CARTESIAN_POINT ( 'NONE',  ( 25.18081956565028889, -274.1816276034521138, -310.8572134494829697 ) ) ;
#65830 = CARTESIAN_POINT ( 'NONE',  ( -75.48079136813949219, -298.8474813595877322, -207.4797142714373024 ) ) ;
#65831 = CARTESIAN_POINT ( 'NONE',  ( 194.7510731661265595, -143.7221692137691775, 22.50000000000000000 ) ) ;
#65832 = CARTESIAN_POINT ( 'NONE',  ( -112.7661943181041124, -294.9089359349839583, -261.1350847545549527 ) ) ;
#65833 = CARTESIAN_POINT ( 'NONE',  ( 26.31135669083326079, -295.4799752652416487, -307.2889296374409582 ) ) ;
#65834 = CARTESIAN_POINT ( 'NONE',  ( 160.5350683151633291, 250.0000000000000568, 20.22542485937379908 ) ) ;
#65835 = CARTESIAN_POINT ( 'NONE',  ( -92.30524410099367572, -296.6671932431084429, -318.6478714582084422 ) ) ;
#65836 = CARTESIAN_POINT ( 'NONE',  ( 151.0889892289287388, 131.0000000000000284, 11.50000000000000000 ) ) ;
#65838 = CARTESIAN_POINT ( 'NONE',  ( -94.45132050873985463, -297.1942678994180937, -224.8914439131643803 ) ) ;
#65837 = CARTESIAN_POINT ( 'NONE',  ( -111.8570138474588305, -282.7200249352006836, -258.7983972988339474 ) ) ;
#65839 = CARTESIAN_POINT ( 'NONE',  ( -104.4170152507197571, -284.0602523342612926, -308.2831568665051236 ) ) ;
#65840 = CARTESIAN_POINT ( 'NONE',  ( 21.41915046918228072, -284.1215632595194052, -317.8839265780024448 ) ) ;
#65841 = CARTESIAN_POINT ( 'NONE',  ( 14.23586249001719573, -286.4199161249086956, -213.1450519873649512 ) ) ;
#65842 = CARTESIAN_POINT ( 'NONE',  ( 37.12225008550011296, -291.4499572032673882, -262.4323633119647639 ) ) ;
#65843 = CARTESIAN_POINT ( 'NONE',  ( -103.2677838921256210, -278.2662545243572367, -230.7873124337938009 ) ) ;
#65844 = CARTESIAN_POINT ( 'NONE',  ( 10.59707575819633618, -279.9094976428775681, -330.5268031993606428 ) ) ;
#65845 = CARTESIAN_POINT ( 'NONE',  ( -48.18343439339133027, -274.0850372458094171, -506.3822550525310362 ) ) ;
#65846 = CARTESIAN_POINT ( 'NONE',  ( 4.966710597622522982, -285.4327853263189922, -210.3228458875806268 ) ) ;
#65847 = CARTESIAN_POINT ( 'NONE',  ( -73.04221787564945600, -288.4343173699147087, -338.2504473885968537 ) ) ;
#65848 = DIRECTION ( 'NONE',  ( -1.000000000000000000, -0.000000000000000000, -0.000000000000000000 ) ) ;
#65849 = CARTESIAN_POINT ( 'NONE',  ( -88.80179633647965431, -279.1834931639543242, -326.8453174527124929 ) ) ;
#65851 = CARTESIAN_POINT ( 'NONE',  ( 34.50549055392714592, -281.3917765261786030, -283.4721980409929643 ) ) ;
#65850 = CARTESIAN_POINT ( 'NONE',  ( -39.09538557066380093, -293.0941708233737018, -345.6959133537567936 ) ) ;
#65852 = CARTESIAN_POINT ( 'NONE',  ( 29.57572045997232735, -294.2147258880775098, -308.5615993393387271 ) ) ;
#65853 = CARTESIAN_POINT ( 'NONE',  ( 2.012281269467944611, -284.6544373614743222, -205.8585727185341341 ) ) ;
#65854 = CARTESIAN_POINT ( 'NONE',  ( -93.48208219091732474, -281.2440130118706065, -220.6292554365479646 ) ) ;
#65855 = CARTESIAN_POINT ( 'NONE',  ( -107.6820329705125232, -295.8796896351516921, -249.9737193238597683 ) ) ;
#65856 = VERTEX_POINT ( 'NONE', #64880 ) ;
#65857 = CARTESIAN_POINT ( 'NONE',  ( 156.5440870305766055, 215.0000000000000568, 17.21343741151179429 ) ) ;
#65858 = CARTESIAN_POINT ( 'NONE',  ( 35.94439541251172443, -283.3482763720529647, -256.1166257135086539 ) ) ;
#65859 = CARTESIAN_POINT ( 'NONE',  ( 210.8848006936870263, 293.9636489450776367, -54.00000000000000000 ) ) ;
#65860 = CARTESIAN_POINT ( 'NONE',  ( -85.33152481854864391, -281.1952119285918457, -330.4860931364850671 ) ) ;
#65861 = CARTESIAN_POINT ( 'NONE',  ( -2.621342065655723363, -273.6966477828996744, -201.7997052641869686 ) ) ;
#65862 = CARTESIAN_POINT ( 'NONE',  ( -107.7263773463444920, -290.1273863138068236, -289.9122635209611190 ) ) ;
#65863 = CARTESIAN_POINT ( 'NONE',  ( -81.72070101549196863, -280.9558767872229055, -211.4649633205696944 ) ) ;
#65864 = CARTESIAN_POINT ( 'NONE',  ( -90.78989565143865548, -274.8783297375145480, -219.4532258195929160 ) ) ;
#65865 = CARTESIAN_POINT ( 'NONE',  ( -67.54531942401760602, -285.0419614023305712, -340.3195470548292292 ) ) ;
#65866 = CARTESIAN_POINT ( 'NONE',  ( 24.45652004839766036, -280.8930520690052504, -310.0538963542088595 ) ) ;
#65867 = CARTESIAN_POINT ( 'NONE',  ( -72.57172559098098930, -279.5186622458451779, -336.5862199601089060 ) ) ;
#65868 = ORIENTED_EDGE ( 'NONE', *, *, #66040, .F. ) ;
#65869 = CARTESIAN_POINT ( 'NONE',  ( -15.77532429850858620, -274.1568500131879773, -196.3876383848830471 ) ) ;
#65870 = CARTESIAN_POINT ( 'NONE',  ( 26.06180387523198050, -294.9438736946376025, -231.2593390296383973 ) ) ;
#65871 = DIRECTION ( 'NONE',  ( 0.000000000000000000, 0.000000000000000000, -1.000000000000000000 ) ) ;
#65872 = CARTESIAN_POINT ( 'NONE',  ( 14.61415361889143760, -292.4695821745240210, -325.5054263021999645 ) ) ;
#65873 = CARTESIAN_POINT ( 'NONE',  ( -2.879096943440680345, -274.0283724233834732, -205.9381607116308146 ) ) ;
#65874 = DIRECTION ( 'NONE',  ( 1.000000000000000000, 0.000000000000000000, 0.000000000000000000 ) ) ;
#65875 = CARTESIAN_POINT ( 'NONE',  ( 33.80926092852174492, -294.7181304391621097, -242.6425893817074950 ) ) ;
#65877 = CARTESIAN_POINT ( 'NONE',  ( 8.600460027102576177, -293.8706629469612608, -208.9978884705523967 ) ) ;
#65876 = CARTESIAN_POINT ( 'NONE',  ( 39.58706461736021254, -284.0519495502703080, -270.3284710469133074 ) ) ;
#65878 = CARTESIAN_POINT ( 'NONE',  ( -12.65975566729633428, -290.7306689656015237, -341.0069249568863938 ) ) ;
#65879 = CARTESIAN_POINT ( 'NONE',  ( 35.00833566613925285, -273.7982598874033897, -289.4791918884091615 ) ) ;
#65880 = CARTESIAN_POINT ( 'NONE',  ( -68.62066859927622886, -279.3865951612418712, -337.9246740013025487 ) ) ;
#65881 = CARTESIAN_POINT ( 'NONE',  ( 19.92554231376057672, -292.2935245048903425, -317.9192628601773549 ) ) ;
#65882 = CARTESIAN_POINT ( 'NONE',  ( -109.3827079970369738, -280.7144166943138544, -246.7338633729383446 ) ) ;
#65883 = AXIS2_PLACEMENT_3D ( 'NONE', #72741, #88329, #81226 ) ;
#65884 = ORIENTED_EDGE ( 'NONE', *, *, #793, .F. ) ;
#65885 = CARTESIAN_POINT ( 'NONE',  ( -80.64208556750783430, -283.3242018049514854, -329.2216841063703896 ) ) ;
#65886 = CARTESIAN_POINT ( 'NONE',  ( -94.73960930164052741, -280.3236726324363417, -219.4988280940565915 ) ) ;
#65887 = CARTESIAN_POINT ( 'NONE',  ( -31.68102171690648206, -281.7771537337149539, -346.7678083002064113 ) ) ;
#65888 = CARTESIAN_POINT ( 'NONE',  ( -42.77750913042631709, -278.0604198057099552, -346.9331245745490264 ) ) ;
#65889 = CARTESIAN_POINT ( 'NONE',  ( 35.91472517847984847, -276.7998691822635351, -248.8177041494605533 ) ) ;
#65890 = CARTESIAN_POINT ( 'NONE',  ( -82.13390479932378696, -293.9090924074131408, -214.2458315076590907 ) ) ;
#65891 = VERTEX_POINT ( 'NONE', #66701 ) ;
#65892 = CARTESIAN_POINT ( 'NONE',  ( -63.80845765909949563, -299.7073753037106485, -200.1313016257661843 ) ) ;
#65893 = CARTESIAN_POINT ( 'NONE',  ( -29.56662005178704788, -274.9734487608597533, -344.6519395095928644 ) ) ;
#65894 = CARTESIAN_POINT ( 'NONE',  ( -107.4410674961157497, -292.6902660290031122, -241.0344627663689892 ) ) ;
#65895 = CARTESIAN_POINT ( 'NONE',  ( 14.95422200761641562, -292.1620778603046915, -219.2099503084498622 ) ) ;
#65896 = CARTESIAN_POINT ( 'NONE',  ( 18.59576727346057723, -287.7818032554592946, -323.1865535597679582 ) ) ;
#65897 = DIRECTION ( 'NONE',  ( 0.000000000000000000, 0.000000000000000000, 1.000000000000000000 ) ) ;
#65899 = CARTESIAN_POINT ( 'NONE',  ( -94.92185217541755549, -282.3065766172842928, -316.5436213277922661 ) ) ;
#65898 = CARTESIAN_POINT ( 'NONE',  ( 37.74957912682096151, -291.9486960904557122, -256.2223035354735998 ) ) ;
#65900 = CARTESIAN_POINT ( 'NONE',  ( -111.5397449963474230, -292.3654667848398958, -273.9926129638059251 ) ) ;
#65901 = CARTESIAN_POINT ( 'NONE',  ( -92.02279969251297587, -283.7336356121102767, -220.8828702972186875 ) ) ;
#65902 = CARTESIAN_POINT ( 'NONE',  ( -4.592467130376145512, -283.9264818236449059, -336.1542119788002765 ) ) ;
#65903 = CARTESIAN_POINT ( 'NONE',  ( -15.00921045676239629, -289.7111584425884416, -343.8611031199193917 ) ) ;
#65904 = CARTESIAN_POINT ( 'NONE',  ( -14.29540576429860188, -280.8514322604997915, -200.9761362627264702 ) ) ;
#65905 = CARTESIAN_POINT ( 'NONE',  ( 19.13335302357579337, -291.6393496880280054, -218.6061463346869402 ) ) ;
#65906 = CARTESIAN_POINT ( 'NONE',  ( 22.85898160912359955, -287.7144297596924503, -222.5904200343319133 ) ) ;
#65907 = CARTESIAN_POINT ( 'NONE',  ( 36.63031377635126518, -287.7769118219187590, -249.0138320403187322 ) ) ;
#65908 = CARTESIAN_POINT ( 'NONE',  ( -95.76721665583242782, -285.3331676562137318, -226.5951606299279888 ) ) ;
#65909 = ORIENTED_EDGE ( 'NONE', *, *, #22374, .T. ) ;
#65910 = ADVANCED_FACE ( 'NONE', ( #16967 ), #37794, .F. ) ;
#65911 = DIRECTION ( 'NONE',  ( 0.000000000000000000, 0.000000000000000000, 1.000000000000000000 ) ) ;
#65912 = CARTESIAN_POINT ( 'NONE',  ( 37.99520844272763043, -295.3042731890324148, -261.8409060735369280 ) ) ;
#65913 = CARTESIAN_POINT ( 'NONE',  ( -34.88734675084126025, -293.7067547396778195, -346.8285909597219074 ) ) ;
#65914 = CARTESIAN_POINT ( 'NONE',  ( -106.4903298721224303, -277.2892350638995254, -294.6370839284992371 ) ) ;
#65915 = ADVANCED_FACE ( 'NONE', ( #52479 ), #43304, .T. ) ;
#65916 = CARTESIAN_POINT ( 'NONE',  ( -30.48752868040909192, -297.4844462213418979, -193.4637846374093613 ) ) ;
#65917 = CARTESIAN_POINT ( 'NONE',  ( 25.44867885469276558, -291.5041519684930904, -231.6886148249389237 ) ) ;
#65918 = CARTESIAN_POINT ( 'NONE',  ( -19.04246480916356887, -276.0509228699447135, -198.5924736606033321 ) ) ;
#65919 = CARTESIAN_POINT ( 'NONE',  ( -110.7381659365240409, -294.9211031748773735, -260.4389765355931559 ) ) ;
#65920 = CARTESIAN_POINT ( 'NONE',  ( 22.90513883822377039, -294.1758070528954931, -228.4170414593597798 ) ) ;
#65921 = CARTESIAN_POINT ( 'NONE',  ( 28.67889141215444226, -295.0626537967168019, -302.3452616740846679 ) ) ;
#65922 = CARTESIAN_POINT ( 'NONE',  ( -43.45429243013615661, -257.5024557858946537, -441.6962169675167047 ) ) ;
#65923 = CARTESIAN_POINT ( 'NONE',  ( -44.64350477871803946, -293.1440563137820732, -345.2244300709161848 ) ) ;
#65924 = CARTESIAN_POINT ( 'NONE',  ( -35.76203819307012566, -300.0720829547246353, -195.3605707076006013 ) ) ;
#65925 = CARTESIAN_POINT ( 'NONE',  ( -39.95440870581483495, -290.0269077196645071, -343.5995299415985187 ) ) ;
#65926 = CARTESIAN_POINT ( 'NONE',  ( -72.13091536240513335, -295.8589809509435895, -334.5766211629199915 ) ) ;
#65927 = CARTESIAN_POINT ( 'NONE',  ( -88.08550981830383364, -279.7380237565122911, -326.0699375581911568 ) ) ;
#65928 = CARTESIAN_POINT ( 'NONE',  ( -112.8154426446185852, -277.0792615340583893, -282.8915794164530553 ) ) ;
#65929 = CARTESIAN_POINT ( 'NONE',  ( 7.182734913916002384, -273.9894863080115215, -207.5989751464046549 ) ) ;
#65930 = CARTESIAN_POINT ( 'NONE',  ( -21.09733145479795624, -280.9221035006244733, -343.0601076353809162 ) ) ;
#65931 = CARTESIAN_POINT ( 'NONE',  ( -113.4110265899463599, -277.0083979453259531, -265.9004021971235261 ) ) ;
#65932 = CARTESIAN_POINT ( 'NONE',  ( -33.97136655586751885, -278.0943049750007958, -195.2700447427622237 ) ) ;
#65933 = EDGE_CURVE ( 'NONE', #12065, #47975, #44313, .T. ) ;
#65934 = CARTESIAN_POINT ( 'NONE',  ( -40.52266495658383860, -296.6961748250478763, -196.9242040062792967 ) ) ;
#65935 = CARTESIAN_POINT ( 'NONE',  ( -41.79599345211435235, -275.9963199119455339, -195.4430843555014405 ) ) ;
#65936 = DIRECTION ( 'NONE',  ( -0.3024135303179549816, -0.9531768234071953394, 0.000000000000000000 ) ) ;
#65937 = CARTESIAN_POINT ( 'NONE',  ( -87.53473460053250221, -289.3757413580710818, -214.1555480570359578 ) ) ;
#65938 = CARTESIAN_POINT ( 'NONE',  ( -106.5135117000522911, -290.1164061756080628, -304.3092349933458536 ) ) ;
#65939 = CARTESIAN_POINT ( 'NONE',  ( -21.76028743816657141, -276.2515857240513242, -196.8271258288489776 ) ) ;
#65940 = CARTESIAN_POINT ( 'NONE',  ( -108.1874836982243124, -270.8706271185409946, -245.7465776028672337 ) ) ;
#65941 = CARTESIAN_POINT ( 'NONE',  ( -108.0824881141068374, -283.3651533450540114, -300.4956054416641109 ) ) ;
#65942 = DIRECTION ( 'NONE',  ( 0.000000000000000000, 1.000000000000000000, 0.000000000000000000 ) ) ;
#65943 = CARTESIAN_POINT ( 'NONE',  ( 21.18455266390713021, -280.1972415876811056, -317.2819622906920358 ) ) ;
#65944 = DIRECTION ( 'NONE',  ( 0.000000000000000000, 1.000000000000000000, 0.000000000000000000 ) ) ;
#65945 = CARTESIAN_POINT ( 'NONE',  ( -49.74078322464380619, -290.6855396640504523, -197.9673190511191763 ) ) ;
#65946 = CARTESIAN_POINT ( 'NONE',  ( -24.91206906884427852, -284.3518004266574053, -197.1217259765511756 ) ) ;
#65947 = CARTESIAN_POINT ( 'NONE',  ( 195.1467215189997546, 26.67165171595035389, 15.11006648940266039 ) ) ;
#65948 = DIRECTION ( 'NONE',  ( 0.000000000000000000, -1.000000000000000000, 0.000000000000000000 ) ) ;
#65949 = CARTESIAN_POINT ( 'NONE',  ( 36.18203819356016027, -291.3618678629532610, -255.5536686649602700 ) ) ;
#65950 = CARTESIAN_POINT ( 'NONE',  ( -59.41507680527886492, -278.9429034422712448, -340.7827514188816167 ) ) ;
#65951 = CARTESIAN_POINT ( 'NONE',  ( -13.53071806803214194, -283.9547827405726252, -343.1693994564748209 ) ) ;
#65953 = CARTESIAN_POINT ( 'NONE',  ( -22.45983557658234986, -286.2478943656337833, -198.8422511808585398 ) ) ;
#65952 = CARTESIAN_POINT ( 'NONE',  ( -3.394394904562281212, -274.6874083083788491, -337.8802947113563278 ) ) ;
#65954 = CARTESIAN_POINT ( 'NONE',  ( 21.31750813661597732, -277.5968364044633745, -314.7961515080252752 ) ) ;
#65955 = CARTESIAN_POINT ( 'NONE',  ( -71.72104108337192940, -278.3215278409545022, -334.9559156926094374 ) ) ;
#65956 = CARTESIAN_POINT ( 'NONE',  ( -75.12186625607682799, -287.5493480374124715, -205.5119532044941195 ) ) ;
#65957 = VERTEX_POINT ( 'NONE', #9381 ) ;
#65958 = DIRECTION ( 'NONE',  ( 1.000000000000000000, 0.000000000000000000, 0.000000000000000000 ) ) ;
#65959 = CARTESIAN_POINT ( 'NONE',  ( -81.87343011763827860, -295.4734290814205906, -333.2428401687030259 ) ) ;
#65960 = CARTESIAN_POINT ( 'NONE',  ( -51.02886567050759936, -291.2076823765269751, -343.7931668184233445 ) ) ;
#65961 = CARTESIAN_POINT ( 'NONE',  ( 196.7510731661265595, -143.7221692137691775, -32.50000000000000711 ) ) ;
#65962 = CARTESIAN_POINT ( 'NONE',  ( -55.63300648810263738, -276.3376638359844719, -190.3683826091709363 ) ) ;
#65963 = CARTESIAN_POINT ( 'NONE',  ( -109.3113213907166568, -277.8104039890518493, -243.7151196863976850 ) ) ;
#65964 = CARTESIAN_POINT ( 'NONE',  ( 38.85679907281704715, -291.9157062107698266, -267.4873151123534853 ) ) ;
#65965 = CARTESIAN_POINT ( 'NONE',  ( 24.10154053994182988, -288.5119644990451206, -229.5817167905381666 ) ) ;
#65966 = CARTESIAN_POINT ( 'NONE',  ( -110.0343559269828120, -280.1303189486744714, -284.3474544559434207 ) ) ;
#65967 = CARTESIAN_POINT ( 'NONE',  ( 22.83473592384047990, -289.6118616578893352, -317.4714989777941128 ) ) ;
#65968 = CARTESIAN_POINT ( 'NONE',  ( -54.11278054615037547, -285.2675302830276109, -343.5154558611239963 ) ) ;
#65969 = CARTESIAN_POINT ( 'NONE',  ( -114.0441001613910288, -278.8106921386081467, -263.0160367791310705 ) ) ;
#65970 = CARTESIAN_POINT ( 'NONE',  ( -95.17950200455065612, -271.2084113306615905, -222.8561745852593390 ) ) ;
#65971 = CARTESIAN_POINT ( 'NONE',  ( -67.36050189434993740, -279.5025040208689120, -199.4536321645202861 ) ) ;
#65972 = CARTESIAN_POINT ( 'NONE',  ( -111.4231494417489756, -274.4841323063036498, -264.8448713526778420 ) ) ;
#65973 = CARTESIAN_POINT ( 'NONE',  ( 2.197429475817664013, -229.5268262511776527, 22.50000000000000000 ) ) ;
#65974 = CARTESIAN_POINT ( 'NONE',  ( -106.6379572354042296, -292.6233781216987495, -303.7686719486574702 ) ) ;
#65975 = CARTESIAN_POINT ( 'NONE',  ( -4.246915530093622770, -272.7222692138797697, -201.9457069542743568 ) ) ;
#65976 = FACE_OUTER_BOUND ( 'NONE', #13779, .T. ) ;
#65977 = CARTESIAN_POINT ( 'NONE',  ( -91.33807603188630253, -278.7649825298331621, -221.1434399492984255 ) ) ;
#65978 = CARTESIAN_POINT ( 'NONE',  ( 38.74506690713576518, -276.8744282527746918, -279.6842598408074423 ) ) ;
#65979 = CARTESIAN_POINT ( 'NONE',  ( 95.73017409340855011, -301.1753302961462282, -196.7389390362352231 ) ) ;
#65980 = CARTESIAN_POINT ( 'NONE',  ( -50.06634564565337087, -282.2693411840519957, -346.1175613297530163 ) ) ;
#65981 = CARTESIAN_POINT ( 'NONE',  ( 35.28277365933605836, -289.4988292765806932, -284.6976763241843855 ) ) ;
#65982 = CARTESIAN_POINT ( 'NONE',  ( -43.25551352050557341, -299.4990130816950114, -194.2312246572168135 ) ) ;
#65983 = CARTESIAN_POINT ( 'NONE',  ( -103.5145756664146290, -298.2631219816349812, -231.6669218888956721 ) ) ;
#65984 = CARTESIAN_POINT ( 'NONE',  ( -34.19934104096697070, -297.0126997540321554, -345.1284504759887000 ) ) ;
#65985 = CARTESIAN_POINT ( 'NONE',  ( 32.79733761175518225, -279.2108490636829288, -244.1250818987050764 ) ) ;
#65986 = CARTESIAN_POINT ( 'NONE',  ( -99.19224125675204107, -271.1414247475190678, -228.4795093348032822 ) ) ;
#65987 = CARTESIAN_POINT ( 'NONE',  ( 33.11189621951743334, -288.7779186230117148, -241.1935299996296749 ) ) ;
#65988 = CARTESIAN_POINT ( 'NONE',  ( 1.463601776810747435, -287.4404803334741700, -332.5573768527789298 ) ) ;
#65989 = CARTESIAN_POINT ( 'NONE',  ( 123.0373869404028113, 148.7393932779486079, -263.4038933679887577 ) ) ;
#65990 = ORIENTED_EDGE ( 'NONE', *, *, #73681, .F. ) ;
#65991 = CARTESIAN_POINT ( 'NONE',  ( -2.088830972431062971, -287.1693679847561498, -338.1537540920544984 ) ) ;
#65992 = CARTESIAN_POINT ( 'NONE',  ( -66.34133048055761606, -289.1091883054617142, -337.4308879379889277 ) ) ;
#65993 = EDGE_LOOP ( 'NONE', ( #15740, #53740, #5309, #76183 ) ) ;
#65994 = CARTESIAN_POINT ( 'NONE',  ( -70.94324956237295510, -286.6988010066888251, -201.4232591024590135 ) ) ;
#65995 = CARTESIAN_POINT ( 'NONE',  ( -16.37073773745650129, -277.1069362282830753, -340.3591661227330292 ) ) ;
#65996 = CARTESIAN_POINT ( 'NONE',  ( 8.676474224327343165, -291.5862835011914740, -208.9448498506494616 ) ) ;
#65997 = CARTESIAN_POINT ( 'NONE',  ( -16.16193853528575630, -283.4368465355158264, -344.3401479676193730 ) ) ;
#65998 = CARTESIAN_POINT ( 'NONE',  ( 30.46993938637740484, -283.5273767765294792, -305.3509636138021506 ) ) ;
#65999 = CARTESIAN_POINT ( 'NONE',  ( 2.086954024954835507, -282.8726163968291303, -336.4756059801734978 ) ) ;
#66000 = CARTESIAN_POINT ( 'NONE',  ( 20.53008303935344969, -281.2586714350285320, -225.8105357819634662 ) ) ;
#66001 = CARTESIAN_POINT ( 'NONE',  ( 65.15629269179825656, 47.80519856837923243, -319.0222192987535550 ) ) ;
#66002 = CARTESIAN_POINT ( 'NONE',  ( -54.34637575705281876, -279.2711085221470739, -343.2902765430991963 ) ) ;
#66003 = CARTESIAN_POINT ( 'NONE',  ( 166.9140850792291531, 232.6971882099037146, -192.2382519929172418 ) ) ;
#66004 = CARTESIAN_POINT ( 'NONE',  ( -77.96030328704325996, -207.4903925274613243, -353.7115950856197628 ) ) ;
#66005 = CARTESIAN_POINT ( 'NONE',  ( -102.1687970221487234, -272.2111267290140404, -236.3390446985912661 ) ) ;
#66006 = CARTESIAN_POINT ( 'NONE',  ( 37.70267676728949624, -292.8467791220786580, -253.3353416622107090 ) ) ;
#66007 = CARTESIAN_POINT ( 'NONE',  ( 168.1374001855827771, 229.6528827650084850, -190.0556063141613663 ) ) ;
#66009 = CARTESIAN_POINT ( 'NONE',  ( -20.97148885136189733, -287.2384240427127793, -342.3226118230091970 ) ) ;
#66008 = CARTESIAN_POINT ( 'NONE',  ( 6.963136212523474811, -273.3258323534875558, -207.9231837627890229 ) ) ;
#66010 = CARTESIAN_POINT ( 'NONE',  ( -10.01361473381519929, -296.5519072661414839, -339.3831523595944759 ) ) ;
#66011 = CARTESIAN_POINT ( 'NONE',  ( 33.86221415781191979, -288.6281075565840410, -252.1102026907373670 ) ) ;
#66012 = ORIENTED_EDGE ( 'NONE', *, *, #72819, .F. ) ;
#66013 = CARTESIAN_POINT ( 'NONE',  ( -19.33081930196000187, -295.7672974475588035, -345.0377406702301073 ) ) ;
#66014 = CARTESIAN_POINT ( 'NONE',  ( -41.33255420213366449, -286.4929353506379357, -197.3961484234209820 ) ) ;
#66015 = CARTESIAN_POINT ( 'NONE',  ( -34.10243567483509963, -273.0123313599640937, -193.7386690775432498 ) ) ;
#66016 = CARTESIAN_POINT ( 'NONE',  ( -27.75781637311466810, -295.7363576475738682, -346.6527932587918599 ) ) ;
#66017 = CARTESIAN_POINT ( 'NONE',  ( 32.12770106494478739, -293.6188855934028084, -237.1687736219842293 ) ) ;
#66018 = CARTESIAN_POINT ( 'NONE',  ( -107.3958945317856148, -290.9909506204559193, -249.7884584224612183 ) ) ;
#66019 = ORIENTED_EDGE ( 'NONE', *, *, #16970, .F. ) ;
#66020 = CARTESIAN_POINT ( 'NONE',  ( -55.02086467013484850, -275.7466931561976935, -196.8984653198138801 ) ) ;
#66021 = CARTESIAN_POINT ( 'NONE',  ( -0.2243317157130767237, -273.3294074106844960, -203.3364276961902135 ) ) ;
#66022 = ORIENTED_EDGE ( 'NONE', *, *, #72919, .T. ) ;
#66023 = EDGE_CURVE ( 'NONE', #16112, #5855, #77773, .T. ) ;
#66024 = CARTESIAN_POINT ( 'NONE',  ( -99.37453220276103139, -278.6649973889156513, -224.8256493548919082 ) ) ;
#66025 = CARTESIAN_POINT ( 'NONE',  ( -33.75048651690141099, -296.5777826597361013, -196.6687291552181591 ) ) ;
#66026 = CARTESIAN_POINT ( 'NONE',  ( -68.57837650279431330, -275.6066369441006145, -337.7185155995596233 ) ) ;
#66027 = CARTESIAN_POINT ( 'NONE',  ( -38.09929201648341035, -275.1221121905756490, -197.0559194685275202 ) ) ;
#66028 = CARTESIAN_POINT ( 'NONE',  ( -62.12054311311919008, -274.6631157985659115, -201.4451010611083746 ) ) ;
#66029 = CARTESIAN_POINT ( 'NONE',  ( -73.48292372479861001, -275.3399509485612953, -203.4611192335009093 ) ) ;
#66030 = CARTESIAN_POINT ( 'NONE',  ( 32.20547296823256289, -273.1937361781164668, -241.2159385632868407 ) ) ;
#66031 = CARTESIAN_POINT ( 'NONE',  ( -106.0802043782211115, -296.8708493983693870, -295.3878298224027503 ) ) ;
#66032 = CARTESIAN_POINT ( 'NONE',  ( 28.91724979246798455, -292.5581131290470580, -302.4961697213598200 ) ) ;
#66033 = LINE ( 'NONE', #93482, #21549 ) ;
#66034 = CARTESIAN_POINT ( 'NONE',  ( -45.63674563646462445, -277.6468202138307788, -346.9041275316455426 ) ) ;
#66035 = CARTESIAN_POINT ( 'NONE',  ( -11.49220680197487354, -274.5650069652637626, -202.0369934768249323 ) ) ;
#66036 = CARTESIAN_POINT ( 'NONE',  ( -111.4018388592818098, -282.9946217862026856, -289.6066973615876350 ) ) ;
#66037 = CARTESIAN_POINT ( 'NONE',  ( -109.4492848898728852, -298.2790390378648908, -291.6320294789139211 ) ) ;
#66038 = CARTESIAN_POINT ( 'NONE',  ( 209.7064572754725873, 36.40703279031890816, 14.69807322781363546 ) ) ;
#66039 = CARTESIAN_POINT ( 'NONE',  ( 2.543587831087332329, -285.7992832856398877, -209.0278844860571894 ) ) ;
#66040 = EDGE_CURVE ( 'NONE', #10890, #9221, #3499, .T. ) ;
#66041 = CARTESIAN_POINT ( 'NONE',  ( -111.1678542005621324, -276.8604487981932039, -265.1006059854234422 ) ) ;
#66042 = CARTESIAN_POINT ( 'NONE',  ( -108.3938765661287817, -276.8758715650670297, -289.5174000258427327 ) ) ;
#66043 = CARTESIAN_POINT ( 'NONE',  ( -8.246032400199567292, -284.6713510151253104, -339.5011695459937755 ) ) ;
#66044 = CARTESIAN_POINT ( 'NONE',  ( 3.136201015468592868, -275.8139566337198971, -209.0740009697422863 ) ) ;
#66045 = DIRECTION ( 'NONE',  ( -1.000000000000000000, 0.000000000000000000, 0.000000000000000000 ) ) ;
#66046 = CARTESIAN_POINT ( 'NONE',  ( 38.75671217578710070, -273.8907332383798803, -265.5112157061028597 ) ) ;
#66047 = CARTESIAN_POINT ( 'NONE',  ( -81.19052702700666657, -281.4579206195212464, -209.3094283791246539 ) ) ;
#66048 = CARTESIAN_POINT ( 'NONE',  ( 151.2975037349265790, 130.0000000000000568, -12.50000000000000000 ) ) ;
#66049 = CARTESIAN_POINT ( 'NONE',  ( 13.26396962234478494, -288.6729886025011638, -214.1805127963725113 ) ) ;
#66050 = CARTESIAN_POINT ( 'NONE',  ( 37.69313454270169217, -291.5317616071852171, -268.7859035075917404 ) ) ;
#66051 = DIRECTION ( 'NONE',  ( 2.220446049250312686E-15, 0.000000000000000000, 1.000000000000000000 ) ) ;
#66052 = CARTESIAN_POINT ( 'NONE',  ( -110.0682975175384257, -271.3802467245080265, -259.4268275758536788 ) ) ;
#66053 = CARTESIAN_POINT ( 'NONE',  ( -41.64108055106496664, -290.1371457672456131, -196.1998288687785532 ) ) ;
#66054 = CARTESIAN_POINT ( 'NONE',  ( 192.1331913634949160, 286.0196433216794389, -110.9393339982713940 ) ) ;
#66055 = CARTESIAN_POINT ( 'NONE',  ( -40.57949923632136802, -296.0112990352631073, -195.4181424580750104 ) ) ;
#66056 = CARTESIAN_POINT ( 'NONE',  ( 25.79468216994817098, -285.4616420928705907, -227.4833052941875735 ) ) ;
#66057 = CARTESIAN_POINT ( 'NONE',  ( 21.66165175352695371, -283.7681958806242619, -314.7108346939210151 ) ) ;
#66058 = CARTESIAN_POINT ( 'NONE',  ( -30.94650066090903096, -284.3717522162310729, -194.6309231019361903 ) ) ;
#66059 = CARTESIAN_POINT ( 'NONE',  ( -74.07530136059953918, -284.9753751873201963, -334.1845109833982974 ) ) ;
#66060 = EDGE_CURVE ( 'NONE', #87290, #87519, #8917, .T. ) ;
#66061 = CARTESIAN_POINT ( 'NONE',  ( -53.71588573135835532, -284.0703950441616712, -341.7189099582902827 ) ) ;
#66062 = CARTESIAN_POINT ( 'NONE',  ( -38.86117933839373251, -291.0510151458734640, -345.7010011079727292 ) ) ;
#66063 = CARTESIAN_POINT ( 'NONE',  ( -90.15144164196092902, -273.6634804787148596, -214.2805050641428863 ) ) ;
#66064 = ORIENTED_EDGE ( 'NONE', *, *, #31573, .T. ) ;
#66065 = CARTESIAN_POINT ( 'NONE',  ( 2.401529393632486187, -286.6042686961881145, -334.6859261543385742 ) ) ;
#66066 = CARTESIAN_POINT ( 'NONE',  ( 27.64882962133886579, -276.0944812524138570, -311.7546724988639539 ) ) ;
#66067 = CARTESIAN_POINT ( 'NONE',  ( 32.35536109802747262, -295.1829867537711038, -243.6372249810924586 ) ) ;
#66068 = CARTESIAN_POINT ( 'NONE',  ( -48.18343439339131606, -254.9385145489663103, -455.0573192304916006 ) ) ;
#66069 = CARTESIAN_POINT ( 'NONE',  ( -95.95921662488163406, -292.4090924074130839, -317.1477375740089997 ) ) ;
#66070 = CARTESIAN_POINT ( 'NONE',  ( -34.84646163410921815, -281.7050120358837262, -343.8244200158424633 ) ) ;
#66071 = CARTESIAN_POINT ( 'NONE',  ( -76.87292535886210487, -275.5796475827423251, -334.3536929904196313 ) ) ;
#66072 = CARTESIAN_POINT ( 'NONE',  ( -111.7627580636821705, -271.2447935318899681, -253.5024735639898097 ) ) ;
#66073 = CARTESIAN_POINT ( 'NONE',  ( 11.81011439785202022, -275.6966483520877205, -324.5407205639933181 ) ) ;
#66074 = CARTESIAN_POINT ( 'NONE',  ( 13.36634690950409521, -294.2975295354068521, -216.8877440760342665 ) ) ;
#66075 = CARTESIAN_POINT ( 'NONE',  ( -2.337482997635717652, -293.4686188073713424, -206.0187097626381956 ) ) ;
#66076 = CARTESIAN_POINT ( 'NONE',  ( -109.3566275938010364, -286.5352166089218713, -253.2235999723304474 ) ) ;
#66077 = CARTESIAN_POINT ( 'NONE',  ( 34.93503741262060203, -295.2941302456838457, -295.3161050383188808 ) ) ;
#66078 = CARTESIAN_POINT ( 'NONE',  ( 21.91537591650899586, -295.5212637591776570, -318.7748427327967988 ) ) ;
#66079 = CARTESIAN_POINT ( 'NONE',  ( -110.0994113897043150, -296.2992449649553919, -276.8975311389967260 ) ) ;
#66080 = CARTESIAN_POINT ( 'NONE',  ( -70.84354940306981518, -291.4942087385542777, -337.4769689093386660 ) ) ;
#66081 = CARTESIAN_POINT ( 'NONE',  ( -34.47684589114251708, -283.1837523824060554, -347.3078048165201608 ) ) ;
#66082 = CARTESIAN_POINT ( 'NONE',  ( -34.79486249015194232, -296.1636494873990273, -194.8019355729566371 ) ) ;
#66083 = CARTESIAN_POINT ( 'NONE',  ( -49.34263412137227789, -285.7366782149577489, -194.2483421608772574 ) ) ;
#66084 = CARTESIAN_POINT ( 'NONE',  ( -73.61982333243398102, -279.5159652989553365, -335.6118894819285288 ) ) ;
#66085 = CARTESIAN_POINT ( 'NONE',  ( -41.32924030689272854, -284.7957865902727690, -197.0598755493348619 ) ) ;
#66086 = CARTESIAN_POINT ( 'NONE',  ( 31.03089293745648192, -285.9562495446321577, -301.1862564772725364 ) ) ;
#66087 = CARTESIAN_POINT ( 'NONE',  ( -88.08631184020785554, -277.4904669211045984, -214.1002091699997436 ) ) ;
#66088 = LINE ( 'NONE', #73641, #54456 ) ;
#66089 = CARTESIAN_POINT ( 'NONE',  ( -89.70258657129043911, -284.7967025947124853, -219.3343681353435670 ) ) ;
#66090 = CARTESIAN_POINT ( 'NONE',  ( 3.596731780877818530, -281.7944765932532505, -205.5523993004658792 ) ) ;
#66091 = CARTESIAN_POINT ( 'NONE',  ( -20.55955531734109698, -287.9006213800693672, -345.3234250713186952 ) ) ;
#66092 = CIRCLE ( 'NONE', #28235, 7.999999999999998224 ) ;
#66093 = CARTESIAN_POINT ( 'NONE',  ( -5.599255531615181525, -278.2417037915337801, -339.6349054416850777 ) ) ;
#66094 = CARTESIAN_POINT ( 'NONE',  ( -45.57976181540851712, -278.4695144073904771, -346.4758676100841512 ) ) ;
#66095 = CARTESIAN_POINT ( 'NONE',  ( -96.40445346122366743, -278.9858919640156500, -227.4590064584303661 ) ) ;
#66096 = CARTESIAN_POINT ( 'NONE',  ( -92.35136436181264230, -275.2403398427313164, -219.8864300158642493 ) ) ;
#66097 = CARTESIAN_POINT ( 'NONE',  ( 8.850926610725585064, -292.6657811484924423, -208.6890426982433269 ) ) ;
#66098 = CARTESIAN_POINT ( 'NONE',  ( 32.00407513567640905, -285.9353487869912556, -298.1230440207729089 ) ) ;
#66099 = CARTESIAN_POINT ( 'NONE',  ( -8.829665107975266380, -294.0191345196998896, -199.6963865043881583 ) ) ;
#66100 = CARTESIAN_POINT ( 'NONE',  ( -26.17382344825159279, -293.8269501812651470, -342.8145830715150169 ) ) ;
#66101 = CARTESIAN_POINT ( 'NONE',  ( -38.34684057618156316, -294.7318136091298015, -343.3753438536031126 ) ) ;
#66102 = CARTESIAN_POINT ( 'NONE',  ( -101.4332290556287717, -292.1887592232049542, -228.1496667420828999 ) ) ;
#66103 = CARTESIAN_POINT ( 'NONE',  ( 35.62109070840234892, -282.1441816992916642, -265.8529230820548150 ) ) ;
#66104 = EDGE_CURVE ( 'NONE', #17769, #36764, #92785, .T. ) ;
#66105 = CARTESIAN_POINT ( 'NONE',  ( -92.99330366548598192, -272.3359316672772366, -217.4673774189938058 ) ) ;
#66106 = CARTESIAN_POINT ( 'NONE',  ( 37.40729431877169731, -288.4302970889677908, -288.4694880668265569 ) ) ;
#66107 = CARTESIAN_POINT ( 'NONE',  ( 20.64905750427460518, -280.3590095926362551, -319.1194763697392887 ) ) ;
#66108 = CARTESIAN_POINT ( 'NONE',  ( 35.92892959339673808, -288.1823469417914225, -293.9653360743826624 ) ) ;
#66109 = CARTESIAN_POINT ( 'NONE',  ( -2.179929660692826676, -286.8641446966494755, -206.3064384258233019 ) ) ;
#66110 = DIRECTION ( 'NONE',  ( 0.000000000000000000, 1.000000000000000000, 0.000000000000000000 ) ) ;
#66111 = CARTESIAN_POINT ( 'NONE',  ( 23.82377260802752517, -22.69053332001751855, -342.9562588441870048 ) ) ;
#66112 = CARTESIAN_POINT ( 'NONE',  ( 121.1859076339088261, 147.6349627520604315, -260.2004405834634326 ) ) ;
#66113 = CARTESIAN_POINT ( 'NONE',  ( -106.4200512936071448, -277.4276321675980626, -294.6142659312679370 ) ) ;
#66114 = CARTESIAN_POINT ( 'NONE',  ( -89.31462926828430682, -276.7250682024576918, -322.1346745910945515 ) ) ;
#66115 = CARTESIAN_POINT ( 'NONE',  ( 19.33869485627723961, -298.2516321568845115, -193.4272256200833056 ) ) ;
#66116 = CARTESIAN_POINT ( 'NONE',  ( 66.48133663197175736, 45.91875831897123561, -316.4011423777610617 ) ) ;
#66117 = CARTESIAN_POINT ( 'NONE',  ( 24.08057763346275593, -295.9141664115978756, -315.1186874849448145 ) ) ;
#66118 = CARTESIAN_POINT ( 'NONE',  ( -33.51147481886336266, -292.5939780942691186, -197.3875446723942844 ) ) ;
#66119 = CARTESIAN_POINT ( 'NONE',  ( -96.76159264080231992, -274.1480947809783970, -221.7391969496065656 ) ) ;
#66120 = CARTESIAN_POINT ( 'NONE',  ( 8.273016916975223012, -287.0975865961645468, -327.9852541188967052 ) ) ;
#66121 = CARTESIAN_POINT ( 'NONE',  ( -85.75050163867139474, -274.0532577059026380, -210.6124717838628158 ) ) ;
#66122 = CARTESIAN_POINT ( 'NONE',  ( -71.66687781941519120, -297.7519742814442907, -205.9203557116978232 ) ) ;
#66123 = ORIENTED_EDGE ( 'NONE', *, *, #72960, .T. ) ;
#66124 = CARTESIAN_POINT ( 'NONE',  ( 152.4536156746142410, 275.0000000000000568, -12.49999999999999289 ) ) ;
#66125 = CARTESIAN_POINT ( 'NONE',  ( -111.8212895134480647, -280.6345699979332267, -257.6290731998062711 ) ) ;
#66126 = CARTESIAN_POINT ( 'NONE',  ( -89.29522423156527111, -278.8840629922526091, -322.1541459818229214 ) ) ;
#66127 = CARTESIAN_POINT ( 'NONE',  ( -105.4273245950790141, -279.8715159360588700, -304.2184560779058415 ) ) ;
#66128 = CARTESIAN_POINT ( 'NONE',  ( -1.367413542175457408, -273.0182866451992822, -206.0305844135806126 ) ) ;
#66129 = CARTESIAN_POINT ( 'NONE',  ( 61.37083282337847123, -250.8548725835408391, 21.50000000000000000 ) ) ;
#66130 = DIRECTION ( 'NONE',  ( 0.000000000000000000, 1.000000000000000000, 0.000000000000000000 ) ) ;
#66131 = CARTESIAN_POINT ( 'NONE',  ( -74.50761706514632010, -279.7099112787716422, -207.4723333888128138 ) ) ;
#66132 = CARTESIAN_POINT ( 'NONE',  ( 38.97844609957957118, -276.4722499455084517, -279.7180645430580626 ) ) ;
#66133 = CARTESIAN_POINT ( 'NONE',  ( 34.96443898096862313, -277.8090652615731528, -290.3294791407587354 ) ) ;
#66134 = CARTESIAN_POINT ( 'NONE',  ( -103.1079713876986688, -276.6150240926625088, -309.3674106093390037 ) ) ;
#66135 = ORIENTED_EDGE ( 'NONE', *, *, #35872, .F. ) ;
#66136 = CARTESIAN_POINT ( 'NONE',  ( 196.0143093133015384, 24.42324672360809856, 11.99999999999998934 ) ) ;
#66137 = CARTESIAN_POINT ( 'NONE',  ( 37.04826314654771835, -283.6867148496959885, -282.4643720260480677 ) ) ;
#66138 = CARTESIAN_POINT ( 'NONE',  ( -9.656915403891026983, -291.6203586457856431, -202.5860582337112419 ) ) ;
#66139 = CARTESIAN_POINT ( 'NONE',  ( -37.97327468512063575, -285.3930244844734148, -193.4656441189118823 ) ) ;
#66140 = CARTESIAN_POINT ( 'NONE',  ( -56.60392223614617535, -281.5437258422837203, -341.8239811392599563 ) ) ;
#66141 = CARTESIAN_POINT ( 'NONE',  ( 10.27626711274774784, -280.9551496881786079, -326.5343017521307161 ) ) ;
#66142 = CARTESIAN_POINT ( 'NONE',  ( 34.45038752060246878, -282.5561904310054615, -255.0360839601250689 ) ) ;
#66143 = LINE ( 'NONE', #67986, #27646 ) ;
#66144 = CARTESIAN_POINT ( 'NONE',  ( -34.52911555161163903, -281.4172295406225430, -346.5091959951091667 ) ) ;
#66145 = CARTESIAN_POINT ( 'NONE',  ( -111.9509851454597111, -298.4541466758237220, -278.0067204115215418 ) ) ;
#66146 = CARTESIAN_POINT ( 'NONE',  ( -29.67585023549577983, -288.1491791819337891, -195.5863684260210675 ) ) ;
#66147 = DIRECTION ( 'NONE',  ( 0.000000000000000000, 0.000000000000000000, 1.000000000000000000 ) ) ;
#66148 = CARTESIAN_POINT ( 'NONE',  ( -67.77170110816078363, -293.5760985054318439, -201.1854005458759787 ) ) ;
#66149 = CARTESIAN_POINT ( 'NONE',  ( 19.81654992031413087, -274.2240834862521979, -318.9196919231536071 ) ) ;
#66150 = EDGE_CURVE ( 'NONE', #50859, #43923, #18710, .T. ) ;
#66151 = CARTESIAN_POINT ( 'NONE',  ( -51.66524851583518796, -288.4280885383340660, -345.8528048202717855 ) ) ;
#66152 = CARTESIAN_POINT ( 'NONE',  ( 29.47135571708405521, -291.5317990336986327, -238.8962851691227911 ) ) ;
#66153 = CARTESIAN_POINT ( 'NONE',  ( -109.6140389296505617, -277.4117689209807622, -257.0212333084846250 ) ) ;
#66154 = CARTESIAN_POINT ( 'NONE',  ( -93.13440738901661575, -294.0043750418785748, -319.3308974227988415 ) ) ;
#66155 = CARTESIAN_POINT ( 'NONE',  ( -95.32940307620039277, -291.2351964166499556, -315.5330746465203333 ) ) ;
#66156 = LINE ( 'NONE', #32008, #59350 ) ;
#66157 = CARTESIAN_POINT ( 'NONE',  ( 159.4851178187871312, 3.000000000000000000, -10.00000000000000000 ) ) ;
#66158 = CARTESIAN_POINT ( 'NONE',  ( 3.836708363788984499, -292.9888542598583285, -334.6654121107679885 ) ) ;
#66159 = CARTESIAN_POINT ( 'NONE',  ( -1.819014711898614634, -288.1307872994415220, -205.6154633439350619 ) ) ;
#66160 = CARTESIAN_POINT ( 'NONE',  ( -93.94134525835545446, -289.4889604077101239, -219.6614711810919687 ) ) ;
#66161 = CARTESIAN_POINT ( 'NONE',  ( -76.16431008742902975, -291.0074205110040566, -332.8765550575475345 ) ) ;
#66162 = EDGE_CURVE ( 'NONE', #31737, #2308, #12193, .T. ) ;
#66163 = DIRECTION ( 'NONE',  ( -0.000000000000000000, 1.000000000000000000, -0.000000000000000000 ) ) ;
#66164 = CARTESIAN_POINT ( 'NONE',  ( -29.14490234459867324, -289.7484541362188111, -343.0619723992427907 ) ) ;
#66165 = FACE_OUTER_BOUND ( 'NONE', #19629, .T. ) ;
#66166 = CARTESIAN_POINT ( 'NONE',  ( 27.11901448957914340, -289.3040594959810505, -311.8452425603758797 ) ) ;
#66167 = CARTESIAN_POINT ( 'NONE',  ( -76.61333355973137316, -277.5499408138261970, -205.9878486124086692 ) ) ;
#66168 = CARTESIAN_POINT ( 'NONE',  ( -84.55731244321239615, -279.7555171181150513, -209.4953843830671474 ) ) ;
#66169 = CARTESIAN_POINT ( 'NONE',  ( -22.56607903649278413, -279.9029110658683521, -194.7593732424615780 ) ) ;
#66170 = CARTESIAN_POINT ( 'NONE',  ( -9.997698658045548470, -284.4089916776244991, -200.5095058365575085 ) ) ;
#66171 = CARTESIAN_POINT ( 'NONE',  ( 82.64890176555634582, -299.5541904835127980, -195.3611179825600175 ) ) ;
#66172 = CARTESIAN_POINT ( 'NONE',  ( -16.55349886411488924, -278.4632098133459408, -199.0960061382260449 ) ) ;
#66173 = CARTESIAN_POINT ( 'NONE',  ( -3.810469677352952722, -280.6097109925814834, -337.4623265507131578 ) ) ;
#66174 = CARTESIAN_POINT ( 'NONE',  ( 194.7510731661265595, -142.7221692137691775, -21.50000000000000000 ) ) ;
#66175 = CARTESIAN_POINT ( 'NONE',  ( -106.9516383514800992, -276.6277249140856611, -301.7493912487947227 ) ) ;
#66176 = CARTESIAN_POINT ( 'NONE',  ( -109.9365306865469591, -283.1596655254510893, -295.0893020166682277 ) ) ;
#66177 = CARTESIAN_POINT ( 'NONE',  ( -37.16102936435173376, -298.9957304702170973, -197.1229343357308323 ) ) ;
#66178 = CARTESIAN_POINT ( 'NONE',  ( -76.14923425061607531, -274.9698771563925561, -204.4776238346569244 ) ) ;
#66179 = CARTESIAN_POINT ( 'NONE',  ( 0.8788775508262285374, -276.1940202473241470, -332.6400997886959772 ) ) ;
#66180 = CARTESIAN_POINT ( 'NONE',  ( -98.01168189571093592, -297.9514028555648224, -314.4755901044721895 ) ) ;
#66181 = CARTESIAN_POINT ( 'NONE',  ( -78.13460596832146621, -289.7508380882433698, -335.7298134849900748 ) ) ;
#66182 = CARTESIAN_POINT ( 'NONE',  ( -22.81854561775204360, -278.3162935493934356, -196.1567302363904446 ) ) ;
#66183 = CARTESIAN_POINT ( 'NONE',  ( -77.16744560436603706, -291.3675513776994990, -204.3988677873917652 ) ) ;
#66184 = CARTESIAN_POINT ( 'NONE',  ( -71.29245107400900849, -288.5706700674882654, -335.2656172880286363 ) ) ;
#66185 = CARTESIAN_POINT ( 'NONE',  ( 37.60729084355889995, -291.5874995104225036, -273.1268725211789956 ) ) ;
#66186 = VERTEX_POINT ( 'NONE', #77063 ) ;
#66187 = CARTESIAN_POINT ( 'NONE',  ( 197.0504801697426274, 72.68537487628056226, 12.20529943163058384 ) ) ;
#66188 = CARTESIAN_POINT ( 'NONE',  ( -110.0334865253988283, -290.1565627107095793, -263.0199578598904964 ) ) ;
#66189 = DIRECTION ( 'NONE',  ( -0.000000000000000000, -1.000000000000000000, -0.000000000000000000 ) ) ;
#66190 = CARTESIAN_POINT ( 'NONE',  ( -12.79034058128880602, -287.3049248243992793, -197.6283814949794930 ) ) ;
#66191 = CARTESIAN_POINT ( 'NONE',  ( -21.33282851196159058, -297.3376638359844719, -340.3538533559490702 ) ) ;
#66192 = ADVANCED_FACE ( 'NONE', ( #26409 ), #40118, .F. ) ;
#66193 = CARTESIAN_POINT ( 'NONE',  ( 23.83418438494624070, -293.2306099254367382, -316.7327835532024096 ) ) ;
#66194 = CARTESIAN_POINT ( 'NONE',  ( 13.36654357170882967, -283.6755981805604847, -327.7201503939587042 ) ) ;
#66195 = CARTESIAN_POINT ( 'NONE',  ( -94.12070177419889205, -285.0345505328479021, -224.4594481924937099 ) ) ;
#66196 = CARTESIAN_POINT ( 'NONE',  ( 27.06065995135497104, -276.3856676272631034, -234.8491716076192688 ) ) ;
#66197 = CARTESIAN_POINT ( 'NONE',  ( 28.59953159782821785, -292.0395868346770385, -305.4515059461646160 ) ) ;
#66198 = CARTESIAN_POINT ( 'NONE',  ( -72.08219691047548849, -272.3772148180811428, -205.6498068435246580 ) ) ;
#66199 = ORIENTED_EDGE ( 'NONE', *, *, #10780, .T. ) ;
#66200 = CARTESIAN_POINT ( 'NONE',  ( -113.2098679957031493, -271.2709011634024137, -296.4525692007673570 ) ) ;
#66201 = CARTESIAN_POINT ( 'NONE',  ( -22.10588334872066341, -294.5288140447204341, -345.8171593477336501 ) ) ;
#66202 = CARTESIAN_POINT ( 'NONE',  ( 17.00947126192458114, -288.7544643511031950, -219.4771558312718582 ) ) ;
#66203 = CARTESIAN_POINT ( 'NONE',  ( -110.5223253264944532, -297.9231711942348966, -247.2483553638753619 ) ) ;
#66204 = CARTESIAN_POINT ( 'NONE',  ( -19.79941697596794370, -286.9351261977479908, -199.3952038431443725 ) ) ;
#66205 = CARTESIAN_POINT ( 'NONE',  ( -103.2035382961771717, -278.1278574104970858, -230.8238118596773063 ) ) ;
#66206 = CARTESIAN_POINT ( 'NONE',  ( -24.91609755745417232, -295.5491945781254799, -346.3026428160024466 ) ) ;
#66207 = CARTESIAN_POINT ( 'NONE',  ( 20.52996379649732361, -286.3613126322387075, -319.2607703108955661 ) ) ;
#66208 = CARTESIAN_POINT ( 'NONE',  ( 19.51693187456766410, -294.5918196319122444, -322.3313484280354260 ) ) ;
#66209 = CARTESIAN_POINT ( 'NONE',  ( -2.433060018909899203, -292.8607462158156522, -206.2105460648086250 ) ) ;
#66210 = CARTESIAN_POINT ( 'NONE',  ( 143.6449502718966755, -26.00396092263537540, -47.19625681453479871 ) ) ;
#66211 = FACE_BOUND ( 'NONE', #56522, .T. ) ;
#66212 = CARTESIAN_POINT ( 'NONE',  ( 197.0305496340489526, 281.6334632708399681, -110.2979370532489725 ) ) ;
#66213 = CARTESIAN_POINT ( 'NONE',  ( 38.65864648130963133, -289.1584726103948242, -277.1915694142041389 ) ) ;
#66214 = CARTESIAN_POINT ( 'NONE',  ( 40.65961533371913106, -290.8380690714489560, -252.5904736702033802 ) ) ;
#66215 = ORIENTED_EDGE ( 'NONE', *, *, #90373, .T. ) ;
#66216 = ADVANCED_FACE ( 'NONE', ( #68095 ), #77882, .T. ) ;
#66217 = CARTESIAN_POINT ( 'NONE',  ( -56.52319810575206560, -279.1599330881629157, -195.8388643604391746 ) ) ;
#66218 = CARTESIAN_POINT ( 'NONE',  ( 33.08850524321100295, -283.8826458234749452, -295.8050803148556156 ) ) ;
#66219 = CARTESIAN_POINT ( 'NONE',  ( -61.45241253695066064, -183.8721261770043611, -361.2693405134621685 ) ) ;
#66220 = EDGE_CURVE ( 'NONE', #57488, #44867, #25922, .T. ) ;
#66221 = CARTESIAN_POINT ( 'NONE',  ( -95.35719787236388356, -283.8037644705867137, -220.5544399037451342 ) ) ;
#66222 = CARTESIAN_POINT ( 'NONE',  ( -20.83331738389067667, -286.9184498722517560, -342.9475319595702558 ) ) ;
#66223 = CARTESIAN_POINT ( 'NONE',  ( -5.652821940133198275, -276.3248819761196842, -201.5416404841618032 ) ) ;
#66224 = CARTESIAN_POINT ( 'NONE',  ( -57.92811876987593678, -298.2712828428845455, -200.2598497414804228 ) ) ;
#66225 = CARTESIAN_POINT ( 'NONE',  ( -58.56655815169438029, -294.0172417464543173, -340.7226762288333930 ) ) ;
#66226 = CARTESIAN_POINT ( 'NONE',  ( -112.8975821993737867, -279.3835805932195058, -255.9860603205730172 ) ) ;
#66227 = CARTESIAN_POINT ( 'NONE',  ( 33.89326580096770414, -275.7633822261303749, -286.3735107259606139 ) ) ;
#66228 = CARTESIAN_POINT ( 'NONE',  ( 25.88191826893634584, -276.0563511635842247, -226.9297079082920732 ) ) ;
#66229 = CARTESIAN_POINT ( 'NONE',  ( -1.623932807737227701, -275.5102978981704496, -338.2266733710313815 ) ) ;
#66230 = DIRECTION ( 'NONE',  ( 0.000000000000000000, 0.000000000000000000, 1.000000000000000000 ) ) ;
#66231 = CARTESIAN_POINT ( 'NONE',  ( 37.17849715955711076, -273.4376097656809748, -261.4529637872618082 ) ) ;
#66232 = CARTESIAN_POINT ( 'NONE',  ( -112.0253742975123572, -297.7738308010550554, -286.5152229647271156 ) ) ;
#66233 = CARTESIAN_POINT ( 'NONE',  ( 156.8041522122653930, 250.4202232226203648, 16.89672165344857646 ) ) ;
#66234 = CARTESIAN_POINT ( 'NONE',  ( 175.2296996224750103, 20.00000000000000000, 15.00000000000000000 ) ) ;
#66235 = CARTESIAN_POINT ( 'NONE',  ( -71.33370899889742134, -286.6718353107985422, -205.4090633014450304 ) ) ;
#66236 = CARTESIAN_POINT ( 'NONE',  ( -80.96128524120030079, -285.3952042039550179, -332.6449365984241808 ) ) ;
#66237 = CARTESIAN_POINT ( 'NONE',  ( -2.130011946789559296, -285.8796093435105377, -206.2416184379708000 ) ) ;
#66238 = CARTESIAN_POINT ( 'NONE',  ( -109.3832904801213033, -277.1616709541115711, -254.2892951371272261 ) ) ;
#66239 = CARTESIAN_POINT ( 'NONE',  ( -104.1134967517435967, -285.9792942613892137, -302.9196978354106022 ) ) ;
#66240 = CARTESIAN_POINT ( 'NONE',  ( -111.0439562123325032, -277.0646320494101360, -267.8656547143996249 ) ) ;
#66241 = CARTESIAN_POINT ( 'NONE',  ( -24.26099852445735650, -277.9610216637191229, -342.5454526789682177 ) ) ;
#66242 = CARTESIAN_POINT ( 'NONE',  ( 197.4487343191780440, 71.87628676167049946, -11.52796263498073159 ) ) ;
#66243 = CARTESIAN_POINT ( 'NONE',  ( -110.4032385894416564, -273.0444201342810402, -270.3673720632041864 ) ) ;
#66244 = CARTESIAN_POINT ( 'NONE',  ( 37.51785605277983393, -282.1371794258329260, -252.9768987208467763 ) ) ;
#66245 = CARTESIAN_POINT ( 'NONE',  ( -4.184672242022903887, -283.1190158340443759, -339.8028128101969969 ) ) ;
#66246 = ORIENTED_EDGE ( 'NONE', *, *, #2847, .F. ) ;
#66247 = ORIENTED_EDGE ( 'NONE', *, *, #47379, .T. ) ;
#66248 = CARTESIAN_POINT ( 'NONE',  ( 196.7775620068246951, 42.35718252767666314, 12.67800755580416450 ) ) ;
#66249 = CARTESIAN_POINT ( 'NONE',  ( 26.09046235596253283, -288.8593408859181295, -228.9284467850930582 ) ) ;
#66250 = CARTESIAN_POINT ( 'NONE',  ( -111.0712337495254616, -288.9794200432615412, -290.7879176716971870 ) ) ;
#66251 = CARTESIAN_POINT ( 'NONE',  ( -109.0450232749765433, -295.5571919200965567, -284.9574814036002408 ) ) ;
#66252 = CARTESIAN_POINT ( 'NONE',  ( -73.37859312159817193, -290.9355723273632748, -202.4149856994655750 ) ) ;
#66253 = CARTESIAN_POINT ( 'NONE',  ( -15.66602171189749804, -287.2465526226158090, -340.8479028432313385 ) ) ;
#66254 = CARTESIAN_POINT ( 'NONE',  ( 23.99063488775317410, -286.6869393951224083, -311.0500775808962999 ) ) ;
#66255 = AXIS2_PLACEMENT_3D ( 'NONE', #46013, #10028, #38898 ) ;
#66256 = CARTESIAN_POINT ( 'NONE',  ( -38.64727948680960168, -287.2405332112700762, -196.9631070599960196 ) ) ;
#66257 = CARTESIAN_POINT ( 'NONE',  ( -108.6402299844791628, -276.8544628302163346, -246.9258729306777411 ) ) ;
#66258 = CARTESIAN_POINT ( 'NONE',  ( -34.71078962606990359, -291.0192456420278404, -345.3149635237269308 ) ) ;
#66259 = CARTESIAN_POINT ( 'NONE',  ( -59.51144153415526006, -287.3384259627416100, -342.1840320860181350 ) ) ;
#66260 = CARTESIAN_POINT ( 'NONE',  ( -95.29530733418177135, -284.8647811227368152, -315.1564422041469129 ) ) ;
#66261 = CARTESIAN_POINT ( 'NONE',  ( -110.5379609001591916, -292.7713613690945067, -253.2632865322329110 ) ) ;
#66262 = CARTESIAN_POINT ( 'NONE',  ( 123.4306832106270946, -134.2391364535880882, -4.999999999999990230 ) ) ;
#66263 = CARTESIAN_POINT ( 'NONE',  ( 29.33919985515026596, -212.1443419142231051, 25.50000000000000000 ) ) ;
#66264 = CARTESIAN_POINT ( 'NONE',  ( -107.6414661936025396, -274.8849138503065319, -243.0815948640712065 ) ) ;
#66265 = CARTESIAN_POINT ( 'NONE',  ( 27.93006829711379879, -280.3002559186471103, -237.2003369834671105 ) ) ;
#66266 = CARTESIAN_POINT ( 'NONE',  ( 17.26502906607845489, -280.2731301445279541, -321.8471598800334732 ) ) ;
#66267 = CARTESIAN_POINT ( 'NONE',  ( 29.42927706732763582, -293.2453693709277900, -308.4921940707182557 ) ) ;
#66268 = CARTESIAN_POINT ( 'NONE',  ( -90.91483488503378396, -271.5186021575332234, -219.2750459673879391 ) ) ;
#66269 = CARTESIAN_POINT ( 'NONE',  ( -29.58726449603378938, -275.0331772571075248, -344.4480384772639354 ) ) ;
#66270 = CARTESIAN_POINT ( 'NONE',  ( -55.43113996832510537, -299.1298088578427041, -199.0763255000922527 ) ) ;
#66271 = DIRECTION ( 'NONE',  ( -0.000000000000000000, 1.000000000000000000, -0.000000000000000000 ) ) ;
#66273 =( BOUNDED_SURFACE ( )  B_SPLINE_SURFACE ( 3, 2, ( 
 ( #70983, #71453, #48709 ),
 ( #92736, #27908, #35924 ),
 ( #56309, #6589, #85174 ),
 ( #35467, #77612, #49195 ),
 ( #21247, #36384, #64386 ),
 ( #29291, #92263, #28363 ),
 ( #50116, #58187, #41604 ),
 ( #57255, #79012, #14166 ),
 ( #71933, #64842, #51048 ),
 ( #87940, #23575, #23092 ) ),
 .UNSPECIFIED., .F., .F., .F. ) 
 B_SPLINE_SURFACE_WITH_KNOTS ( ( 4, 2, 2, 2, 4 ),
 ( 3, 3 ),
 ( 0.000000000000000000, 0.002512116609398717254, 0.005024233218797434508, 0.007536349828196151762, 0.01004846643759486902 ),
 ( 0.000000000000000000, 1.000000000000000000 ),
 .UNSPECIFIED. ) 
 GEOMETRIC_REPRESENTATION_ITEM ( )  RATIONAL_B_SPLINE_SURFACE ( (
 ( 1.000000000000000000, 0.8168508380123967738, 1.000000000000000000),
 ( 1.000000000000000000, 0.8469983227716593177, 1.000000000000000000),
 ( 1.000000000000000000, 0.8738795229725790925, 1.000000000000000000),
 ( 1.000000000000000000, 0.9200744724124843010, 1.000000000000000000),
 ( 1.000000000000000000, 0.9393932456996403335, 1.000000000000000000),
 ( 1.000000000000000000, 0.9701270577444791599, 1.000000000000000000),
 ( 1.000000000000000000, 0.9814990972770829547, 1.000000000000000000),
 ( 1.000000000000000000, 0.9964108658798418450, 1.000000000000000000),
 ( 1.000000000000000000, 1.000001410412884040, 1.000000000000000000),
 ( 1.000000000000000000, 1.000000000000000000, 1.000000000000000000) ) ) 
 REPRESENTATION_ITEM ( '' )  SURFACE ( )  );
#66272 = CARTESIAN_POINT ( 'NONE',  ( -113.3244589239191953, -294.8017813316301954, -269.5901594478612537 ) ) ;
#66274 = CARTESIAN_POINT ( 'NONE',  ( -28.80978810612744567, -296.3672858384592246, -343.5055084722031893 ) ) ;
#66275 = DIRECTION ( 'NONE',  ( 0.000000000000000000, 1.000000000000000000, 0.000000000000000000 ) ) ;
#66276 = CARTESIAN_POINT ( 'NONE',  ( -68.57701191593261569, -296.2762252371691716, -336.5334537720560775 ) ) ;
#66277 = EDGE_CURVE ( 'NONE', #89964, #13924, #8162, .T. ) ;
#66278 = CARTESIAN_POINT ( 'NONE',  ( 156.4217629211117355, 119.0463968525363327, 9.000000000000001776 ) ) ;
#66280 = CARTESIAN_POINT ( 'NONE',  ( -103.7185893734331330, -296.9633585651827161, -239.8567469666458578 ) ) ;
#66279 = CARTESIAN_POINT ( 'NONE',  ( -99.62253987202920769, -283.1449827732726021, -227.8484269787984999 ) ) ;
#66281 = CARTESIAN_POINT ( 'NONE',  ( -110.9260302234101516, -284.8390000856119855, -247.5024510225785548 ) ) ;
#66282 = CARTESIAN_POINT ( 'NONE',  ( 37.01301151980471360, -283.6445369452757177, -283.8752483961154667 ) ) ;
#66283 = CARTESIAN_POINT ( 'NONE',  ( -49.33724514145076512, -285.5701039007482223, -194.2689122834692625 ) ) ;
#66284 = CARTESIAN_POINT ( 'NONE',  ( 36.72586583802087290, -291.4145776740485871, -259.6829112690270449 ) ) ;
#66285 = CARTESIAN_POINT ( 'NONE',  ( -112.6954123733869579, -277.7079001701363836, -285.7602027750559159 ) ) ;
#66286 = CARTESIAN_POINT ( 'NONE',  ( -106.6662871844225293, -281.6237833571633473, -303.7098442033569654 ) ) ;
#66287 = CARTESIAN_POINT ( 'NONE',  ( -43.49887528382338786, -252.7496869255646459, -490.1845544134979491 ) ) ;
#66288 = CARTESIAN_POINT ( 'NONE',  ( 31.76814765271049978, -286.6744077386492791, -295.0787117998168014 ) ) ;
#66289 = EDGE_CURVE ( 'NONE', #87518, #41101, #62403, .T. ) ;
#66290 = CARTESIAN_POINT ( 'NONE',  ( -84.98345390722781190, -288.6120137024563519, -330.5267680774360315 ) ) ;
#66291 = FACE_OUTER_BOUND ( 'NONE', #71598, .T. ) ;
#66292 = CARTESIAN_POINT ( 'NONE',  ( -112.4206482094779176, -280.1573145912028053, -256.0869066622111632 ) ) ;
#66294 = CARTESIAN_POINT ( 'NONE',  ( 21.02424669222132536, -281.8350989828747970, -314.2623411900966062 ) ) ;
#66293 = CARTESIAN_POINT ( 'NONE',  ( 3.318125674472236497, -292.5291581139214259, -333.8668899640919108 ) ) ;
#66295 = CARTESIAN_POINT ( 'NONE',  ( 0.5423524140913242864, -294.7283853601740589, -337.4120983849635991 ) ) ;
#66296 = CARTESIAN_POINT ( 'NONE',  ( -29.58597057095891714, -284.2294967350505317, -195.2002048942119643 ) ) ;
#66297 = CARTESIAN_POINT ( 'NONE',  ( -104.3991098286895323, -280.9972328294093700, -236.6551308134961005 ) ) ;
#66298 = CARTESIAN_POINT ( 'NONE',  ( -110.6495100021942335, -270.7648327654998184, -253.7480675990668715 ) ) ;
#66299 = ORIENTED_EDGE ( 'NONE', *, *, #66834, .F. ) ;
#66300 = CARTESIAN_POINT ( 'NONE',  ( 199.1087447750284980, 64.61450673763175701, -10.46317447812566392 ) ) ;
#66301 = CARTESIAN_POINT ( 'NONE',  ( 36.66007489787520512, -283.4009729962876349, -260.2010829297898908 ) ) ;
#66302 = CARTESIAN_POINT ( 'NONE',  ( -77.98917990656750021, -295.1221123911157065, -331.1327783948392494 ) ) ;
#66303 = CARTESIAN_POINT ( 'NONE',  ( 121.3395553409046670, -299.5541904835127980, -195.3611179825600175 ) ) ;
#66304 = CARTESIAN_POINT ( 'NONE',  ( -112.3417001280813707, -270.0523547857347353, -270.3292895737510548 ) ) ;
#66305 = CARTESIAN_POINT ( 'NONE',  ( -64.83274058808314066, -272.8992798406845282, -198.5946004532373763 ) ) ;
#66306 = ADVANCED_FACE ( 'NONE', ( #5105 ), #26874, .F. ) ;
#66307 = CARTESIAN_POINT ( 'NONE',  ( -98.84290870578105626, -289.8415005164987406, -309.6879707422454544 ) ) ;
#66308 = CARTESIAN_POINT ( 'NONE',  ( -79.46690301104561627, -280.9916952213127956, -209.8948047739962419 ) ) ;
#66309 = CARTESIAN_POINT ( 'NONE',  ( -11.22598392839584136, -275.9982241095415247, -201.2817819423349590 ) ) ;
#66310 = CARTESIAN_POINT ( 'NONE',  ( -21.86832297695727689, -284.4571705894740603, -344.9735500094316762 ) ) ;
#66311 = CARTESIAN_POINT ( 'NONE',  ( -54.57119190547125243, -278.6208465729222326, -198.9624758551673551 ) ) ;
#66312 = CARTESIAN_POINT ( 'NONE',  ( -65.04893841182567371, -279.4141527832276779, -340.1106632695494909 ) ) ;
#66313 = ORIENTED_EDGE ( 'NONE', *, *, #21333, .T. ) ;
#66314 = CARTESIAN_POINT ( 'NONE',  ( -81.24864485088895094, -273.3070385659617614, -207.0416248235253533 ) ) ;
#66315 = CARTESIAN_POINT ( 'NONE',  ( -97.94772280539935139, -293.0654984960622187, -227.0509325671463614 ) ) ;
#66316 = DIRECTION ( 'NONE',  ( 0.000000000000000000, 0.000000000000000000, -1.000000000000000000 ) ) ;
#66317 = CARTESIAN_POINT ( 'NONE',  ( 38.37164501064047784, -291.7272215707329224, -273.1530430956136684 ) ) ;
#66318 = CIRCLE ( 'NONE', #14946, 3.842139515347647638 ) ;
#66319 = CARTESIAN_POINT ( 'NONE',  ( 21.53448887771002163, -274.4541891647140801, -227.0993240997837574 ) ) ;
#66320 = CARTESIAN_POINT ( 'NONE',  ( -37.81037309103371058, -293.5664969595428602, -194.0558881400799294 ) ) ;
#66322 = CARTESIAN_POINT ( 'NONE',  ( 19.11260001187631730, -294.0491121035935862, -218.5835097482835181 ) ) ;
#66321 = CARTESIAN_POINT ( 'NONE',  ( 35.78497577281001440, -278.2662352645559167, -287.0191576251351080 ) ) ;
#66323 = EDGE_CURVE ( 'NONE', #27549, #86758, #53884, .T. ) ;
#66324 = CARTESIAN_POINT ( 'NONE',  ( 3.424946345996064068, -288.6018247239894094, -207.6067638692849471 ) ) ;
#66325 = CARTESIAN_POINT ( 'NONE',  ( 18.79403842591196749, -274.2415484329758328, -319.8658665008601929 ) ) ;
#66326 = B_SPLINE_CURVE_WITH_KNOTS ( 'NONE', 3,
 ( #9267, #23021, #46190, #75095, #1259, #51900, #23504, #31995, #39073, #15941, #44795, #38144, #8807, #67061, #60427, #2197, #89267, #24417, #53297, #82647, #32476, #10675, #68929, #62290 ),
 .UNSPECIFIED., .F., .F.,
 ( 4, 2, 2, 2, 2, 2, 2, 2, 2, 2, 2, 4 ),
 ( 5.000000000000000311E-10, 0.06250000043739496747, 0.1250000003747899491, 0.2500000002495798568, 0.3750000001243697922, 0.4999999999991597277, 0.6249999998739497187, 0.7499999997487397652, 0.8124999996861348439, 0.8749999996235298116, 0.9374999995609247794, 0.9999999994983197471 ),
 .UNSPECIFIED. ) ;
#66327 = CARTESIAN_POINT ( 'NONE',  ( 36.04115808835049251, -277.3096142734244154, -257.7847379865123116 ) ) ;
#66328 = CARTESIAN_POINT ( 'NONE',  ( 37.14883234711485471, -291.6375679589755237, -270.7921943464806986 ) ) ;
#66329 = CARTESIAN_POINT ( 'NONE',  ( -98.44595379486447939, -281.0173802862722710, -225.5443959811486820 ) ) ;
#66330 = EDGE_LOOP ( 'NONE', ( #55716, #25260, #8524, #24529 ) ) ;
#66331 = CARTESIAN_POINT ( 'NONE',  ( -33.49935557264054609, -282.6692078668725685, -343.2936768864429951 ) ) ;
#66332 = CARTESIAN_POINT ( 'NONE',  ( -50.89854609281908893, -280.9624848078023547, -194.8779779019191380 ) ) ;
#66333 = CARTESIAN_POINT ( 'NONE',  ( -81.34607319154994798, -282.4304646125908675, -333.1283203970305067 ) ) ;
#66334 = CARTESIAN_POINT ( 'NONE',  ( -41.36010559900251593, -278.0428033818589029, -347.0337453539904686 ) ) ;
#66335 = CARTESIAN_POINT ( 'NONE',  ( 24.75134548844062010, -276.4791412284788521, -225.9860788277405845 ) ) ;
#66336 = CARTESIAN_POINT ( 'NONE',  ( 30.89617123739170168, -283.8376638359844719, -254.7536222014695397 ) ) ;
#66337 = ORIENTED_EDGE ( 'NONE', *, *, #14901, .T. ) ;
#66338 = CARTESIAN_POINT ( 'NONE',  ( -108.9583337159623966, -274.8347243186335618, -248.4788891605057870 ) ) ;
#66339 = CARTESIAN_POINT ( 'NONE',  ( -14.76420760042905655, -293.4313878049808864, -200.6152729145111095 ) ) ;
#66340 = CARTESIAN_POINT ( 'NONE',  ( -111.7975396809801651, -276.6407332248783746, -265.0531280738588293 ) ) ;
#66341 = CARTESIAN_POINT ( 'NONE',  ( -37.47698575588407266, -290.8139219892755705, -346.3605677252420492 ) ) ;
#66342 = CARTESIAN_POINT ( 'NONE',  ( 4.568863140731014738, -291.9827902628720722, -210.4041752620166790 ) ) ;
#66343 = CARTESIAN_POINT ( 'NONE',  ( 22.35342337738662621, -287.7117428803312009, -318.9206914852170485 ) ) ;
#66344 = CARTESIAN_POINT ( 'NONE',  ( 165.4284657918965991, 2.965303559109564446, 10.00000000000000000 ) ) ;
#66345 = CARTESIAN_POINT ( 'NONE',  ( -110.4013569069839491, -283.0880799951265203, -259.9338955989343276 ) ) ;
#66346 = CARTESIAN_POINT ( 'NONE',  ( -111.3521065996476835, -292.3295727306268645, -276.7595594117125870 ) ) ;
#66347 = CARTESIAN_POINT ( 'NONE',  ( -101.5863601767124607, -283.5226122734850378, -234.1549068759208012 ) ) ;
#66348 = CARTESIAN_POINT ( 'NONE',  ( -35.66824909721538717, -281.3887259151706530, -196.8745333958138417 ) ) ;
#66349 = CARTESIAN_POINT ( 'NONE',  ( -99.67218712236601164, -290.8974015767936976, -315.1913412864594193 ) ) ;
#66350 = CARTESIAN_POINT ( 'NONE',  ( -57.13590006197910043, -280.2821311035039002, -200.0320479583949975 ) ) ;
#66351 = CARTESIAN_POINT ( 'NONE',  ( -37.77729363036129229, -290.8417404348701325, -193.7594275390628127 ) ) ;
#66352 = CARTESIAN_POINT ( 'NONE',  ( 31.27300087953015151, -287.9089917782112025, -235.7752592302306880 ) ) ;
#66353 = CARTESIAN_POINT ( 'NONE',  ( -3.082497158390807179, -289.1041096724353565, -339.2657485101670432 ) ) ;
#66354 = CARTESIAN_POINT ( 'NONE',  ( -59.98064433010927132, -285.9171105684835652, -200.9602663313739299 ) ) ;
#66355 = ORIENTED_EDGE ( 'NONE', *, *, #81253, .F. ) ;
#66356 = CARTESIAN_POINT ( 'NONE',  ( 202.9738562182569694, 293.9636489450776367, -40.00000000000000711 ) ) ;
#66357 = CARTESIAN_POINT ( 'NONE',  ( 36.55127138825917399, -295.1991612316996907, -253.5658206663924261 ) ) ;
#66358 = CARTESIAN_POINT ( 'NONE',  ( -25.00395213005931794, -293.5829239540091748, -345.9203204897705746 ) ) ;
#66359 = CARTESIAN_POINT ( 'NONE',  ( -1.365063887643188645, -275.6216248807390343, -334.2079192884575036 ) ) ;
#66360 = CARTESIAN_POINT ( 'NONE',  ( -43.27360506565078424, -297.3278282692725156, -193.6390453134878555 ) ) ;
#66361 = CARTESIAN_POINT ( 'NONE',  ( 15.38498961005499943, -291.2935091543484987, -218.8039926352263933 ) ) ;
#66362 = CARTESIAN_POINT ( 'NONE',  ( -108.5842135590440591, -294.5304442075395173, -290.4229796823129277 ) ) ;
#66363 = CARTESIAN_POINT ( 'NONE',  ( -1.073747979820776077, -293.7500094523796861, -206.5361733068681644 ) ) ;
#66364 = CARTESIAN_POINT ( 'NONE',  ( 34.51677014748355532, -294.4412016062966018, -255.8495252330793619 ) ) ;
#66365 = DIRECTION ( 'NONE',  ( 1.000000000000000000, 0.000000000000000000, 0.000000000000000000 ) ) ;
#66366 = CARTESIAN_POINT ( 'NONE',  ( -33.55333369635184226, -293.0044396248879934, -345.4450694999377447 ) ) ;
#66367 = CARTESIAN_POINT ( 'NONE',  ( 27.29300515917568148, -300.8614267717341022, -195.3390746317473088 ) ) ;
#66368 = CARTESIAN_POINT ( 'NONE',  ( -109.1671486716764861, -291.3045187041875579, -284.7260276395792289 ) ) ;
#66369 = CARTESIAN_POINT ( 'NONE',  ( -80.16374633245293069, -295.9834818402999304, -329.5080523541774937 ) ) ;
#66370 = CARTESIAN_POINT ( 'NONE',  ( -94.67122848778222988, -281.2062132988971825, -221.4359537063214134 ) ) ;
#66371 = CARTESIAN_POINT ( 'NONE',  ( -53.63899006283128301, -278.5322222808999300, -195.5560037588437581 ) ) ;
#66372 = ORIENTED_EDGE ( 'NONE', *, *, #608, .F. ) ;
#66373 = CARTESIAN_POINT ( 'NONE',  ( -110.9371423211469931, -272.1830232205388711, -247.8851359201196658 ) ) ;
#66374 = CARTESIAN_POINT ( 'NONE',  ( 34.33961225689883179, -279.8922357795186144, -290.4385594123805276 ) ) ;
#66375 = CARTESIAN_POINT ( 'NONE',  ( -70.86410080892369479, -278.0171472278371425, -201.9309413702808342 ) ) ;
#66376 = CARTESIAN_POINT ( 'NONE',  ( -103.1753293625201024, -277.0333375185752516, -234.0849317754581875 ) ) ;
#66377 = CARTESIAN_POINT ( 'NONE',  ( 52.44288484880080148, -297.8839743961142403, -196.8885969919342642 ) ) ;
#66378 = LINE ( 'NONE', #30379, #29273 ) ;
#66379 = CIRCLE ( 'NONE', #76980, 0.5000000000000007772 ) ;
#66380 = CARTESIAN_POINT ( 'NONE',  ( 197.4878715644970555, 25.93102243561465414, 12.00000000000000178 ) ) ;
#66381 = CARTESIAN_POINT ( 'NONE',  ( -110.6681626797553548, -288.3496113813343982, -287.7840965609291288 ) ) ;
#66382 = CARTESIAN_POINT ( 'NONE',  ( -112.5653432347661465, -290.3464978709251341, -286.8050687778560359 ) ) ;
#66383 = CARTESIAN_POINT ( 'NONE',  ( -43.90859531930468052, -275.9696206022821912, -195.4298133591807130 ) ) ;
#66384 = CARTESIAN_POINT ( 'NONE',  ( -84.42694655853519237, -271.4038055238236780, -211.9832093679705451 ) ) ;
#66385 = CARTESIAN_POINT ( 'NONE',  ( -95.21985270194804230, -283.0643773297090888, -320.9009861604972116 ) ) ;
#66386 = CARTESIAN_POINT ( 'NONE',  ( 222.4306832106270804, -142.7221692137691775, -21.50000000000000000 ) ) ;
#66387 = CARTESIAN_POINT ( 'NONE',  ( -44.82435747161934358, -281.1465808093095120, -345.0378756386635359 ) ) ;
#66388 = CARTESIAN_POINT ( 'NONE',  ( 197.4836817735085219, 24.47698789593440694, 11.66666666666668384 ) ) ;
#66389 = CARTESIAN_POINT ( 'NONE',  ( 36.01868852669803545, -292.3166263472769515, -268.0407990168725973 ) ) ;
#66390 = CARTESIAN_POINT ( 'NONE',  ( -49.60259615746537776, -284.0338749568397247, -197.0930699730296283 ) ) ;
#66391 = CARTESIAN_POINT ( 'NONE',  ( 197.4878715644970555, 25.93102243561465414, 12.00000000000000000 ) ) ;
#66392 = DIRECTION ( 'NONE',  ( 0.000000000000000000, 1.000000000000000000, 0.000000000000000000 ) ) ;
#66393 = CARTESIAN_POINT ( 'NONE',  ( -19.57432356220730441, -290.2803447609423984, -197.4423248559728279 ) ) ;
#66394 = CARTESIAN_POINT ( 'NONE',  ( -48.71119869762767252, -278.7993323017034868, -343.3320294535976700 ) ) ;
#66395 = CARTESIAN_POINT ( 'NONE',  ( -27.40830629665333618, -284.1338210319679547, -346.3703525756164936 ) ) ;
#66397 = CARTESIAN_POINT ( 'NONE',  ( -54.75633926039605370, -285.8221506931667477, -199.4164344587780988 ) ) ;
#66396 = CARTESIAN_POINT ( 'NONE',  ( -32.74530106327306100, -272.1894717146834068, -194.9281410629301661 ) ) ;
#66398 = CARTESIAN_POINT ( 'NONE',  ( 18.76937238010619424, -277.6489623735701571, -317.9733271361920401 ) ) ;
#66399 = CARTESIAN_POINT ( 'NONE',  ( -41.85635686782941889, -277.9132939323004052, -343.3957910124282762 ) ) ;
#66400 = CARTESIAN_POINT ( 'NONE',  ( -107.4247345445486843, -286.2035275346000844, -297.2146699692959260 ) ) ;
#66401 = ORIENTED_EDGE ( 'NONE', *, *, #87430, .T. ) ;
#66402 = DIRECTION ( 'NONE',  ( 0.000000000000000000, -1.000000000000000000, 0.000000000000000000 ) ) ;
#66403 = CARTESIAN_POINT ( 'NONE',  ( -66.92640102486173248, -295.2626021873625177, -341.4650200683968819 ) ) ;
#66404 = CARTESIAN_POINT ( 'NONE',  ( -22.14916247711017760, -288.2274679733395146, -197.2256968131548263 ) ) ;
#66405 = CARTESIAN_POINT ( 'NONE',  ( 140.6539576904058606, 275.5000000000000568, 10.50000000000000000 ) ) ;
#66406 = CARTESIAN_POINT ( 'NONE',  ( 40.65961533371913106, -290.8380690714489560, -252.5904736702033802 ) ) ;
#66407 = CARTESIAN_POINT ( 'NONE',  ( -113.4086810581186882, -277.6001355830888428, -260.1951521424682028 ) ) ;
#66408 = CARTESIAN_POINT ( 'NONE',  ( -98.54969839028463241, -289.5620170710945445, -224.9518089885522443 ) ) ;
#66409 = CARTESIAN_POINT ( 'NONE',  ( -109.0959934856486058, -285.8521682315225689, -287.2099122023921041 ) ) ;
#66410 = CARTESIAN_POINT ( 'NONE',  ( -100.3419038568832207, -280.8417284533395559, -231.4181145263924861 ) ) ;
#66411 = CARTESIAN_POINT ( 'NONE',  ( 39.11318161578627439, -288.9920798421018162, -271.5240665824787811 ) ) ;
#66412 = CARTESIAN_POINT ( 'NONE',  ( 36.53280121039472306, -283.3861069353757784, -257.4166712002287909 ) ) ;
#66413 = CARTESIAN_POINT ( 'NONE',  ( 12.70622787710087565, -276.5429018825201979, -328.8778242028647583 ) ) ;
#66414 = CARTESIAN_POINT ( 'NONE',  ( -99.81056001969753311, -295.1271678595230128, -229.4082545889327491 ) ) ;
#66415 = CARTESIAN_POINT ( 'NONE',  ( -93.07228700772414243, -279.1125913604073503, -217.1520707403757342 ) ) ;
#66416 = CARTESIAN_POINT ( 'NONE',  ( -36.48664548758041803, -299.9830890439129121, -195.9208274694676390 ) ) ;
#66417 = CARTESIAN_POINT ( 'NONE',  ( 199.9041579857632200, 299.4540172553377602, -5.820662028140222155 ) ) ;
#66418 = EDGE_CURVE ( 'NONE', #7087, #15166, #322, .T. ) ;
#66419 = CARTESIAN_POINT ( 'NONE',  ( -37.30987171927208124, -279.5519495502701943, -345.3611179825600175 ) ) ;
#66420 = CARTESIAN_POINT ( 'NONE',  ( -46.73324378088730668, -272.1743328474673262, -194.9570536345238736 ) ) ;
#66421 = CARTESIAN_POINT ( 'NONE',  ( 175.2296996224750103, 250.5000000000000568, 0.000000000000000000 ) ) ;
#66422 = CARTESIAN_POINT ( 'NONE',  ( -109.6818351608113176, -278.1994185451076191, -259.7685426337143895 ) ) ;
#66423 = CARTESIAN_POINT ( 'NONE',  ( 12.45817665826460363, -277.5811304314962058, -328.5674835242627978 ) ) ;
#66424 = CARTESIAN_POINT ( 'NONE',  ( -101.2299964412172528, -283.0479968938050774, -313.0136063724921200 ) ) ;
#66425 = CARTESIAN_POINT ( 'NONE',  ( 21.99918749449010491, -289.9246533858199655, -314.6161867917600716 ) ) ;
#66426 = CARTESIAN_POINT ( 'NONE',  ( -35.51225111912538779, -299.5947782959736401, -194.0539833116449699 ) ) ;
#66427 = CARTESIAN_POINT ( 'NONE',  ( -35.49928932413877192, -299.2798060552077573, -193.7578199242622645 ) ) ;
#66428 = CARTESIAN_POINT ( 'NONE',  ( 33.52927831415468773, -295.2389984394819749, -246.1722224118713314 ) ) ;
#66429 = CARTESIAN_POINT ( 'NONE',  ( 25.66050301481099893, -280.0980954985886342, -310.8388866879950569 ) ) ;
#66430 = CARTESIAN_POINT ( 'NONE',  ( -10.88415542613376985, -272.4187809568127818, -200.5072420580083588 ) ) ;
#66431 = CARTESIAN_POINT ( 'NONE',  ( -87.24160528045565854, -286.9707023451973100, -212.7027079817666504 ) ) ;
#66432 = CARTESIAN_POINT ( 'NONE',  ( 16.22748109302714070, -287.1899460208875894, -320.4810471324510104 ) ) ;
#66433 = CARTESIAN_POINT ( 'NONE',  ( 155.3377760462712445, 206.0000123873846292, -217.0427545417765032 ) ) ;
#66434 = EDGE_LOOP ( 'NONE', ( #40058, #54092, #63703, #88552 ) ) ;
#66435 = CARTESIAN_POINT ( 'NONE',  ( 36.92737983449001149, -286.3539476226549709, -288.3804692032369985 ) ) ;
#66436 = CARTESIAN_POINT ( 'NONE',  ( 1.319180486372797612, -288.1867502374390142, -332.3080613846667575 ) ) ;
#66437 = ORIENTED_EDGE ( 'NONE', *, *, #25761, .F. ) ;
#66438 = CARTESIAN_POINT ( 'NONE',  ( -49.31010628200724000, -286.9828289858222092, -194.5563607979073026 ) ) ;
#66439 = CARTESIAN_POINT ( 'NONE',  ( 33.91483296102150291, -276.0966094320498883, -286.3739913341262309 ) ) ;
#66440 = EDGE_CURVE ( 'NONE', #36747, #17168, #51948, .T. ) ;
#66441 = CARTESIAN_POINT ( 'NONE',  ( 35.18956090077695364, -292.7895902999543978, -295.4377947591495399 ) ) ;
#66442 = CARTESIAN_POINT ( 'NONE',  ( 4.497204700011000256, -283.1553272494535918, -334.9439668628541540 ) ) ;
#66443 = CARTESIAN_POINT ( 'NONE',  ( 30.09988783270704715, -282.6058122709053464, -234.5506230181639182 ) ) ;
#66444 = CARTESIAN_POINT ( 'NONE',  ( 19.77067678675773266, -282.5871612583490560, -322.0522926998226012 ) ) ;
#66446 = CARTESIAN_POINT ( 'NONE',  ( -14.30623014153881201, -280.6923918672146101, -201.0151350796725751 ) ) ;
#66445 = AXIS2_PLACEMENT_3D ( 'NONE', #78402, #41446, #63281 ) ;
#66447 = CARTESIAN_POINT ( 'NONE',  ( -105.5795714935544112, -294.2666405000204009, -254.7536222014695397 ) ) ;
#66448 = CARTESIAN_POINT ( 'NONE',  ( 194.6022636468435110, 278.9903764957075509, -125.9409043586979209 ) ) ;
#66449 = EDGE_LOOP ( 'NONE', ( #91832, #58175, #73003, #17672 ) ) ;
#66450 = CARTESIAN_POINT ( 'NONE',  ( -110.5532232720421462, -280.3529109491770441, -285.8563207669483859 ) ) ;
#66451 = CARTESIAN_POINT ( 'NONE',  ( -13.87141369607328301, -91.16939480456166223, -359.4227886527972942 ) ) ;
#66452 = CARTESIAN_POINT ( 'NONE',  ( -111.2570529628670215, -268.0638518741617986, -295.3521300423831235 ) ) ;
#66453 = CARTESIAN_POINT ( 'NONE',  ( -110.4862351550085151, -295.8863065711019544, -271.4563773625523595 ) ) ;
#66454 = CARTESIAN_POINT ( 'NONE',  ( 33.27040466433985699, -292.6701675038814301, -239.8085802835533684 ) ) ;
#66455 = CARTESIAN_POINT ( 'NONE',  ( -110.5520430423103448, -271.6439828081399241, -270.3495548111940820 ) ) ;
#66457 = CARTESIAN_POINT ( 'NONE',  ( -97.21950132061779470, -288.3552761995064770, -313.5014626807680997 ) ) ;
#66456 = CARTESIAN_POINT ( 'NONE',  ( 7.576521399050904826, -297.1788500536419519, -193.9609729414230230 ) ) ;
#66458 = CARTESIAN_POINT ( 'NONE',  ( -83.10291939514574722, -297.5462449141708703, -328.8798386925689101 ) ) ;
#66459 = CARTESIAN_POINT ( 'NONE',  ( 19.88873418501042067, -288.2195641263478478, -224.2334746198176560 ) ) ;
#66460 = ORIENTED_EDGE ( 'NONE', *, *, #9747, .F. ) ;
#66461 = CARTESIAN_POINT ( 'NONE',  ( -0.8075652796476866513, -295.5203950504831028, -337.8894923163524595 ) ) ;
#66462 = CARTESIAN_POINT ( 'NONE',  ( -79.34978597921673327, -285.9605087977898847, -210.5218419567632679 ) ) ;
#66463 = CARTESIAN_POINT ( 'NONE',  ( -35.46848148622010655, -296.8700448510948036, -193.7585612416910976 ) ) ;
#66464 = CARTESIAN_POINT ( 'NONE',  ( -90.68121765459423500, -292.1222409655414936, -214.9785416743855251 ) ) ;
#66465 = CARTESIAN_POINT ( 'NONE',  ( 37.69989018066195285, -293.8313140517606712, -253.3230648666520040 ) ) ;
#66466 = ADVANCED_FACE ( 'NONE', ( #35385 ), #41990, .T. ) ;
#66467 = CARTESIAN_POINT ( 'NONE',  ( -109.7004112790123713, -290.8511441086107538, -260.3312183724216311 ) ) ;
#66468 = VERTEX_POINT ( 'NONE', #77533 ) ;
#66469 = CARTESIAN_POINT ( 'NONE',  ( 157.4221907153413724, 15.99782226686522790, 9.062927103449265331 ) ) ;
#66470 = CARTESIAN_POINT ( 'NONE',  ( 0.4535464150409347361, -276.4717381111614714, -204.9180421043208469 ) ) ;
#66471 = CARTESIAN_POINT ( 'NONE',  ( 37.56039170075763423, -274.1445016512689676, -254.2464691009641058 ) ) ;
#66472 = ORIENTED_EDGE ( 'NONE', *, *, #17028, .T. ) ;
#66473 = CARTESIAN_POINT ( 'NONE',  ( 3.463544080642186440, -276.0271454067687955, -335.6500424881484150 ) ) ;
#66474 = CARTESIAN_POINT ( 'NONE',  ( -38.07003196200111717, -272.4427462068400700, -196.5647091927194481 ) ) ;
#66475 = CARTESIAN_POINT ( 'NONE',  ( -60.13504490293512106, -281.6141142164237294, -199.6575674739028727 ) ) ;
#66476 = CARTESIAN_POINT ( 'NONE',  ( -18.72975919936687816, -274.9495012294592016, -342.2253033075599546 ) ) ;
#66477 = CARTESIAN_POINT ( 'NONE',  ( -98.10708992559519004, -274.2004947042232175, -229.2608562051539138 ) ) ;
#66478 = CARTESIAN_POINT ( 'NONE',  ( -48.92443079987220500, -274.8423769140602531, -197.9962336114622019 ) ) ;
#66479 = CARTESIAN_POINT ( 'NONE',  ( -65.86787885169044898, -275.4442033553438591, -199.9182238212333402 ) ) ;
#66480 = CARTESIAN_POINT ( 'NONE',  ( -86.93452339649391547, -271.3865157570705264, -213.5558957347547562 ) ) ;
#66481 = CARTESIAN_POINT ( 'NONE',  ( -94.84849385212076811, -296.5680316617691687, -315.4927182660333642 ) ) ;
#66482 = CARTESIAN_POINT ( 'NONE',  ( 35.79038758835083911, -292.2398906598892836, -278.9975681299496841 ) ) ;
#66483 = CARTESIAN_POINT ( 'NONE',  ( 215.9306832106270804, -199.2391364535880882, 9.184850993605165694E-16 ) ) ;
#66484 = EDGE_CURVE ( 'NONE', #54755, #55081, #35348, .T. ) ;
#66485 = CARTESIAN_POINT ( 'NONE',  ( 22.59701001507071538, -276.6916989883891347, -318.6196825054826718 ) ) ;
#66486 = CARTESIAN_POINT ( 'NONE',  ( 15.44532235868296866, -274.9907889820449896, -219.8644380348377183 ) ) ;
#66487 = CARTESIAN_POINT ( 'NONE',  ( -100.5793658247346229, -283.8095936837894442, -227.2060260905129496 ) ) ;
#66488 = CARTESIAN_POINT ( 'NONE',  ( -107.7119898544983982, -298.2082499067275876, -296.9284819815736682 ) ) ;
#66489 = CARTESIAN_POINT ( 'NONE',  ( 209.9972545312790544, 27.55378999303205845, 10.00000000000000000 ) ) ;
#66490 = CARTESIAN_POINT ( 'NONE',  ( 0.2604114106753362967, -285.7636028412070459, -207.5431242034451031 ) ) ;
#66491 = CARTESIAN_POINT ( 'NONE',  ( -96.40707171369399475, -277.4102245005706209, -225.7390138244824698 ) ) ;
#66492 = CARTESIAN_POINT ( 'NONE',  ( -67.05710276042545104, -276.0242310646790997, -337.6839949623957864 ) ) ;
#66493 = CARTESIAN_POINT ( 'NONE',  ( 34.58704563722467640, -283.8264306477723267, -291.6487622513163842 ) ) ;
#66494 = CARTESIAN_POINT ( 'NONE',  ( 34.28411631165699447, -276.9682628140044471, -286.4455762975343873 ) ) ;
#66495 = CARTESIAN_POINT ( 'NONE',  ( 154.7659666677267580, 19.56018909072084000, 12.94946946941269594 ) ) ;
#66496 = CARTESIAN_POINT ( 'NONE',  ( 33.98021069235073099, -273.6090891243063083, -243.5352824689463205 ) ) ;
#66497 = CARTESIAN_POINT ( 'NONE',  ( -39.55931662244956470, -282.0245547066186305, -195.2144272685848989 ) ) ;
#66498 = FACE_OUTER_BOUND ( 'NONE', #87863, .T. ) ;
#66499 = CARTESIAN_POINT ( 'NONE',  ( -84.63107619886696398, -287.3265379459054429, -211.4287066457472406 ) ) ;
#66500 = CARTESIAN_POINT ( 'NONE',  ( -94.98446313033487343, -287.8892222012290745, -318.3632743255333253 ) ) ;
#66501 = CARTESIAN_POINT ( 'NONE',  ( 82.12401493620129145, -301.5056145204703171, -195.8476787650543258 ) ) ;
#66502 = CARTESIAN_POINT ( 'NONE',  ( -52.70329859634396286, -296.6459803833660658, -198.5374274384009539 ) ) ;
#66503 = CARTESIAN_POINT ( 'NONE',  ( -64.50183602250376680, -289.8334230107046210, -201.2590630098414124 ) ) ;
#66504 = CARTESIAN_POINT ( 'NONE',  ( -79.37448608631180491, -205.8233151019928755, -350.8497528714748341 ) ) ;
#66505 = DIRECTION ( 'NONE',  ( 0.000000000000000000, -1.000000000000000000, 0.000000000000000000 ) ) ;
#66506 = CARTESIAN_POINT ( 'NONE',  ( 26.85095983609733139, -286.5793011421721985, -311.7139331892660152 ) ) ;
#66507 = CARTESIAN_POINT ( 'NONE',  ( -106.9882521355795149, -283.1860748371248633, -239.8432679973196571 ) ) ;
#66508 = CARTESIAN_POINT ( 'NONE',  ( -57.65494131097599961, -291.7825971754450052, -200.1913941367027974 ) ) ;
#66509 = CARTESIAN_POINT ( 'NONE',  ( 13.73108449473622450, -282.2099691721807062, -217.3095081051319255 ) ) ;
#66510 = CARTESIAN_POINT ( 'NONE',  ( 3.488797392179261880, -283.2906668567015345, -331.1304941987315829 ) ) ;
#66511 = CARTESIAN_POINT ( 'NONE',  ( -62.19682020397199551, -291.3535493450925173, -341.5543945126098038 ) ) ;
#66512 = TOROIDAL_SURFACE ( 'NONE', #12084, 2.500000000000009770, 0.5000000000000000000 ) ;
#66513 = CARTESIAN_POINT ( 'NONE',  ( -37.25571840298405135, -298.2198816790711362, -193.3603518727142898 ) ) ;
#66514 = ORIENTED_EDGE ( 'NONE', *, *, #52243, .F. ) ;
#66515 = CARTESIAN_POINT ( 'NONE',  ( -70.03850431079013106, -287.5592570848596097, -338.4945918141465881 ) ) ;
#66516 = CARTESIAN_POINT ( 'NONE',  ( 29.09594759657340290, -276.0587965248112141, -309.2846194285332331 ) ) ;
#66518 = CARTESIAN_POINT ( 'NONE',  ( 3.111170379154164056, -294.5778371256207606, -207.5670376179971299 ) ) ;
#66517 = VECTOR ( 'NONE', #72213, 1000.000000000000000 ) ;
#66519 = DIRECTION ( 'NONE',  ( -0.000000000000000000, -1.000000000000000000, -0.000000000000000000 ) ) ;
#66520 = CARTESIAN_POINT ( 'NONE',  ( 21.31550574532285580, -284.6948066931273615, -317.0979686699210447 ) ) ;
#66521 = CARTESIAN_POINT ( 'NONE',  ( -79.22626523709432433, -275.6153139136299615, -332.8394249949083701 ) ) ;
#66522 = CARTESIAN_POINT ( 'NONE',  ( 208.0393982316568326, 37.47427918878999265, 12.00000000000000000 ) ) ;
#66523 = CARTESIAN_POINT ( 'NONE',  ( -111.5316412369251680, -294.7315912071073853, -287.8041955825242439 ) ) ;
#66524 = CARTESIAN_POINT ( 'NONE',  ( 30.36931392717984934, -275.2708971366317883, -298.0477452263011742 ) ) ;
#66525 = CARTESIAN_POINT ( 'NONE',  ( -97.90780328148092337, -291.4925754448390194, -312.3648817795429409 ) ) ;
#66526 = CARTESIAN_POINT ( 'NONE',  ( -99.91885982448586390, -292.0156976170268308, -232.3149942361840772 ) ) ;
#66527 = CARTESIAN_POINT ( 'NONE',  ( -103.9144633109148543, -285.8790356856410995, -302.8213076755470752 ) ) ;
#66528 = CARTESIAN_POINT ( 'NONE',  ( 33.90677886897459103, -294.6232960429947525, -242.6059220584592708 ) ) ;
#66529 = CARTESIAN_POINT ( 'NONE',  ( 39.21811721119787819, -294.8664747357288434, -270.2935693556833030 ) ) ;
#66530 = CARTESIAN_POINT ( 'NONE',  ( 12.35332046792512450, -294.1704580053282712, -323.9038025302235155 ) ) ;
#66531 = CARTESIAN_POINT ( 'NONE',  ( 19.35369671610927611, -290.2339909428848159, -319.5371026280207616 ) ) ;
#66532 = CARTESIAN_POINT ( 'NONE',  ( -50.09141791109876607, -283.3770948579393121, -346.3521030884660945 ) ) ;
#66533 = CARTESIAN_POINT ( 'NONE',  ( -104.5028619447186173, -271.1527953924508552, -235.1809469547474691 ) ) ;
#66534 = CARTESIAN_POINT ( 'NONE',  ( -99.78972236026685039, -283.7871752351571217, -315.4973625877774452 ) ) ;
#66535 = EDGE_CURVE ( 'NONE', #74021, #93112, #61041, .T. ) ;
#66536 = CARTESIAN_POINT ( 'NONE',  ( -110.7164244104488802, -283.3040410710634092, -273.6406560215482386 ) ) ;
#66537 = CARTESIAN_POINT ( 'NONE',  ( 29.88316102465614321, -285.9920934734542470, -303.7320165516460975 ) ) ;
#66538 = CARTESIAN_POINT ( 'NONE',  ( -94.95092859298588905, -277.3665260073635750, -221.1326401466070024 ) ) ;
#66539 = CARTESIAN_POINT ( 'NONE',  ( 197.0349383350915105, 285.8449894349855640, -111.9383547020201064 ) ) ;
#66540 = CARTESIAN_POINT ( 'NONE',  ( -59.99175983336060369, -285.2581894993325591, -200.8991626623587479 ) ) ;
#66541 = CARTESIAN_POINT ( 'NONE',  ( -69.27040478109327637, -288.5207737621898900, -340.1850828346537128 ) ) ;
#66542 = CARTESIAN_POINT ( 'NONE',  ( -14.80663321872071414, -278.3651990363064783, -343.2079281468933800 ) ) ;
#66543 = CARTESIAN_POINT ( 'NONE',  ( -20.22006829968976405, -278.1519357152525913, -344.9818892261909582 ) ) ;
#66544 = CARTESIAN_POINT ( 'NONE',  ( -93.08882614292124913, -279.0554556474177730, -223.2116671916093651 ) ) ;
#66545 = CARTESIAN_POINT ( 'NONE',  ( -59.99835590321384871, -275.7371306236574355, -199.1837045198811040 ) ) ;
#66546 = CARTESIAN_POINT ( 'NONE',  ( 17.33086569621237771, -284.8347823811419630, -219.2448528056791019 ) ) ;
#66547 = CARTESIAN_POINT ( 'NONE',  ( -106.9917741021248077, -291.7522190346152229, -301.3988668028130178 ) ) ;
#66548 = CARTESIAN_POINT ( 'NONE',  ( -42.42482450855411713, -294.0380902419025233, -343.4937913948334085 ) ) ;
#66549 = ORIENTED_EDGE ( 'NONE', *, *, #92592, .T. ) ;
#66550 = CARTESIAN_POINT ( 'NONE',  ( -31.60492727441741678, -294.6445953116143528, -343.2066915103906126 ) ) ;
#66551 = CARTESIAN_POINT ( 'NONE',  ( -64.29310352260451111, -292.7883705282490041, -198.5060406575162517 ) ) ;
#66552 = CARTESIAN_POINT ( 'NONE',  ( 18.90923190084793504, -281.5421454768553531, -223.6541646988366381 ) ) ;
#66553 = EDGE_CURVE ( 'NONE', #74598, #48115, #34828, .T. ) ;
#66554 = CARTESIAN_POINT ( 'NONE',  ( -34.04958490837677942, -297.0127962974689808, -193.6708147898868333 ) ) ;
#66555 = CARTESIAN_POINT ( 'NONE',  ( 5.116474773709787094, -287.2610284032228378, -206.1836121535922075 ) ) ;
#66556 = CARTESIAN_POINT ( 'NONE',  ( -75.64947500029836647, -289.8821706816476649, -337.1313110021119996 ) ) ;
#66557 = CARTESIAN_POINT ( 'NONE',  ( -10.74622434378185787, -286.7420567776412668, -202.3419405886913580 ) ) ;
#66558 = DIRECTION ( 'NONE',  ( -0.000000000000000000, -1.000000000000000000, -0.000000000000000000 ) ) ;
#66559 = CARTESIAN_POINT ( 'NONE',  ( -113.9111842188364676, -271.2735285581878202, -270.3448380411595622 ) ) ;
#66560 = CARTESIAN_POINT ( 'NONE',  ( 196.2181823052468701, 281.8870305299420806, -110.2198146774690173 ) ) ;
#66561 = CARTESIAN_POINT ( 'NONE',  ( -61.85353664513819183, -276.5760912380897025, -339.3480755774759245 ) ) ;
#66562 = CARTESIAN_POINT ( 'NONE',  ( -70.60529391094118523, -276.4219086716603897, -335.6892084426448264 ) ) ;
#66563 = CARTESIAN_POINT ( 'NONE',  ( -90.14526775557085614, -272.9970254716726572, -214.2746923727137300 ) ) ;
#66564 = CARTESIAN_POINT ( 'NONE',  ( -87.51707661104852320, -230.5351160159351878, -345.2162280226144162 ) ) ;
#66565 = CARTESIAN_POINT ( 'NONE',  ( -107.1331604661673111, -276.8326398854349577, -301.8341558931759323 ) ) ;
#66566 = CARTESIAN_POINT ( 'NONE',  ( 33.51477028915017797, -295.6646396652234330, -297.8080597423184486 ) ) ;
#66567 = CARTESIAN_POINT ( 'NONE',  ( -94.34285458221397391, -291.6900755765959161, -224.6372224042051471 ) ) ;
#66568 = CARTESIAN_POINT ( 'NONE',  ( -110.6621322215138576, -297.6463770327770249, -247.2004727337939869 ) ) ;
#66569 = CARTESIAN_POINT ( 'NONE',  ( -85.01758769131480165, -288.4107559172310857, -326.3590920367963122 ) ) ;
#66570 = CARTESIAN_POINT ( 'NONE',  ( -93.10397136821094932, -273.9283399552204514, -217.3902058459342754 ) ) ;
#66571 = CARTESIAN_POINT ( 'NONE',  ( -79.72977094586097735, -297.6276265469426789, -210.9283706387506925 ) ) ;
#66572 = EDGE_LOOP ( 'NONE', ( #69188, #48116, #63673, #14996, #38198, #61325 ) ) ;
#66573 = CARTESIAN_POINT ( 'NONE',  ( -23.68628624284178130, -55.96374926131388605, -22.50000000000000000 ) ) ;
#66574 = CARTESIAN_POINT ( 'NONE',  ( -112.7747213021608985, -280.5281136083064553, -265.9823610640664242 ) ) ;
#66575 = AXIS2_PLACEMENT_3D ( 'NONE', #82349, #11315, #55349 ) ;
#66576 = CARTESIAN_POINT ( 'NONE',  ( -85.69834922065264493, -280.4436098588087702, -215.2624740673053338 ) ) ;
#66577 = CARTESIAN_POINT ( 'NONE',  ( -74.81667695509624139, -279.3041413628073428, -336.4640689456617224 ) ) ;
#66578 = CONICAL_SURFACE ( 'NONE', #84667, 2.390969801828402019, 0.09862129276974965220 ) ;
#66579 = CARTESIAN_POINT ( 'NONE',  ( -11.22657677776744833, -272.8784770234071857, -201.3956818251809864 ) ) ;
#66580 = FACE_OUTER_BOUND ( 'NONE', #54616, .T. ) ;
#66581 = CARTESIAN_POINT ( 'NONE',  ( -39.80257052418233599, -229.5268262511776527, 25.50000000000000000 ) ) ;
#66582 = CARTESIAN_POINT ( 'NONE',  ( -87.53216568059616520, -279.4948925565139461, -217.2826061526542674 ) ) ;
#66583 = CARTESIAN_POINT ( 'NONE',  ( 39.39242218108820026, -276.2933073416227217, -265.4399090191439541 ) ) ;
#66584 = CARTESIAN_POINT ( 'NONE',  ( 37.70638377075786707, -277.5621275484356829, -271.1251693911075336 ) ) ;
#66585 = CARTESIAN_POINT ( 'NONE',  ( -79.91308313417442832, -276.1901095226338612, -333.8778254082728267 ) ) ;
#66586 = VERTEX_POINT ( 'NONE', #70903 ) ;
#66587 = CARTESIAN_POINT ( 'NONE',  ( 3.672086032151444801, -284.4835922050748422, -333.6389085444195644 ) ) ;
#66588 = CARTESIAN_POINT ( 'NONE',  ( -38.89077038600851211, -291.2293907658622061, -197.2160422166857927 ) ) ;
#66589 = CARTESIAN_POINT ( 'NONE',  ( 36.59552054225849105, -286.6333361015286414, -249.0390530379026757 ) ) ;
#66590 = CARTESIAN_POINT ( 'NONE',  ( -61.89169633937681425, -281.6153929035950227, -340.2382459872948175 ) ) ;
#66592 = CARTESIAN_POINT ( 'NONE',  ( -14.09351650650305920, -284.4357645358466016, -199.5904562764217474 ) ) ;
#66591 = CARTESIAN_POINT ( 'NONE',  ( -94.75604204560765709, -282.4814043955014427, -316.4134227080695609 ) ) ;
#66593 = CARTESIAN_POINT ( 'NONE',  ( -66.24009643592751218, -280.8703140021155491, -202.8787943446638167 ) ) ;
#66594 = PLANE ( 'NONE',  #71523 ) ;
#66595 = CARTESIAN_POINT ( 'NONE',  ( -76.36589203693866068, -281.9642796306976038, -335.8711607248457085 ) ) ;
#66596 = CARTESIAN_POINT ( 'NONE',  ( 31.58875881740157965, -295.9403147710103781, -300.0489787163130018 ) ) ;
#66597 = CARTESIAN_POINT ( 'NONE',  ( -107.3309813039151095, -286.9099069751821389, -242.8054133358070885 ) ) ;
#66598 = LINE ( 'NONE', #73251, #48914 ) ;
#66599 = CARTESIAN_POINT ( 'NONE',  ( -66.48309816784104953, -293.5936382171083210, -200.6467498814550368 ) ) ;
#66600 = CARTESIAN_POINT ( 'NONE',  ( -18.53949519698757697, -274.8097791831771133, -342.9660608962062156 ) ) ;
#66601 = CARTESIAN_POINT ( 'NONE',  ( -40.34270959484315000, -288.2861179086589800, -347.1540703233896465 ) ) ;
#66602 = CARTESIAN_POINT ( 'NONE',  ( 36.50841899612134966, -291.9575421380910143, -270.7846300421712158 ) ) ;
#66603 = CARTESIAN_POINT ( 'NONE',  ( -48.18343439339133027, -264.7419918502239398, -441.7985027589016909 ) ) ;
#66604 = CARTESIAN_POINT ( 'NONE',  ( -94.84932671742315335, -276.5948735245735293, -316.1427413071419323 ) ) ;
#66605 = CARTESIAN_POINT ( 'NONE',  ( -106.9560242299685910, -295.0315424710443040, -244.4309774975177731 ) ) ;
#66606 = CARTESIAN_POINT ( 'NONE',  ( -63.98415273363372791, -290.7220956686800264, -338.9096281953815151 ) ) ;
#66607 = SURFACE_STYLE_USAGE ( .BOTH. , #23971 ) ;
#66608 = CARTESIAN_POINT ( 'NONE',  ( 25.92596590112605170, -292.5992345257535021, -313.0215233704839761 ) ) ;
#66609 = CARTESIAN_POINT ( 'NONE',  ( 27.74553075529512469, -289.6226049905581590, -305.2563260982196311 ) ) ;
#66610 = CARTESIAN_POINT ( 'NONE',  ( -95.78493256127491406, -289.4539712661127737, -221.7780424918552455 ) ) ;
#66611 = EDGE_CURVE ( 'NONE', #21221, #59134, #34448, .T. ) ;
#66612 = CARTESIAN_POINT ( 'NONE',  ( -1.918562638523249708, -287.9559594502072741, -205.8014211269785676 ) ) ;
#66613 = DIRECTION ( 'NONE',  ( 1.000000000000000000, 0.000000000000000000, 0.000000000000000000 ) ) ;
#66614 = CARTESIAN_POINT ( 'NONE',  ( 22.11685055905892838, -287.7594261060488634, -227.6461249135607829 ) ) ;
#66615 = CARTESIAN_POINT ( 'NONE',  ( -85.32809321431076910, -297.6914147089660787, -328.4620033316837748 ) ) ;
#66616 = CARTESIAN_POINT ( 'NONE',  ( 82.64890176555634582, -299.5541904835138780, -192.9651424135223863 ) ) ;
#66617 = CARTESIAN_POINT ( 'NONE',  ( -70.45347019368922759, -290.6839807462974932, -339.4524373328906677 ) ) ;
#66618 = CARTESIAN_POINT ( 'NONE',  ( -61.49601793128326932, -277.7601708064456147, -198.9269948074795309 ) ) ;
#66619 = CARTESIAN_POINT ( 'NONE',  ( -97.03530360568313995, -278.2328109423121987, -318.9864700914941977 ) ) ;
#66620 = CARTESIAN_POINT ( 'NONE',  ( -86.78789101243724247, -279.0531173677605352, -211.2931821224103714 ) ) ;
#66621 = CARTESIAN_POINT ( 'NONE',  ( -75.72229887860241604, -283.5396852722327026, -205.9256441488438156 ) ) ;
#66622 = CARTESIAN_POINT ( 'NONE',  ( -110.9948563253906997, -274.0459037229676369, -270.3801370180107710 ) ) ;
#66623 = CARTESIAN_POINT ( 'NONE',  ( -3.768093034443908085, -278.6394812760652826, -204.1376373545090814 ) ) ;
#66624 = CARTESIAN_POINT ( 'NONE',  ( -24.89133884712969191, -280.8933118828296074, -344.3732004978055556 ) ) ;
#66625 = DIRECTION ( 'NONE',  ( 0.000000000000000000, 1.000000000000000000, 0.000000000000000000 ) ) ;
#66626 = CARTESIAN_POINT ( 'NONE',  ( -112.0348454774373153, -277.2298124661746215, -254.6891549789921498 ) ) ;
#66627 = CARTESIAN_POINT ( 'NONE',  ( -98.34171545634058020, -274.5460398394204731, -229.1074149326821896 ) ) ;
#66628 = CARTESIAN_POINT ( 'NONE',  ( -114.0170112492860000, -283.5132591388492642, -267.1137264803851394 ) ) ;
#66629 = CARTESIAN_POINT ( 'NONE',  ( -109.2904024274250645, -273.5331711080482364, -256.8239539616066054 ) ) ;
#66630 = CARTESIAN_POINT ( 'NONE',  ( -99.10161077251049733, -274.5801524595136129, -225.2809147237078093 ) ) ;
#66631 = CARTESIAN_POINT ( 'NONE',  ( 23.81352440969225981, -274.6661249362725812, -230.4596643937491649 ) ) ;
#66632 = CARTESIAN_POINT ( 'NONE',  ( -61.63761508680422452, -297.3678486702981445, -341.3718377428374424 ) ) ;
#66633 = CARTESIAN_POINT ( 'NONE',  ( -69.35536841980209033, -289.6285265735170924, -340.4049997764796558 ) ) ;
#66634 = CARTESIAN_POINT ( 'NONE',  ( -79.09432247200943777, -277.5740299021042574, -207.3219212862858001 ) ) ;
#66635 = CARTESIAN_POINT ( 'NONE',  ( -110.7824890474801549, -290.0927151617007098, -293.6751278584420675 ) ) ;
#66637 = CARTESIAN_POINT ( 'NONE',  ( -98.31318920715831666, -289.0492812452019962, -310.9534737019613999 ) ) ;
#66636 = AXIS2_PLACEMENT_3D ( 'NONE', #90150, #24361, #25298 ) ;
#66638 = CARTESIAN_POINT ( 'NONE',  ( -14.45196511547495000, -290.3485889822512718, -198.8848804238548098 ) ) ;
#66639 = VERTEX_POINT ( 'NONE', #21165 ) ;
#66640 = CARTESIAN_POINT ( 'NONE',  ( 154.1415209985679269, 20.37991841447902175, 11.45812909362559040 ) ) ;
#66641 = CARTESIAN_POINT ( 'NONE',  ( -107.7868233548885826, -289.8017717728951652, -289.9247424993363893 ) ) ;
#66642 = CARTESIAN_POINT ( 'NONE',  ( 169.7306087885279453, 276.0000000000000568, -24.89999999999999147 ) ) ;
#66643 = VECTOR ( 'NONE', #40854, 1000.000000000000000 ) ;
#66644 = CARTESIAN_POINT ( 'NONE',  ( 23.66711653063709520, -287.8700596135395813, -223.7483207976022754 ) ) ;
#66645 = CARTESIAN_POINT ( 'NONE',  ( -82.08285599513421005, -292.1948066931273615, -326.5171145203363494 ) ) ;
#66646 = CARTESIAN_POINT ( 'NONE',  ( 11.04069315161959963, -293.4602013878662774, -330.0279682166208772 ) ) ;
#66647 = CARTESIAN_POINT ( 'NONE',  ( -65.05781846114622624, -284.7219546923205939, -341.6852220976551280 ) ) ;
#66648 = CARTESIAN_POINT ( 'NONE',  ( -110.0959412061875895, -284.3065188182854968, -276.3461334077276774 ) ) ;
#66649 = CARTESIAN_POINT ( 'NONE',  ( 29.52784386171970965, -276.4575154558016266, -239.7469643032682427 ) ) ;
#66650 = CARTESIAN_POINT ( 'NONE',  ( 34.21288022044010546, -291.2950836534887458, -248.9274711602004970 ) ) ;
#66651 = CARTESIAN_POINT ( 'NONE',  ( -5.119962510331440342, -273.2809468059714391, -204.4011015592346894 ) ) ;
#66652 = ORIENTED_EDGE ( 'NONE', *, *, #2889, .F. ) ;
#66653 = LINE ( 'NONE', #15520, #16885 ) ;
#66654 = CARTESIAN_POINT ( 'NONE',  ( 30.88164433630877426, -293.6790123540964146, -306.0166864331076226 ) ) ;
#66655 = CARTESIAN_POINT ( 'NONE',  ( -75.47843760216241549, -287.4593674365907532, -206.4322242598769037 ) ) ;
#66656 = CARTESIAN_POINT ( 'NONE',  ( -101.2995229053768895, -298.1909737508792091, -228.0182974826144289 ) ) ;
#66657 = CARTESIAN_POINT ( 'NONE',  ( 32.36829771458664595, -287.9117171895986189, -248.3099355626429201 ) ) ;
#66658 = CARTESIAN_POINT ( 'NONE',  ( -113.9976860803573118, -277.5596677635057290, -274.4452372310885835 ) ) ;
#66659 = CARTESIAN_POINT ( 'NONE',  ( -36.38797637594077372, -292.7152250514493517, -193.4559499800649292 ) ) ;
#66660 = CARTESIAN_POINT ( 'NONE',  ( 13.43689223911416164, -284.8930272069046055, -214.0604690638379566 ) ) ;
#66661 = CARTESIAN_POINT ( 'NONE',  ( 30.88556681058348374, -294.3454674177526726, -306.0091801671821941 ) ) ;
#66662 = CARTESIAN_POINT ( 'NONE',  ( -81.74526626170977295, -291.7619236875598290, -212.3280806636016393 ) ) ;
#66663 = LINE ( 'NONE', #31610, #14657 ) ;
#66664 = CARTESIAN_POINT ( 'NONE',  ( 180.0836269057152208, 251.0244910122962949, -164.3671539782268667 ) ) ;
#66665 = CARTESIAN_POINT ( 'NONE',  ( -112.4510006355684908, -285.8986872631709275, -284.1156267515526110 ) ) ;
#66666 = CARTESIAN_POINT ( 'NONE',  ( 25.18497378105905682, -279.6952119285918457, -320.2651865833026363 ) ) ;
#66667 = ORIENTED_EDGE ( 'NONE', *, *, #67205, .T. ) ;
#66668 = CARTESIAN_POINT ( 'NONE',  ( -5.912845675140160573, -281.5493938731575554, -336.6052296906557331 ) ) ;
#66669 = CARTESIAN_POINT ( 'NONE',  ( -111.4213247328650880, -277.9565197447284959, -291.2884567999438445 ) ) ;
#66670 = CARTESIAN_POINT ( 'NONE',  ( 21.64133933810120780, -284.1855163729746323, -316.4157538635529932 ) ) ;
#66671 = CARTESIAN_POINT ( 'NONE',  ( -61.35559941387249694, -183.8768497150109340, -360.9409086351379869 ) ) ;
#66672 = CARTESIAN_POINT ( 'NONE',  ( -99.32126633906587188, -282.5287862902465008, -315.1389364568215683 ) ) ;
#66673 = CARTESIAN_POINT ( 'NONE',  ( 33.84973376563834790, -285.2808363263382603, -247.8766542323534736 ) ) ;
#66674 = CARTESIAN_POINT ( 'NONE',  ( -68.36039097110868568, -275.5094503813119218, -201.2228144700276573 ) ) ;
#66675 = CARTESIAN_POINT ( 'NONE',  ( -104.8214434374840778, -297.4197765858179991, -242.3526784617394867 ) ) ;
#66676 = ADVANCED_FACE ( 'NONE', ( #28745 ), #73131, .T. ) ;
#66677 = CARTESIAN_POINT ( 'NONE',  ( -10.32418687202441809, -293.3768298803088328, -338.7080085908231126 ) ) ;
#66678 = CARTESIAN_POINT ( 'NONE',  ( -109.6380863644192942, -278.8704263816352409, -296.7188510151196965 ) ) ;
#66679 = CARTESIAN_POINT ( 'NONE',  ( -56.60017204741144070, -277.3072711218024438, -340.8274729419055689 ) ) ;
#66680 = CARTESIAN_POINT ( 'NONE',  ( -107.7989798829545407, -274.0206871230410570, -239.9403905836601041 ) ) ;
#66681 = CARTESIAN_POINT ( 'NONE',  ( -84.68639591732380723, -276.6072652499581181, -330.7607884625851398 ) ) ;
#66682 = CARTESIAN_POINT ( 'NONE',  ( 197.8563597697584839, 42.27872732282708057, 12.00000000000000355 ) ) ;
#66683 = CARTESIAN_POINT ( 'NONE',  ( -5.654136641094509308, -274.6353443764088524, -338.3521506364288030 ) ) ;
#66684 = EDGE_CURVE ( 'NONE', #4576, #47569, #77722, .T. ) ;
#66685 = CARTESIAN_POINT ( 'NONE',  ( -96.04698207720574032, -297.3142253595705142, -319.2925613599231269 ) ) ;
#66686 = CARTESIAN_POINT ( 'NONE',  ( 175.2296996224750103, 133.0000000000000000, -24.00000000000001066 ) ) ;
#66687 = CARTESIAN_POINT ( 'NONE',  ( 26.40820234725076787, -24.66803830325296687, -341.1985388896944755 ) ) ;
#66688 = CARTESIAN_POINT ( 'NONE',  ( -53.74551868804229571, -284.3471893230417322, -341.8636884958267501 ) ) ;
#66689 = CARTESIAN_POINT ( 'NONE',  ( -60.89598388462611211, -285.1137155922242528, -342.6598846594791894 ) ) ;
#66690 = CARTESIAN_POINT ( 'NONE',  ( -54.77261557253265067, -285.1708422916265135, -199.3153977015881537 ) ) ;
#66691 = CARTESIAN_POINT ( 'NONE',  ( -109.0623672766620729, -277.1790428158155351, -252.9661094684980753 ) ) ;
#66692 = CARTESIAN_POINT ( 'NONE',  ( -106.3536204270571375, -286.0511008532281494, -297.8545499948111797 ) ) ;
#66693 = CARTESIAN_POINT ( 'NONE',  ( -89.95515244568397861, -277.7726323302619562, -218.6890878146726322 ) ) ;
#66694 = CARTESIAN_POINT ( 'NONE',  ( -11.13073371842595627, -277.7819877096691243, -338.8243293707045041 ) ) ;
#66695 = DIRECTION ( 'NONE',  ( -0.000000000000000000, -1.000000000000000000, -0.000000000000000000 ) ) ;
#66696 = CARTESIAN_POINT ( 'NONE',  ( -54.23184288650222129, -274.3216581455266692, -199.2786903435467707 ) ) ;
#66697 = CARTESIAN_POINT ( 'NONE',  ( 36.32680637813746216, -282.6316718168910143, -292.3870917561814053 ) ) ;
#66698 = CARTESIAN_POINT ( 'NONE',  ( 0.8432681186432263720, -283.0493417035392554, -337.1703136565325849 ) ) ;
#66699 = ORIENTED_EDGE ( 'NONE', *, *, #84888, .T. ) ;
#66700 = ORIENTED_EDGE ( 'NONE', *, *, #8700, .T. ) ;
#66701 = CARTESIAN_POINT ( 'NONE',  ( 193.5659903145831038, 250.0000000000000568, 16.24901362097127233 ) ) ;
#66702 = CARTESIAN_POINT ( 'NONE',  ( 32.90612757349362028, -289.7803605344437869, -298.8831495163289560 ) ) ;
#66703 = CARTESIAN_POINT ( 'NONE',  ( -100.0298913023517429, -296.2683635824841986, -232.5426995085460646 ) ) ;
#66704 = CARTESIAN_POINT ( 'NONE',  ( 15.37433248308129308, -292.1220328462279667, -214.3028865048143814 ) ) ;
#66705 = CARTESIAN_POINT ( 'NONE',  ( 18.33677346312641987, -286.7142773349410731, -318.7139422826398913 ) ) ;
#66706 = CARTESIAN_POINT ( 'NONE',  ( -34.57387675725116338, -287.5915584499234114, -343.9482619998299242 ) ) ;
#66707 = CARTESIAN_POINT ( 'NONE',  ( 18.95650955822851458, -288.0921982289884227, -223.2496955252817088 ) ) ;
#66708 = CARTESIAN_POINT ( 'NONE',  ( -93.72452607665498192, -275.8649272248415514, -319.8179434850908365 ) ) ;
#66709 = CARTESIAN_POINT ( 'NONE',  ( -15.20433921795632592, -287.1701872580026134, -343.3297796228917491 ) ) ;
#66710 = CARTESIAN_POINT ( 'NONE',  ( -40.75171745722013128, -288.0095491815368973, -195.3878388967245598 ) ) ;
#66711 = CARTESIAN_POINT ( 'NONE',  ( -23.67098173512307824, -286.8778148181965548, -344.3269977883953175 ) ) ;
#66712 = AXIS2_PLACEMENT_3D ( 'NONE', #3395, #32284, #61191 ) ;
#66713 = CARTESIAN_POINT ( 'NONE',  ( 7.948848076696403808, -283.3573060838906486, -327.9773882919641323 ) ) ;
#66714 = CARTESIAN_POINT ( 'NONE',  ( -73.81221612591677683, -293.5691591439108947, -204.6349444228563357 ) ) ;
#66715 = CARTESIAN_POINT ( 'NONE',  ( 208.4306832106271088, -44.55766379199612004, -7.500000000000012434 ) ) ;
#66716 = CARTESIAN_POINT ( 'NONE',  ( 197.2116943569230898, 214.9331615741067765, -12.42446933126075592 ) ) ;
#66717 = CARTESIAN_POINT ( 'NONE',  ( -92.62617576607279091, -299.1884703524148108, -218.7780632528977662 ) ) ;
#66718 = CARTESIAN_POINT ( 'NONE',  ( -51.84940131230460736, -279.0590405015331612, -198.6006392681399291 ) ) ;
#66719 = CARTESIAN_POINT ( 'NONE',  ( 9.010565118092618064, -280.4163668864175634, -329.3890097020399139 ) ) ;
#66720 = CARTESIAN_POINT ( 'NONE',  ( 25.57654286247664643, -293.3340608566641663, -314.4913720465977462 ) ) ;
#66721 = CARTESIAN_POINT ( 'NONE',  ( -60.75055225159313466, -296.1433127619204129, -200.3180259472798070 ) ) ;
#66722 = CARTESIAN_POINT ( 'NONE',  ( 16.62533118532242682, -274.3568591648520396, -321.6336616008841247 ) ) ;
#66723 = CARTESIAN_POINT ( 'NONE',  ( -84.78376024725687898, -297.0371047690934461, -326.5571878338938632 ) ) ;
#66724 = CARTESIAN_POINT ( 'NONE',  ( 206.6165621753558526, 0.01303144969186966970, 7.291618491801075130 ) ) ;
#66725 = CARTESIAN_POINT ( 'NONE',  ( -78.50871170176674241, -272.0842206655200926, -205.9881154884022010 ) ) ;
#66726 = CARTESIAN_POINT ( 'NONE',  ( -111.8901102181933567, -294.9793387879476541, -255.5800720510984547 ) ) ;
#66727 = CARTESIAN_POINT ( 'NONE',  ( 21.81083818433715393, -295.5862676791116996, -314.1372773570800518 ) ) ;
#66728 = DIRECTION ( 'NONE',  ( 0.000000000000000000, 0.000000000000000000, 1.000000000000000000 ) ) ;
#66729 = CARTESIAN_POINT ( 'NONE',  ( -3.059060201505739318, -295.3897480925137415, -334.9931713849321113 ) ) ;
#66730 = DIRECTION ( 'NONE',  ( 0.000000000000000000, 0.7071067811865474617, 0.7071067811865474617 ) ) ;
#66732 = CARTESIAN_POINT ( 'NONE',  ( -96.40841390429547175, -295.9515655637036389, -313.2791125579200298 ) ) ;
#66731 = CARTESIAN_POINT ( 'NONE',  ( -75.25685377393928377, -283.5699375086498435, -205.1792469172315236 ) ) ;
#66733 = CARTESIAN_POINT ( 'NONE',  ( -99.78847660527259222, -283.9538283504805349, -315.4990862996025385 ) ) ;
#66734 = CARTESIAN_POINT ( 'NONE',  ( -34.00381809868024874, -282.0139860387562294, -194.8748759016867211 ) ) ;
#66735 = CARTESIAN_POINT ( 'NONE',  ( -2.228762407993491124, -286.1707241459696434, -201.8421655686406666 ) ) ;
#66736 = CARTESIAN_POINT ( 'NONE',  ( -63.41624496468342898, -289.7114337277871527, -200.2173617543675732 ) ) ;
#66737 = ADVANCED_FACE ( 'NONE', ( #7419 ), #6636, .T. ) ;
#66738 = CARTESIAN_POINT ( 'NONE',  ( -37.30987171927208834, -271.5523547857346784, -195.3611179825600175 ) ) ;
#66739 = CARTESIAN_POINT ( 'NONE',  ( -17.01954791531377609, -285.0047789399824296, -199.6803399071605440 ) ) ;
#66740 = CARTESIAN_POINT ( 'NONE',  ( -111.2477783009753836, -289.2148846050994280, -290.8399880543827862 ) ) ;
#66741 = DIRECTION ( 'NONE',  ( 0.000000000000000000, 0.000000000000000000, 1.000000000000000000 ) ) ;
#66742 = CARTESIAN_POINT ( 'NONE',  ( -110.5323212056413240, -298.2808308655049814, -260.5099338820116941 ) ) ;
#66743 = CARTESIAN_POINT ( 'NONE',  ( -107.0311960033911873, -279.5726451904997134, -301.8263652807584663 ) ) ;
#66745 = CARTESIAN_POINT ( 'NONE',  ( 7.158569387886407398, -280.3439879132166084, -212.4022905858366812 ) ) ;
#66744 = CARTESIAN_POINT ( 'NONE',  ( 28.13278233394262173, -292.0684992701981741, -307.7692669019813820 ) ) ;
#66746 = CARTESIAN_POINT ( 'NONE',  ( -39.10571175695683621, -295.2403958382071778, -347.3409092754811240 ) ) ;
#66747 = CARTESIAN_POINT ( 'NONE',  ( -37.94592848949424280, -284.1244890159491661, -194.8035299426656195 ) ) ;
#66748 = CARTESIAN_POINT ( 'NONE',  ( -107.7380240075472244, -280.8897397479200890, -244.3390825784085791 ) ) ;
#66749 = CARTESIAN_POINT ( 'NONE',  ( -4.241001199789314668, -293.6634512845080280, -335.7031955238873024 ) ) ;
#66750 = CARTESIAN_POINT ( 'NONE',  ( -109.2750270191963580, -270.8344936132971270, -248.3745720545137772 ) ) ;
#66751 = EDGE_LOOP ( 'NONE', ( #28911, #12974, #53649 ) ) ;
#66752 = LINE ( 'NONE', #65857, #65053 ) ;
#66753 = CARTESIAN_POINT ( 'NONE',  ( 30.45628928834290861, -283.1185492304643958, -239.0078743276770865 ) ) ;
#66754 = CARTESIAN_POINT ( 'NONE',  ( -72.15942204334145060, -295.0334859749779639, -334.6071260114547385 ) ) ;
#66755 = DIRECTION ( 'NONE',  ( 0.000000000000000000, 0.000000000000000000, 1.000000000000000000 ) ) ;
#66756 = CARTESIAN_POINT ( 'NONE',  ( -54.49178911615187104, -280.7666405000204009, -345.3538533559490702 ) ) ;
#66757 = CARTESIAN_POINT ( 'NONE',  ( -63.49251044722220882, -272.9170078647272817, -198.1095163396097973 ) ) ;
#66758 = CARTESIAN_POINT ( 'NONE',  ( 27.03893497890713959, -289.4141400277896992, -311.7920166814591312 ) ) ;
#66759 = CARTESIAN_POINT ( 'NONE',  ( -74.97778835006916154, -291.3694006683082875, -207.7519247701086442 ) ) ;
#66760 = CARTESIAN_POINT ( 'NONE',  ( -32.94076872930077116, -281.6287284087828766, -196.7993102558860983 ) ) ;
#66761 = CARTESIAN_POINT ( 'NONE',  ( -89.82526302268895790, -274.8961100652074379, -218.4774400045996003 ) ) ;
#66762 = CARTESIAN_POINT ( 'NONE',  ( -38.34393925807676595, -278.8342387412107541, -196.9584190451636232 ) ) ;
#66763 = CARTESIAN_POINT ( 'NONE',  ( 25.67839293862412120, -278.1013100876400586, -311.1197902605612740 ) ) ;
#66764 = EDGE_LOOP ( 'NONE', ( #90459, #73802, #64471, #88072, #13817, #55385 ) ) ;
#66765 = CARTESIAN_POINT ( 'NONE',  ( 21.85221839399833499, -274.7231276717928949, -221.1160165558101767 ) ) ;
#66766 = CARTESIAN_POINT ( 'NONE',  ( 13.87657676184798738, -294.6974971904480185, -216.3425812706616682 ) ) ;
#66767 = DIRECTION ( 'NONE',  ( 0.000000000000000000, 0.000000000000000000, 1.000000000000000000 ) ) ;
#66768 = CARTESIAN_POINT ( 'NONE',  ( 188.7149167944524493, -12.49482340714361506, 13.00000000000000178 ) ) ;
#66769 = CARTESIAN_POINT ( 'NONE',  ( 35.89480652357097057, -291.4442121337436333, -250.9017380571721958 ) ) ;
#66770 = CARTESIAN_POINT ( 'NONE',  ( -63.08294680178118341, -297.3743099841260005, -201.9740623292235284 ) ) ;
#66771 = CARTESIAN_POINT ( 'NONE',  ( 175.2296996224750103, 275.5000000000000568, 0.000000000000000000 ) ) ;
#66772 = AXIS2_PLACEMENT_3D ( 'NONE', #66955, #87315, #88712 ) ;
#66773 = CARTESIAN_POINT ( 'NONE',  ( -42.03087026812858085, -293.5141712697696335, -194.1986637375347584 ) ) ;
#66774 = CARTESIAN_POINT ( 'NONE',  ( 10.59707575819634329, -277.1948066931274184, -210.1954327657594490 ) ) ;
#66775 = CARTESIAN_POINT ( 'NONE',  ( 34.42101848358568361, -289.2779139193150399, -249.0994495047464170 ) ) ;
#66776 = CARTESIAN_POINT ( 'NONE',  ( 12.96170564915455792, -274.3481182168935106, -325.8353443617008907 ) ) ;
#66777 = CARTESIAN_POINT ( 'NONE',  ( 29.13651351811480694, -277.0264742199000239, -236.8654271353415766 ) ) ;
#66779 = CARTESIAN_POINT ( 'NONE',  ( -30.65371873581474915, -290.2172107132033148, -196.2221599197860087 ) ) ;
#66778 = CIRCLE ( 'NONE', #35018, 4.025000000000000355 ) ;
#66780 = CARTESIAN_POINT ( 'NONE',  ( -88.12141876326258227, -281.2106996960274614, -214.1318937876493749 ) ) ;
#66781 = ORIENTED_EDGE ( 'NONE', *, *, #72094, .T. ) ;
#66782 = CARTESIAN_POINT ( 'NONE',  ( -8.461594524924265670, -282.0123982166359156, -337.5164019799333914 ) ) ;
#66783 = CARTESIAN_POINT ( 'NONE',  ( -112.4177867730260800, -279.8291844199134744, -254.6429016545420154 ) ) ;
#66784 = CARTESIAN_POINT ( 'NONE',  ( -50.04286232407507384, -282.0055599113663334, -345.9573482249328436 ) ) ;
#66785 = CARTESIAN_POINT ( 'NONE',  ( -77.68102657602891270, -278.5205858967833024, -335.7341309429302783 ) ) ;
#66786 = CARTESIAN_POINT ( 'NONE',  ( 28.50749117222059681, -277.5786736424022365, -308.9174631994290507 ) ) ;
#66787 = CARTESIAN_POINT ( 'NONE',  ( 7.399455738971494334, -283.1948066931273615, -214.2051214447836571 ) ) ;
#66788 = ORIENTED_EDGE ( 'NONE', *, *, #11852, .F. ) ;
#66789 = CARTESIAN_POINT ( 'NONE',  ( -104.5493569401108829, -298.1117102138980499, -303.7670087738766256 ) ) ;
#66790 = CARTESIAN_POINT ( 'NONE',  ( -82.72691286868111149, -290.7692845221287712, -327.9320180720994244 ) ) ;
#66791 = CARTESIAN_POINT ( 'NONE',  ( -107.8254883898565879, -276.2507622517907748, -295.0920485928824064 ) ) ;
#66792 = CARTESIAN_POINT ( 'NONE',  ( -38.87693049490011532, -290.8312997388157441, -346.3322775390297465 ) ) ;
#66793 = CARTESIAN_POINT ( 'NONE',  ( -93.51284384142114448, -290.5637697198045544, -223.5580854985755650 ) ) ;
#66794 = CARTESIAN_POINT ( 'NONE',  ( -5.657569261768225388, -288.1541658785433242, -340.4727629119571475 ) ) ;
#66795 = CARTESIAN_POINT ( 'NONE',  ( 209.4486294747436261, 36.74096400909239435, 13.09663628362915055 ) ) ;
#66796 = CARTESIAN_POINT ( 'NONE',  ( -102.4868907441952928, -282.4833049739951889, -305.1476620427841908 ) ) ;
#66797 = CARTESIAN_POINT ( 'NONE',  ( -97.54672305710471392, -291.8152614121597708, -313.7917603447917827 ) ) ;
#66798 = CARTESIAN_POINT ( 'NONE',  ( -106.8339590332081457, -282.7069109963416054, -295.0393749829704007 ) ) ;
#66799 = CARTESIAN_POINT ( 'NONE',  ( 36.19649311150399740, -282.8796814814920140, -271.3034798066948383 ) ) ;
#66800 = CARTESIAN_POINT ( 'NONE',  ( -36.07865563205614023, -289.9779596449803307, -347.1285035105844372 ) ) ;
#66801 = CARTESIAN_POINT ( 'NONE',  ( -107.1735840877335590, -278.7581654899304340, -292.0129478101076757 ) ) ;
#66802 = CARTESIAN_POINT ( 'NONE',  ( 3.940539295488321159, -291.3894212940592752, -205.7708353016273293 ) ) ;
#66803 = CARTESIAN_POINT ( 'NONE',  ( 32.56086856997399792, -287.9448447371245834, -238.3302530837080155 ) ) ;
#66804 = CARTESIAN_POINT ( 'NONE',  ( -8.250585376719735464, -289.1736423544753052, -341.6020112660514769 ) ) ;
#66805 = CARTESIAN_POINT ( 'NONE',  ( -108.0927015866721490, -284.4815127564268096, -288.3415461514354661 ) ) ;
#66806 = ORIENTED_EDGE ( 'NONE', *, *, #69037, .T. ) ;
#66807 = DIRECTION ( 'NONE',  ( 0.000000000000000000, -0.2502735790305594676, -0.9681751575201846816 ) ) ;
#66808 = CARTESIAN_POINT ( 'NONE',  ( -53.15501775893466174, -293.7120492957038209, -196.2113074505303132 ) ) ;
#66809 = CARTESIAN_POINT ( 'NONE',  ( 35.01451407175223807, -292.5541256450414380, -295.3804821535210863 ) ) ;
#66810 = CARTESIAN_POINT ( 'NONE',  ( -29.70075624538922909, -276.0119215304806630, -343.2477860638952052 ) ) ;
#66811 = CARTESIAN_POINT ( 'NONE',  ( -101.4601106621486224, -296.4601683663465224, -227.8854986308761283 ) ) ;
#66812 = CARTESIAN_POINT ( 'NONE',  ( 13.39438997519455121, -291.2577753230997359, -216.9143508928158894 ) ) ;
#66813 = CARTESIAN_POINT ( 'NONE',  ( -58.16875831301216238, -296.0191570815654813, -199.3385324285015088 ) ) ;
#66814 = CARTESIAN_POINT ( 'NONE',  ( -94.61031751668357970, -292.4026886597474117, -224.4343232609355709 ) ) ;
#66815 = CARTESIAN_POINT ( 'NONE',  ( 19.94389446515256026, -295.2754580729890677, -316.1259345595842660 ) ) ;
#66816 = CARTESIAN_POINT ( 'NONE',  ( -25.22895927321087228, -292.8980477503152429, -344.5981907666093207 ) ) ;
#66817 = CARTESIAN_POINT ( 'NONE',  ( 60.19128830256915563, -301.2732859087743691, -195.3278605009263060 ) ) ;
#66818 = CARTESIAN_POINT ( 'NONE',  ( 25.90528312414506118, -288.9997458554204854, -307.3833121448694214 ) ) ;
#66819 = CARTESIAN_POINT ( 'NONE',  ( 22.23351816859807428, -278.1618069544609853, -316.5253106550804887 ) ) ;
#66820 = CARTESIAN_POINT ( 'NONE',  ( -112.5085079222426003, -277.4173112377816892, -256.0345818978447028 ) ) ;
#66821 = CARTESIAN_POINT ( 'NONE',  ( -76.37382014607375424, -272.8935266381818110, -204.0439799770036586 ) ) ;
#66822 = CARTESIAN_POINT ( 'NONE',  ( 4.173423967329497941, -280.5681187145156059, -332.2118747651024933 ) ) ;
#66823 = CARTESIAN_POINT ( 'NONE',  ( -111.4025260527821501, -276.7247644265662530, -288.3444230124958381 ) ) ;
#66824 = CARTESIAN_POINT ( 'NONE',  ( -108.6493845057013488, -295.4707646075503362, -252.5203891492550667 ) ) ;
#66825 = CARTESIAN_POINT ( 'NONE',  ( -94.72225332419415622, -275.2202216751836659, -222.0458084243138330 ) ) ;
#66826 = CARTESIAN_POINT ( 'NONE',  ( 11.60863304955299213, -275.4040876644211266, -215.9997109070220063 ) ) ;
#66827 = DIRECTION ( 'NONE',  ( 1.124465274301078281E-16, 1.000000000000000000, -0.000000000000000000 ) ) ;
#66828 = AXIS2_PLACEMENT_3D ( 'NONE', #87858, #37225, #9253 ) ;
#66829 = CARTESIAN_POINT ( 'NONE',  ( -108.8616546510138221, -288.8794171114324172, -246.4639909370486066 ) ) ;
#66830 = VECTOR ( 'NONE', #25148, 1000.000000000000000 ) ;
#66831 = CARTESIAN_POINT ( 'NONE',  ( -57.29089898836343053, -289.3025524128559596, -344.7871143467750130 ) ) ;
#66832 = CARTESIAN_POINT ( 'NONE',  ( 0.2558075010870646260, -276.5517316177546832, -205.2581371564674555 ) ) ;
#66833 = CARTESIAN_POINT ( 'NONE',  ( -110.3868204106277204, -294.3427326982731529, -286.6226933687775613 ) ) ;
#66834 = EDGE_CURVE ( 'NONE', #50388, #6488, #6037, .T. ) ;
#66835 = CARTESIAN_POINT ( 'NONE',  ( -1.718098331928909372, -281.7894003285283020, -338.4428175501761302 ) ) ;
#66836 = ADVANCED_FACE ( 'NONE', ( #57175 ), #92654, .F. ) ;
#66837 = FACE_OUTER_BOUND ( 'NONE', #41234, .T. ) ;
#66838 = AXIS2_PLACEMENT_3D ( 'NONE', #41192, #3846, #48785 ) ;
#66839 = CARTESIAN_POINT ( 'NONE',  ( 19.42697874413789449, -280.2317892636173156, -319.3938110875790812 ) ) ;
#66840 = CARTESIAN_POINT ( 'NONE',  ( 0.000000000000000000, 3.000000000000000000, -9.000000000000001776 ) ) ;
#66841 = CARTESIAN_POINT ( 'NONE',  ( -57.75071423307057472, -290.5777154140786251, -199.8054558447315969 ) ) ;
#66842 = CARTESIAN_POINT ( 'NONE',  ( -57.71094265623317199, -283.9260509383547628, -198.9216310065164066 ) ) ;
#66843 = CARTESIAN_POINT ( 'NONE',  ( 199.8090428944973382, 41.61473866538664623, 10.14950798386179009 ) ) ;
#66844 = DIRECTION ( 'NONE',  ( 0.000000000000000000, 0.000000000000000000, 1.000000000000000000 ) ) ;
#66845 = CARTESIAN_POINT ( 'NONE',  ( 37.64040703607278715, -291.5935751674341532, -273.6000701297232354 ) ) ;
#66846 = CARTESIAN_POINT ( 'NONE',  ( -54.11617747601757600, -278.8711408014724498, -342.2821602979754516 ) ) ;
#66847 = CARTESIAN_POINT ( 'NONE',  ( -33.06549193672525178, -284.2045168166098961, -346.8576654642611174 ) ) ;
#66849 = CARTESIAN_POINT ( 'NONE',  ( -87.69450223319059035, -285.3246945150340821, -217.5066449441906968 ) ) ;
#66848 = CARTESIAN_POINT ( 'NONE',  ( 13.02320048660527974, -272.8285620592045575, -213.9645318959786948 ) ) ;
#66850 = CARTESIAN_POINT ( 'NONE',  ( 3.475893269915882211, -277.9165547436763291, -331.5926375238618107 ) ) ;
#66851 = CARTESIAN_POINT ( 'NONE',  ( 20.97180314478336172, -276.9744973678308497, -314.5441131671724406 ) ) ;
#66852 = CARTESIAN_POINT ( 'NONE',  ( -70.21325028285555447, -287.6191410338793162, -202.9484942099033162 ) ) ;
#66853 = ORIENTED_EDGE ( 'NONE', *, *, #11054, .T. ) ;
#66854 = FACE_OUTER_BOUND ( 'NONE', #39932, .T. ) ;
#66855 = CARTESIAN_POINT ( 'NONE',  ( -97.40877091635981344, -295.7397667153531415, -318.5581936505013800 ) ) ;
#66856 = CARTESIAN_POINT ( 'NONE',  ( -42.81943693280844343, -287.9626094766422852, -195.9046641415179124 ) ) ;
#66857 = CARTESIAN_POINT ( 'NONE',  ( 222.4306832106270804, -134.2391364535880882, -21.50000000000000000 ) ) ;
#66858 = CARTESIAN_POINT ( 'NONE',  ( -19.05039376806006857, -289.7666405000204009, -190.3683826091709363 ) ) ;
#66859 = CARTESIAN_POINT ( 'NONE',  ( -108.2217078181806329, -277.8461775948298964, -241.0777264638954875 ) ) ;
#66860 = CARTESIAN_POINT ( 'NONE',  ( -74.27313864602086824, -289.9694517170592576, -203.7089667408608591 ) ) ;
#66861 = CARTESIAN_POINT ( 'NONE',  ( -42.74409273166229184, -287.5029134548743173, -196.8533256199991115 ) ) ;
#66862 = CARTESIAN_POINT ( 'NONE',  ( -110.4901901947326905, -280.1655134037587231, -281.6426256381563462 ) ) ;
#66863 = CARTESIAN_POINT ( 'NONE',  ( 26.63442371319922941, -288.4242674244037516, -228.5799993914037316 ) ) ;
#66864 = CARTESIAN_POINT ( 'NONE',  ( -26.42722136458372972, -284.9135586049499693, -344.6154075554599672 ) ) ;
#66865 = CARTESIAN_POINT ( 'NONE',  ( 22.64233765057464609, -276.3660845546355631, -318.6615273389513163 ) ) ;
#66866 = CARTESIAN_POINT ( 'NONE',  ( -52.95506504555213922, -295.8712886083820308, -197.3144395312322104 ) ) ;
#66867 = CARTESIAN_POINT ( 'NONE',  ( -56.55460229822654128, -279.6445882519741417, -195.7416199393135230 ) ) ;
#66868 = CARTESIAN_POINT ( 'NONE',  ( -109.8857681398556423, -298.6882604995303723, -253.6676342733145759 ) ) ;
#66869 = CARTESIAN_POINT ( 'NONE',  ( 156.4892692376083971, 15.19211566834788485, 9.995848581180753811 ) ) ;
#66870 = CARTESIAN_POINT ( 'NONE',  ( 39.58706461736021254, -278.0519495502701943, -270.3284710469133074 ) ) ;
#66871 = CARTESIAN_POINT ( 'NONE',  ( -35.52524190666022008, -272.3144843020784833, -194.3832051352771657 ) ) ;
#66872 = EDGE_CURVE ( 'NONE', #44128, #59550, #27825, .T. ) ;
#66873 = CARTESIAN_POINT ( 'NONE',  ( 151.9709352735115147, -299.5541904835127980, -195.3611179825600175 ) ) ;
#66874 = CARTESIAN_POINT ( 'NONE',  ( -85.15024169605698035, -277.2407497297832606, -325.6760518972466798 ) ) ;
#66875 = CARTESIAN_POINT ( 'NONE',  ( -60.76438287097140289, -274.9600488305526369, -197.3716450990360727 ) ) ;
#66876 = CARTESIAN_POINT ( 'NONE',  ( 0.7411836450362718764, -281.6159739079147357, -337.0284904910478758 ) ) ;
#66877 = CARTESIAN_POINT ( 'NONE',  ( -2.874775822079837617, -290.3505950851243824, -335.9160213339897609 ) ) ;
#66878 = CARTESIAN_POINT ( 'NONE',  ( -84.80046405501836659, -298.9313138850195060, -210.6085157178228826 ) ) ;
#66879 = CARTESIAN_POINT ( 'NONE',  ( -97.92940309623408268, -298.3864361357140069, -223.4662933586699296 ) ) ;
#66880 = CARTESIAN_POINT ( 'NONE',  ( -37.58074946566359387, -294.0493461499370937, -195.5154062998323354 ) ) ;
#66881 = CARTESIAN_POINT ( 'NONE',  ( 22.46000633220254983, -280.1684892219421954, -315.3687749933597502 ) ) ;
#66882 = CARTESIAN_POINT ( 'NONE',  ( 23.27210241904560561, -282.8803055347647728, -227.1490694301642179 ) ) ;
#66883 = CARTESIAN_POINT ( 'NONE',  ( -3.333295855144573050, -272.5235449935348697, -203.8992293558194433 ) ) ;
#66884 = CARTESIAN_POINT ( 'NONE',  ( -100.7420801062649787, -285.5889673348611382, -312.7266960608000659 ) ) ;
#66885 = CARTESIAN_POINT ( 'NONE',  ( -39.98294687965398708, -288.0063123397029017, -343.6724244598802329 ) ) ;
#66886 = CARTESIAN_POINT ( 'NONE',  ( 155.1585690732346450, 206.2207167234212193, -217.1754125233248374 ) ) ;
#66887 = ORIENTED_EDGE ( 'NONE', *, *, #82549, .T. ) ;
#66888 = CARTESIAN_POINT ( 'NONE',  ( -31.88710179228944952, -287.5594633726584561, -346.6291079395904262 ) ) ;
#66889 = CARTESIAN_POINT ( 'NONE',  ( 3.622960444184753381, -288.1511743511123314, -330.8702800020743666 ) ) ;
#66890 = ORIENTED_EDGE ( 'NONE', *, *, #83986, .T. ) ;
#66891 = CARTESIAN_POINT ( 'NONE',  ( -16.21374430696123881, -283.8650357875006307, -344.1393293041872425 ) ) ;
#66892 = CARTESIAN_POINT ( 'NONE',  ( 30.29921685870103332, -276.2554330213101821, -298.0055659719299683 ) ) ;
#66893 = CARTESIAN_POINT ( 'NONE',  ( -58.83881269432927041, -290.7007250168816768, -196.7447702036221813 ) ) ;
#66894 = CARTESIAN_POINT ( 'NONE',  ( 38.69266256807665627, -282.0553151159350023, -258.5230288893407646 ) ) ;
#66895 = CARTESIAN_POINT ( 'NONE',  ( 18.63824324903709950, -282.3594468031603810, -218.5059958408970715 ) ) ;
#66896 = CARTESIAN_POINT ( 'NONE',  ( -97.15328148535061814, -284.2350876661647021, -318.8412887183046109 ) ) ;
#66897 = CARTESIAN_POINT ( 'NONE',  ( -30.26238517892669577, -280.1440608554726737, -197.6548388104711478 ) ) ;
#66898 = CARTESIAN_POINT ( 'NONE',  ( -53.35057174420112602, -292.7666405000204577, -340.3538533559490702 ) ) ;
#66899 = CARTESIAN_POINT ( 'NONE',  ( -113.6817389704806232, -274.0367189774781309, -270.3800200741469553 ) ) ;
#66900 = VERTEX_POINT ( 'NONE', #65217 ) ;
#66901 = VECTOR ( 'NONE', #74134, 1000.000000000000000 ) ;
#66902 = CARTESIAN_POINT ( 'NONE',  ( 37.53361432508727802, -277.5681354020764502, -271.5902829283072037 ) ) ;
#66903 = CARTESIAN_POINT ( 'NONE',  ( -84.83675082977744353, -218.8559137767458367, -351.9183727634863885 ) ) ;
#66904 = CIRCLE ( 'NONE', #39629, 2.046895004029262832 ) ;
#66905 = CARTESIAN_POINT ( 'NONE',  ( -55.31070341228750920, -297.1635380649868807, -199.4496675265181693 ) ) ;
#66906 = CARTESIAN_POINT ( 'NONE',  ( 38.75475483610038197, -293.2018864487969836, -281.7126132640497644 ) ) ;
#66907 = CARTESIAN_POINT ( 'NONE',  ( -81.97344496812658576, -219.2901136445231316, -349.2013451768860364 ) ) ;
#66908 = CIRCLE ( 'NONE', #86561, 2.500000000000008882 ) ;
#66910 = CARTESIAN_POINT ( 'NONE',  ( -13.04349295403358866, -287.1309604114507010, -340.0463929163666990 ) ) ;
#66909 = CARTESIAN_POINT ( 'NONE',  ( -70.45713483483130801, -296.1988329782084861, -201.4991235301377799 ) ) ;
#66911 = CARTESIAN_POINT ( 'NONE',  ( -99.75924385471867595, -297.8645385357791042, -310.6412569139009747 ) ) ;
#66912 = CARTESIAN_POINT ( 'NONE',  ( 17.24575557252470759, -288.1672371298577104, -221.1340723638584507 ) ) ;
#66913 = VERTEX_POINT ( 'NONE', #64761 ) ;
#66914 = CARTESIAN_POINT ( 'NONE',  ( -36.26568712721649490, -295.9802549357141288, -347.1313467208539691 ) ) ;
#66915 = AXIS2_PLACEMENT_3D ( 'NONE', #30583, #88793, #59484 ) ;
#66916 = CARTESIAN_POINT ( 'NONE',  ( -108.7263763185654284, -285.2504037482521539, -254.7393821814821138 ) ) ;
#66917 = CARTESIAN_POINT ( 'NONE',  ( -60.01583976572951684, -296.5597358308956473, -197.1355909887807059 ) ) ;
#66918 = CARTESIAN_POINT ( 'NONE',  ( -0.8894949029108201177, -293.3264616937420328, -202.7194477265767887 ) ) ;
#66919 = CARTESIAN_POINT ( 'NONE',  ( 39.59422962047796801, -294.0078450261160583, -267.4326853852362547 ) ) ;
#66920 = CARTESIAN_POINT ( 'NONE',  ( -106.5719643720372716, -291.0263627114725864, -247.2057618589018944 ) ) ;
#66921 = EDGE_LOOP ( 'NONE', ( #12390, #71838, #72939, #33722 ) ) ;
#66922 = PLANE ( 'NONE',  #30675 ) ;
#66923 = CARTESIAN_POINT ( 'NONE',  ( -112.9017001288127346, -274.4719972107771468, -270.3855110958305090 ) ) ;
#66924 = CARTESIAN_POINT ( 'NONE',  ( 26.60757217046068845, -273.7896616436511863, -228.1888606222470059 ) ) ;
#66925 = ORIENTED_EDGE ( 'NONE', *, *, #64104, .T. ) ;
#66926 = CARTESIAN_POINT ( 'NONE',  ( -45.64920957719182582, -276.6622845402636699, -346.9027751304702178 ) ) ;
#66927 = CARTESIAN_POINT ( 'NONE',  ( -79.29326907088395160, -271.8756530370084192, -209.5824471396249180 ) ) ;
#66928 = CARTESIAN_POINT ( 'NONE',  ( -109.6847239637551041, -280.1958005568909016, -287.0712763307971613 ) ) ;
#66929 = CARTESIAN_POINT ( 'NONE',  ( -5.772504451945826176, -274.7721814257769779, -337.5632956575348089 ) ) ;
#66930 = CARTESIAN_POINT ( 'NONE',  ( -63.23383045339200947, -298.9124187889054269, -201.6289025273190703 ) ) ;
#66931 = CARTESIAN_POINT ( 'NONE',  ( -89.41788040884343047, -274.2373398920433942, -218.8685952697086634 ) ) ;
#66932 = CARTESIAN_POINT ( 'NONE',  ( -108.2294805023921498, -274.6651982674780470, -242.8501941320334652 ) ) ;
#66933 = CARTESIAN_POINT ( 'NONE',  ( -8.300646040271290715, -272.4504779498249150, -200.7713833410523137 ) ) ;
#66934 = CARTESIAN_POINT ( 'NONE',  ( 18.05509406843059494, -294.8820821946591764, -318.0780878978462169 ) ) ;
#66935 = CARTESIAN_POINT ( 'NONE',  ( -66.78328110061660539, -290.2333653970372893, -202.9180440001503314 ) ) ;
#66936 = CARTESIAN_POINT ( 'NONE',  ( 195.7510731661265595, -164.3527196417747405, 21.50000000000000000 ) ) ;
#66937 = CARTESIAN_POINT ( 'NONE',  ( -2.747158939369240827, -277.0995192502858231, -339.0980127403515212 ) ) ;
#66938 = CARTESIAN_POINT ( 'NONE',  ( -16.64269548449760805, -274.4936814796191697, -200.3044730340681099 ) ) ;
#66939 = CARTESIAN_POINT ( 'NONE',  ( -102.5068597461124966, -282.7097126234372695, -310.4460309048053546 ) ) ;
#66940 = CARTESIAN_POINT ( 'NONE',  ( -110.8140545556915839, -298.7563420454741276, -254.4314279822453386 ) ) ;
#66941 = CARTESIAN_POINT ( 'NONE',  ( 175.2296996224750103, 275.0000000000000568, 0.000000000000000000 ) ) ;
#66942 = CARTESIAN_POINT ( 'NONE',  ( -54.78495104298879426, -285.0194472865028956, -199.2570719344716110 ) ) ;
#66943 = CARTESIAN_POINT ( 'NONE',  ( -104.1662447159930878, -282.0962989774749303, -304.8914503707903236 ) ) ;
#66944 = EDGE_CURVE ( 'NONE', #48610, #33225, #93586, .T. ) ;
#66945 = CARTESIAN_POINT ( 'NONE',  ( -96.92188341286590969, -276.1847858055671736, -314.2933678676043883 ) ) ;
#66946 = CARTESIAN_POINT ( 'NONE',  ( -64.56789046347860506, -275.9892728393234620, -338.7826994224380428 ) ) ;
#66947 = CARTESIAN_POINT ( 'NONE',  ( 33.90511230064365833, -283.2477437889155567, -246.7694381402021691 ) ) ;
#66948 = CARTESIAN_POINT ( 'NONE',  ( 35.77230737555238704, -276.6654787420447974, -263.3677301236903645 ) ) ;
#66949 = CARTESIAN_POINT ( 'NONE',  ( 164.2231345125756263, 300.2961574867697436, -7.500000000000000000 ) ) ;
#66950 = CARTESIAN_POINT ( 'NONE',  ( -0.4150895636654400311, -272.9344185597497585, -203.6914525832594620 ) ) ;
#66951 = CARTESIAN_POINT ( 'NONE',  ( 9.656385950408930441, -282.6968129654923132, -211.6326093896558120 ) ) ;
#66952 = EDGE_CURVE ( 'NONE', #43263, #70876, #50515, .T. ) ;
#66953 = DIRECTION ( 'NONE',  ( -0.000000000000000000, 1.000000000000000000, -0.000000000000000000 ) ) ;
#66954 = CARTESIAN_POINT ( 'NONE',  ( 23.52844107698648557, -288.8662780168637596, -225.5934945264107228 ) ) ;
#66955 = CARTESIAN_POINT ( 'NONE',  ( 196.7510731661265595, -143.7221692137691775, 21.50000000000000000 ) ) ;
#66956 = CARTESIAN_POINT ( 'NONE',  ( -92.28431649405821702, -287.8371035508541809, -321.4873099704672086 ) ) ;
#66957 = FACE_OUTER_BOUND ( 'NONE', #46030, .T. ) ;
#66958 = CARTESIAN_POINT ( 'NONE',  ( -71.83812560875631448, -296.3804402151587283, -205.5616057012519491 ) ) ;
#66959 = CARTESIAN_POINT ( 'NONE',  ( -100.7546451304853576, -289.2144811071910340, -231.7649538593386183 ) ) ;
#66960 = CARTESIAN_POINT ( 'NONE',  ( -51.00049622308160480, -154.6998088915060237, -359.8797964913271130 ) ) ;
#66961 = CARTESIAN_POINT ( 'NONE',  ( -44.74174808262339553, -295.9584584443144308, -195.6753159266001205 ) ) ;
#66962 = CARTESIAN_POINT ( 'NONE',  ( 32.22478160262502911, -286.4362108120465109, -301.7173353969674849 ) ) ;
#66963 = CARTESIAN_POINT ( 'NONE',  ( -15.88060979045458154, -284.3700096286873418, -340.9717546821901237 ) ) ;
#66964 = CARTESIAN_POINT ( 'NONE',  ( -109.0139266078943479, -283.1146767995436448, -245.1209522924006592 ) ) ;
#66965 = CARTESIAN_POINT ( 'NONE',  ( -90.75918558089340138, -291.2677466969161628, -220.5875131363787318 ) ) ;
#66966 = CARTESIAN_POINT ( 'NONE',  ( 34.51970584627218841, -283.1848775805641480, -286.2139805139627811 ) ) ;
#66967 = CARTESIAN_POINT ( 'NONE',  ( 32.88673142598792509, -282.0842894519435049, -249.8533358341228450 ) ) ;
#66968 = CARTESIAN_POINT ( 'NONE',  ( -97.69629866007362295, -291.9183837106073156, -315.5015036296520634 ) ) ;
#66969 = AXIS2_PLACEMENT_3D ( 'NONE', #92547, #27715, #71753 ) ;
#66970 = CARTESIAN_POINT ( 'NONE',  ( -60.15011439280849714, -297.9312707115456078, -196.7612125331842492 ) ) ;
#66971 = CIRCLE ( 'NONE', #26132, 25.00000000000000000 ) ;
#66972 = CARTESIAN_POINT ( 'NONE',  ( 34.56964662923419240, -285.9292752154952382, -293.5575057481635213 ) ) ;
#66973 = CARTESIAN_POINT ( 'NONE',  ( 24.36765778347885103, -276.1647972375599238, -316.4149467717384141 ) ) ;
#66974 = CARTESIAN_POINT ( 'NONE',  ( -82.74914644617162196, -293.4082697403888460, -211.0503515312420575 ) ) ;
#66975 = LINE ( 'NONE', #61293, #72664 ) ;
#66976 = CARTESIAN_POINT ( 'NONE',  ( -69.91165696735023971, -282.1233781216988064, -202.8022627189028810 ) ) ;
#66977 = AXIS2_PLACEMENT_3D ( 'NONE', #52008, #82291, #22660 ) ;
#66978 = CARTESIAN_POINT ( 'NONE',  ( -106.9680502258036938, -276.1835217548601236, -298.6842498030480328 ) ) ;
#66979 = DIRECTION ( 'NONE',  ( 0.000000000000000000, -1.000000000000000000, 0.000000000000000000 ) ) ;
#66980 = CARTESIAN_POINT ( 'NONE',  ( -57.16178524344420708, -296.2006026990770238, -196.7292158022059141 ) ) ;
#66981 = CARTESIAN_POINT ( 'NONE',  ( -97.92301971794994131, -272.4696893868625693, -229.3587696319173403 ) ) ;
#66982 = AXIS2_PLACEMENT_3D ( 'NONE', #33791, #19122, #3037 ) ;
#66983 = CARTESIAN_POINT ( 'NONE',  ( -108.7853764634695324, -292.3091231213562082, -252.2401853915949346 ) ) ;
#66984 = CARTESIAN_POINT ( 'NONE',  ( -52.42991519985337590, -292.7955404200284306, -198.6448713283560892 ) ) ;
#66985 = CARTESIAN_POINT ( 'NONE',  ( -99.87536134978427071, -285.7715062841502913, -310.0488776312305390 ) ) ;
#66986 = CARTESIAN_POINT ( 'NONE',  ( -1.099458937905831046, -293.9488008365583482, -203.0922080215096912 ) ) ;
#66987 = CARTESIAN_POINT ( 'NONE',  ( 10.79542237820755801, -294.0166852179127659, -210.8277229195600739 ) ) ;
#66988 = CARTESIAN_POINT ( 'NONE',  ( 10.28991587961307808, -294.2063519485525944, -325.6804560207181680 ) ) ;
#66989 = CARTESIAN_POINT ( 'NONE',  ( 4.757764759355538331, -290.4842402628768809, -332.4933580632563235 ) ) ;
#66990 = CARTESIAN_POINT ( 'NONE',  ( 35.60976771557110965, -282.0310421820111628, -295.1658925406056824 ) ) ;
#66991 = CARTESIAN_POINT ( 'NONE',  ( -101.6577801209563603, -271.2242178407157098, -230.3143037071844788 ) ) ;
#66992 = CARTESIAN_POINT ( 'NONE',  ( -95.81516978679371732, -285.0621525138377024, -220.1827133802016192 ) ) ;
#66993 = AXIS2_PLACEMENT_3D ( 'NONE', #3689, #2751, #76117 ) ;
#66994 = CARTESIAN_POINT ( 'NONE',  ( 17.76202262981522040, -278.2385657843595936, -320.7332088602555586 ) ) ;
#66995 = CARTESIAN_POINT ( 'NONE',  ( -108.7482648970749182, -283.5704796478498224, -253.3296122133066319 ) ) ;
#66996 = CARTESIAN_POINT ( 'NONE',  ( 34.03631996487620626, -285.8492817032945936, -293.3867319003311422 ) ) ;
#66997 = CARTESIAN_POINT ( 'NONE',  ( -38.13285378101332412, -278.1819267755583382, -194.6004450691214629 ) ) ;
#66998 = DIRECTION ( 'NONE',  ( 0.000000000000000000, 0.000000000000000000, 1.000000000000000000 ) ) ;
#66999 = CARTESIAN_POINT ( 'NONE',  ( -104.6518066812248691, -284.4424024861571638, -241.8174135537645384 ) ) ;
#67000 = AXIS2_PLACEMENT_3D ( 'NONE', #17817, #10696, #75574 ) ;
#67001 = CARTESIAN_POINT ( 'NONE',  ( -50.88458104402136684, -281.0878689522181162, -194.9648376097752305 ) ) ;
#67002 = CARTESIAN_POINT ( 'NONE',  ( 38.44072848535298448, -286.7685144958991827, -282.9250486333608592 ) ) ;
#67003 = CARTESIAN_POINT ( 'NONE',  ( 17.85098030138730607, -296.0081874964122903, -319.6929294394686849 ) ) ;
#67004 = CARTESIAN_POINT ( 'NONE',  ( -9.485102557075622443, -278.2942285080972624, -341.2867860252569017 ) ) ;
#67005 = CARTESIAN_POINT ( 'NONE',  ( 21.36306452885605012, -277.5317845536938535, -319.4228024309114176 ) ) ;
#67006 = CARTESIAN_POINT ( 'NONE',  ( -40.50789072475588171, -276.9263566499165563, -343.3048872462796339 ) ) ;
#67007 = CARTESIAN_POINT ( 'NONE',  ( 10.36552654395365991, -300.6508398382715086, -195.5114658272372026 ) ) ;
#67008 = CARTESIAN_POINT ( 'NONE',  ( 31.66192681710618828, -285.1714003743475701, -241.2694682481871382 ) ) ;
#67009 = CARTESIAN_POINT ( 'NONE',  ( -111.2239763421976591, -292.3886879039816904, -251.6577748456057009 ) ) ;
#67010 = CIRCLE ( 'NONE', #56411, 24.50000000000000355 ) ;
#67011 = CARTESIAN_POINT ( 'NONE',  ( 6.235694213800440977, -293.3654088854264046, -329.3755113720337135 ) ) ;
#67012 = ORIENTED_EDGE ( 'NONE', *, *, #27047, .F. ) ;
#67013 = CARTESIAN_POINT ( 'NONE',  ( 27.17476342466528294, -293.6859328467060095, -304.6702287837336485 ) ) ;
#67014 = CARTESIAN_POINT ( 'NONE',  ( -69.50611118704075864, -292.7183612831727828, -200.7268419830291180 ) ) ;
#67015 = CARTESIAN_POINT ( 'NONE',  ( -110.0043858952703602, -279.0922718530686097, -278.8098239488264767 ) ) ;
#67016 = CARTESIAN_POINT ( 'NONE',  ( -102.5129343499546479, -272.1432336441174016, -229.7959797157119510 ) ) ;
#67017 = CARTESIAN_POINT ( 'NONE',  ( 39.50290023730125455, -288.2542591529239075, -274.4092868848603644 ) ) ;
#67018 = CARTESIAN_POINT ( 'NONE',  ( 0.7125367929813983814, -288.8927725998009919, -337.3363715993124856 ) ) ;
#67019 = CARTESIAN_POINT ( 'NONE',  ( -68.78788600754154459, -285.9602766895080208, -204.4441763113638899 ) ) ;
#67020 = CARTESIAN_POINT ( 'NONE',  ( 121.2562179577859354, 149.7689830918628218, -263.4557525057824137 ) ) ;
#67021 = CARTESIAN_POINT ( 'NONE',  ( -23.55173957530102413, -107.6722516029799976, -361.1105106771343571 ) ) ;
#67022 = CARTESIAN_POINT ( 'NONE',  ( -111.3618521999193689, -270.7884898157561793, -270.3386623361540160 ) ) ;
#67023 = CARTESIAN_POINT ( 'NONE',  ( -39.17202761408243106, -276.2728720065729249, -343.4996962346045279 ) ) ;
#67024 = CARTESIAN_POINT ( 'NONE',  ( -76.53263985705950745, -276.5099263182078744, -332.3748119067287803 ) ) ;
#67025 = CARTESIAN_POINT ( 'NONE',  ( -23.36741030153408616, -297.7303750467191321, -193.4237862816653148 ) ) ;
#67026 = CARTESIAN_POINT ( 'NONE',  ( 162.2625608158381851, 217.6175415146854561, -203.0404916468470446 ) ) ;
#67027 = CARTESIAN_POINT ( 'NONE',  ( -95.78339516023345368, -276.5673149934908110, -319.7561003446909922 ) ) ;
#67028 = CARTESIAN_POINT ( 'NONE',  ( 18.79638618443841125, -296.0184493717335386, -321.6480315517689519 ) ) ;
#67029 = ORIENTED_EDGE ( 'NONE', *, *, #16816, .T. ) ;
#67030 = CARTESIAN_POINT ( 'NONE',  ( -100.3538522217745879, -290.5359661716732376, -307.4398937053138070 ) ) ;
#67031 = CARTESIAN_POINT ( 'NONE',  ( -105.1160131458998990, -297.8251019792894567, -234.0432288662204314 ) ) ;
#67032 = CARTESIAN_POINT ( 'NONE',  ( -63.53018616911869287, -274.3710191716231179, -198.0598317881868695 ) ) ;
#67033 = CARTESIAN_POINT ( 'NONE',  ( -110.2415590959016782, -296.6684097743927850, -274.1834951170034742 ) ) ;
#67034 = ORIENTED_EDGE ( 'NONE', *, *, #27704, .T. ) ;
#67035 = DIRECTION ( 'NONE',  ( -1.000000000000000000, -0.000000000000000000, 0.000000000000000000 ) ) ;
#67036 = VECTOR ( 'NONE', #42120, 1000.000000000000000 ) ;
#67037 = CARTESIAN_POINT ( 'NONE',  ( -100.8727300690507747, -279.9242658994360795, -311.3603658274947179 ) ) ;
#67038 = CARTESIAN_POINT ( 'NONE',  ( 26.66720809742409770, -281.6221709145204954, -313.0505378778299246 ) ) ;
#67039 = VECTOR ( 'NONE', #65339, 1000.000000000000000 ) ;
#67040 = CARTESIAN_POINT ( 'NONE',  ( -110.4756489247802307, -279.5562228984588842, -276.1167851085758116 ) ) ;
#67041 = CARTESIAN_POINT ( 'NONE',  ( -113.2189234111708629, -280.2606260639273614, -274.4380038564601705 ) ) ;
#67042 = CARTESIAN_POINT ( 'NONE',  ( -102.6358645727413546, -271.4939527721521699, -236.0837082406988827 ) ) ;
#67043 = DIRECTION ( 'NONE',  ( -1.000000000000000000, 0.000000000000000000, 0.000000000000000000 ) ) ;
#67044 = DIRECTION ( 'NONE',  ( 0.000000000000000000, 0.000000000000000000, 1.000000000000000000 ) ) ;
#67045 = CARTESIAN_POINT ( 'NONE',  ( 25.13518729998423495, -281.1979333874322720, -232.5055345102541082 ) ) ;
#67046 = CIRCLE ( 'NONE', #91217, 5.568361562975243650 ) ;
#67047 = CARTESIAN_POINT ( 'NONE',  ( 34.03805652046323615, -276.7182139850921772, -298.9491097672543560 ) ) ;
#67048 = CARTESIAN_POINT ( 'NONE',  ( 30.72691149552677459, -277.1372324023639635, -238.7468250872570934 ) ) ;
#67049 = CARTESIAN_POINT ( 'NONE',  ( 38.14833764748937028, -273.9767750546992033, -258.4503894650110283 ) ) ;
#67050 = ORIENTED_EDGE ( 'NONE', *, *, #4713, .T. ) ;
#67051 = CARTESIAN_POINT ( 'NONE',  ( 196.4635112535681856, 24.42475431280786680, 11.30725198228063988 ) ) ;
#67052 = CARTESIAN_POINT ( 'NONE',  ( 28.34087215466204768, -284.0229137394446752, -307.4026926134327482 ) ) ;
#67053 = CIRCLE ( 'NONE', #26226, 2.500000000000002220 ) ;
#67054 = CARTESIAN_POINT ( 'NONE',  ( -64.12121758476423850, -290.8908356855160946, -202.2633493847105512 ) ) ;
#67055 = CARTESIAN_POINT ( 'NONE',  ( 9.754876809975540297, -286.0300808005186468, -209.5727537424507148 ) ) ;
#67056 = EDGE_CURVE ( 'NONE', #52349, #64758, #86952, .T. ) ;
#67057 = CARTESIAN_POINT ( 'NONE',  ( -38.92897890924263038, -281.3121561975418672, -344.3700964878531181 ) ) ;
#67059 = CARTESIAN_POINT ( 'NONE',  ( 3.252362589439977469, -284.6821418321059127, -207.9637120391448946 ) ) ;
#67058 = CARTESIAN_POINT ( 'NONE',  ( -48.43527695111280451, -281.7708530120160617, -343.1093651726184817 ) ) ;
#67060 = CARTESIAN_POINT ( 'NONE',  ( -16.82534786963879014, -281.5282079434873594, -199.8897777521180217 ) ) ;
#67061 = CARTESIAN_POINT ( 'NONE',  ( -31.84918176365186682, -124.6684167596312136, -365.2437734796851601 ) ) ;
#67062 = CARTESIAN_POINT ( 'NONE',  ( -78.74234220796599004, -281.9998775941510303, -334.3331997810662983 ) ) ;
#67063 = CARTESIAN_POINT ( 'NONE',  ( -4.091918615892772060, -296.6139714275789743, -337.6022192395366233 ) ) ;
#67065 = CARTESIAN_POINT ( 'NONE',  ( -38.13652149106722078, -278.2821852550586073, -194.3786050189345644 ) ) ;
#67064 = CIRCLE ( 'NONE', #60995, 5.000000000000004441 ) ;
#67066 = CARTESIAN_POINT ( 'NONE',  ( -89.15221949020558156, -278.4558738240499451, -322.0039394398951913 ) ) ;
#67067 = CARTESIAN_POINT ( 'NONE',  ( -79.92116755735197842, -287.4782616339509218, -208.3546154443345984 ) ) ;
#67068 = DIRECTION ( 'NONE',  ( 0.000000000000000000, 0.000000000000000000, 1.000000000000000000 ) ) ;
#67069 = CARTESIAN_POINT ( 'NONE',  ( -5.238584658564489516, -294.3914906410022923, -201.9600640479076787 ) ) ;
#67070 = CIRCLE ( 'NONE', #57970, 0.5000000000000004441 ) ;
#67071 = CARTESIAN_POINT ( 'NONE',  ( 37.00639414487677925, -273.4252965533545421, -260.4939235253460765 ) ) ;
#67072 = CARTESIAN_POINT ( 'NONE',  ( 12.30369635928613192, -287.5782853685344094, -329.0083125243459108 ) ) ;
#67073 = CARTESIAN_POINT ( 'NONE',  ( 15.46200124246062302, -291.2135156333661712, -218.7300750239710965 ) ) ;
#67074 = DIRECTION ( 'NONE',  ( -1.000000000000000000, -0.000000000000000000, -0.000000000000000000 ) ) ;
#67075 = CARTESIAN_POINT ( 'NONE',  ( -61.97076326710509875, -276.0638323838589372, -339.6586574966509602 ) ) ;
#67076 = CARTESIAN_POINT ( 'NONE',  ( -101.2415784662805152, -294.1800223847569100, -308.2469228993342085 ) ) ;
#67077 = CARTESIAN_POINT ( 'NONE',  ( -107.4172661429287814, -291.5736688567221222, -292.6801288580591631 ) ) ;
#67078 = DIRECTION ( 'NONE',  ( -5.501794166262391869E-14, -0.01273136352371387336, 0.9999189529070978688 ) ) ;
#67079 = DIRECTION ( 'NONE',  ( -0.3994899938748465162, 0.000000000000000000, -0.9167375550253601402 ) ) ;
#67080 = CARTESIAN_POINT ( 'NONE',  ( -6.152451996253581967, -290.9344534533494198, -200.7054560148281439 ) ) ;
#67081 = CARTESIAN_POINT ( 'NONE',  ( 0.5622441613669305616, -288.1661762795995969, -206.9791093043430976 ) ) ;
#67082 = CARTESIAN_POINT ( 'NONE',  ( -111.0066043073602202, -289.0289617690413593, -251.6686016540460287 ) ) ;
#67083 = ADVANCED_FACE ( 'NONE', ( #8799 ), #14997, .T. ) ;
#67084 = CARTESIAN_POINT ( 'NONE',  ( -6.788291178628715450, -287.8865278912126087, -203.4005563017663292 ) ) ;
#67085 = LINE ( 'NONE', #8828, #53182 ) ;
#67086 = CARTESIAN_POINT ( 'NONE',  ( 35.15473015238328003, -288.2205742338979917, -260.1492372354751410 ) ) ;
#67087 = CARTESIAN_POINT ( 'NONE',  ( -87.49159065223909693, -297.7272680495831878, -326.6751383333937611 ) ) ;
#67088 = DIRECTION ( 'NONE',  ( 0.000000000000000000, 1.000000000000000000, 0.000000000000000000 ) ) ;
#67089 = CARTESIAN_POINT ( 'NONE',  ( 34.70428713649813091, -289.0893596023928467, -296.5421444732897953 ) ) ;
#67090 = CARTESIAN_POINT ( 'NONE',  ( -56.12183050692097908, -277.8316678855341024, -197.3298115186908603 ) ) ;
#67091 = CARTESIAN_POINT ( 'NONE',  ( -99.63015502882376495, -278.2848947340166319, -315.6150755841263162 ) ) ;
#67092 = CARTESIAN_POINT ( 'NONE',  ( 24.57726242904086078, -280.6108963186658798, -224.6250669129683786 ) ) ;
#67093 = CARTESIAN_POINT ( 'NONE',  ( -101.3192648241746809, -299.0506401058523807, -231.8064421044385881 ) ) ;
#67094 = CARTESIAN_POINT ( 'NONE',  ( -11.30440954584355140, -284.3912514542718100, -200.0257773101257328 ) ) ;
#67095 = CARTESIAN_POINT ( 'NONE',  ( -48.18343439339132317, -264.4312075782299303, -496.1714326515946709 ) ) ;
#67096 = CARTESIAN_POINT ( 'NONE',  ( -69.02940375500685377, -277.7704813289437311, -203.2287493168912249 ) ) ;
#67097 = CARTESIAN_POINT ( 'NONE',  ( -96.48345021416767509, -281.9193463663916077, -316.4832823921498743 ) ) ;
#67098 = CARTESIAN_POINT ( 'NONE',  ( -18.20453976106250948, -63.49190233628851132, 21.50000000000000000 ) ) ;
#67099 = CARTESIAN_POINT ( 'NONE',  ( 33.53302209126650268, -274.3956334448254211, -298.7785890836640306 ) ) ;
#67100 = CARTESIAN_POINT ( 'NONE',  ( -58.58982259336092824, -296.8520811827672219, -340.9247420584073893 ) ) ;
#67101 = CARTESIAN_POINT ( 'NONE',  ( 0.7030212800304437293, -281.4775768392740360, -336.9652633126052592 ) ) ;
#67102 = CARTESIAN_POINT ( 'NONE',  ( -66.92534439354429310, -298.5959352864591096, -203.3532405654270860 ) ) ;
#67103 = CARTESIAN_POINT ( 'NONE',  ( -66.02301925929761239, -275.1093884928051807, -199.5234128694778235 ) ) ;
#67104 = CARTESIAN_POINT ( 'NONE',  ( -90.20898637332717840, -272.9452320430669943, -219.9728193391177342 ) ) ;
#67105 = CARTESIAN_POINT ( 'NONE',  ( 33.68713843373978989, -295.2389984390615041, -246.1184032491807443 ) ) ;
#67106 = CARTESIAN_POINT ( 'NONE',  ( 38.55650100448199424, -287.5555370908015789, -257.3042308033624295 ) ) ;
#67107 = CARTESIAN_POINT ( 'NONE',  ( -73.06288539889933986, -277.6624097925532624, -203.7633346351316845 ) ) ;
#67108 = CARTESIAN_POINT ( 'NONE',  ( -91.60003651476441178, -289.6322510181590815, -325.0715803121302088 ) ) ;
#67109 = CARTESIAN_POINT ( 'NONE',  ( -86.89738658733573118, -288.8205650247093672, -324.3524838485369060 ) ) ;
#67110 = CARTESIAN_POINT ( 'NONE',  ( -25.31635262876623216, -290.2052931954627866, -196.3314505255221434 ) ) ;
#67111 = ORIENTED_EDGE ( 'NONE', *, *, #73397, .T. ) ;
#67112 = CARTESIAN_POINT ( 'NONE',  ( 138.6539576904058606, 275.5000000000000568, -10.49999999999999822 ) ) ;
#67113 = AXIS2_PLACEMENT_3D ( 'NONE', #43404, #72299, #42944 ) ;
#67114 = CARTESIAN_POINT ( 'NONE',  ( -92.46227780242949734, -289.3759609834672801, -318.3920261567783427 ) ) ;
#67115 = DIRECTION ( 'NONE',  ( 0.000000000000000000, 0.000000000000000000, 1.000000000000000000 ) ) ;
#67116 = CARTESIAN_POINT ( 'NONE',  ( -43.65889435197683355, -286.9155621666130855, -193.8036862660932229 ) ) ;
#67117 = CARTESIAN_POINT ( 'NONE',  ( 17.36665895637874613, -289.4090924074130839, -226.6919474004047572 ) ) ;
#67118 = CARTESIAN_POINT ( 'NONE',  ( 37.22856853686766243, -292.8401845483138572, -288.6395646410342692 ) ) ;
#67119 = CARTESIAN_POINT ( 'NONE',  ( 27.89332935335748687, -283.3940585929251483, -310.4326541464980664 ) ) ;
#67120 = CARTESIAN_POINT ( 'NONE',  ( -62.56088033759416334, -285.5480941702116411, -201.8017877787754344 ) ) ;
#67121 = CARTESIAN_POINT ( 'NONE',  ( -96.93742279020844421, -273.3736483458357043, -221.5824675792455594 ) ) ;
#67122 = CARTESIAN_POINT ( 'NONE',  ( 29.61037270951217693, -277.2730852330810762, -300.6705788711578862 ) ) ;
#67123 = CARTESIAN_POINT ( 'NONE',  ( -2.854407636615578614, -290.5304793409114268, -204.1608652479899035 ) ) ;
#67124 = CARTESIAN_POINT ( 'NONE',  ( 28.22283236386519434, -273.9017473753379477, -237.3698678889065548 ) ) ;
#67125 = ORIENTED_EDGE ( 'NONE', *, *, #69736, .F. ) ;
#67126 = CARTESIAN_POINT ( 'NONE',  ( -90.78337343436103879, -230.3218577325732781, -348.1307343985224634 ) ) ;
#67127 = CARTESIAN_POINT ( 'NONE',  ( 23.14770022548389505, -288.8765671158278678, -226.8882310111470986 ) ) ;
#67128 = AXIS2_PLACEMENT_3D ( 'NONE', #69522, #90794, #25953 ) ;
#67129 = CARTESIAN_POINT ( 'NONE',  ( -111.2902972993403239, -297.3761934605768715, -290.6859177791066600 ) ) ;
#67130 = CIRCLE ( 'NONE', #65672, 9.550761578869391144 ) ;
#67131 = CARTESIAN_POINT ( 'NONE',  ( -79.37466418584727990, -286.1195492096652515, -210.4899178405654254 ) ) ;
#67132 = CARTESIAN_POINT ( 'NONE',  ( -112.1696816401933461, -277.8258537772218801, -253.2265506668895512 ) ) ;
#67133 = CARTESIAN_POINT ( 'NONE',  ( 37.32098186564452647, -293.9729947841724993, -251.9546869176466544 ) ) ;
#67134 = CARTESIAN_POINT ( 'NONE',  ( -5.274848766114055287, -284.6092408817195860, -201.7169446826105741 ) ) ;
#67135 = CARTESIAN_POINT ( 'NONE',  ( -32.00973624925237715, -295.3199247476409823, -347.1683429578675373 ) ) ;
#67136 = CARTESIAN_POINT ( 'NONE',  ( -62.81207961219386959, -292.0444990326904531, -201.9261323706388680 ) ) ;
#67137 = DIRECTION ( 'NONE',  ( -1.000000000000000000, -0.000000000000000000, -0.000000000000000000 ) ) ;
#67138 = AXIS2_PLACEMENT_3D ( 'NONE', #10330, #26423, #82767 ) ;
#67139 = CARTESIAN_POINT ( 'NONE',  ( -69.44094709309867142, -196.3684237510412345, -356.8806884016054823 ) ) ;
#67140 = CARTESIAN_POINT ( 'NONE',  ( -111.0565450862888923, -286.3236734884974908, -250.4435723626106096 ) ) ;
#67141 = CARTESIAN_POINT ( 'NONE',  ( -111.2586520408596868, -276.4809262143062369, -234.7283546768995564 ) ) ;
#67142 = ORIENTED_EDGE ( 'NONE', *, *, #24310, .T. ) ;
#67143 = CARTESIAN_POINT ( 'NONE',  ( -108.3962118054631389, -283.2353629247668891, -288.4022500083157183 ) ) ;
#67144 = CARTESIAN_POINT ( 'NONE',  ( -107.3981177076023101, -278.6282213137575354, -238.3291488797613056 ) ) ;
#67145 = CARTESIAN_POINT ( 'NONE',  ( 30.99887550291407479, -283.9542864923766956, -300.9776946793386401 ) ) ;
#67146 = CARTESIAN_POINT ( 'NONE',  ( 204.7386030247377562, 293.0225492072176507, -68.45606671877085603 ) ) ;
#67147 = CARTESIAN_POINT ( 'NONE',  ( -55.57926598438943699, -281.8571562876591088, -344.5635268580948605 ) ) ;
#67148 = CARTESIAN_POINT ( 'NONE',  ( -41.38742328547321847, -284.0210952733966678, -195.8132526376336955 ) ) ;
#67149 = CARTESIAN_POINT ( 'NONE',  ( -21.63436553773008697, -276.1118636618704727, -196.2423948563264560 ) ) ;
#67150 = TOROIDAL_SURFACE ( 'NONE', #89747, 5.654241149514405151, 0.5000000000000000000 ) ;
#67151 = CARTESIAN_POINT ( 'NONE',  ( -107.5202228255254511, -297.3130572852704745, -250.0396172073275807 ) ) ;
#67152 = CARTESIAN_POINT ( 'NONE',  ( 35.32300509861118343, -292.3854889307983171, -281.6954669123883832 ) ) ;
#67153 = CARTESIAN_POINT ( 'NONE',  ( -104.7082862754642889, -279.6844843211132456, -233.2793723770433871 ) ) ;
#67154 = CARTESIAN_POINT ( 'NONE',  ( -39.15776283274031044, -277.0755747228943733, -343.3385248716291471 ) ) ;
#67155 = CARTESIAN_POINT ( 'NONE',  ( -34.78126636156569873, -299.0247202028718334, -193.5960124504560156 ) ) ;
#67156 = CARTESIAN_POINT ( 'NONE',  ( -42.79795384507593070, -276.0398226069784187, -346.8576656513618559 ) ) ;
#67157 = CARTESIAN_POINT ( 'NONE',  ( -100.1937721120643232, -247.9095777054778296, -334.1646650126361351 ) ) ;
#67158 = CARTESIAN_POINT ( 'NONE',  ( 3.986236950277149305, -274.4957818316621001, -333.0085410706611810 ) ) ;
#67159 = EDGE_CURVE ( 'NONE', #84959, #63082, #11128, .T. ) ;
#67160 = CARTESIAN_POINT ( 'NONE',  ( 29.07159097861759633, -295.4731154986054094, -308.2553614361412428 ) ) ;
#67161 = CARTESIAN_POINT ( 'NONE',  ( 152.0128028882535887, 20.82798718771466540, 9.301361753755822193 ) ) ;
#67162 = CARTESIAN_POINT ( 'NONE',  ( -110.2140130185359368, -271.2396475792842807, -270.3444066551136871 ) ) ;
#67163 = CARTESIAN_POINT ( 'NONE',  ( -109.0194057203915179, -285.4290162551033063, -285.8003045221917660 ) ) ;
#67164 = CARTESIAN_POINT ( 'NONE',  ( -93.63319914156471668, -285.6094369579729459, -321.4219724254002131 ) ) ;
#67165 = CARTESIAN_POINT ( 'NONE',  ( -9.446826437434063806, -285.7751645927073696, -202.7771184128829134 ) ) ;
#67166 = CARTESIAN_POINT ( 'NONE',  ( -94.54787670534862798, -277.6048834966633763, -223.7360841601449977 ) ) ;
#67167 = CARTESIAN_POINT ( 'NONE',  ( -81.33948134609407532, -285.5175458894618714, -330.2168709138405234 ) ) ;
#67168 = CARTESIAN_POINT ( 'NONE',  ( -71.24356140075919086, -278.0760311576885329, -204.9147077670567967 ) ) ;
#67169 = CARTESIAN_POINT ( 'NONE',  ( -43.21821857092100316, -278.2077764581086399, -343.4343183007009088 ) ) ;
#67170 = CARTESIAN_POINT ( 'NONE',  ( 207.5984058588019536, 35.65225752631543088, 15.03172026579641951 ) ) ;
#67171 = CARTESIAN_POINT ( 'NONE',  ( -87.38001200859233109, -273.8240679204694175, -217.0550541341134760 ) ) ;
#67172 = CARTESIAN_POINT ( 'NONE',  ( 12.87889640766004362, -281.5354978606392820, -212.2057183741234496 ) ) ;
#67173 = CARTESIAN_POINT ( 'NONE',  ( -2.423677066864237339, -280.9939176628369637, -201.7879707990360032 ) ) ;
#67174 = ORIENTED_EDGE ( 'NONE', *, *, #47800, .T. ) ;
#67175 = ORIENTED_EDGE ( 'NONE', *, *, #32585, .F. ) ;
#67176 = CARTESIAN_POINT ( 'NONE',  ( 198.8856906601489811, 17.32477107587094167, -10.54429824094598800 ) ) ;
#67177 = CARTESIAN_POINT ( 'NONE',  ( 38.34233430548384547, -289.3554556185041520, -265.8676532450549530 ) ) ;
#67178 = CARTESIAN_POINT ( 'NONE',  ( -57.94047622556596622, -296.9763115912165290, -200.1593220665804438 ) ) ;
#67179 = CARTESIAN_POINT ( 'NONE',  ( -81.86460726792671494, -290.8115074242801370, -207.6632430096129269 ) ) ;
#67180 = EDGE_CURVE ( 'NONE', #75708, #92063, #86759, .T. ) ;
#67181 = CARTESIAN_POINT ( 'NONE',  ( 30.60851312404269109, -285.6513616178258417, -241.7073793894672349 ) ) ;
#67182 = CARTESIAN_POINT ( 'NONE',  ( -0.7137964244690365723, -287.1305112318431725, -334.2458695315031036 ) ) ;
#67183 = CARTESIAN_POINT ( 'NONE',  ( -19.73538753594966266, -287.4886996175510490, -199.1070075008561560 ) ) ;
#67184 = CARTESIAN_POINT ( 'NONE',  ( -87.88362010494839183, -275.7586119608566264, -325.7733456167005670 ) ) ;
#67185 = CARTESIAN_POINT ( 'NONE',  ( -62.51875825914677876, -287.7741057323520408, -342.3374072339535701 ) ) ;
#67186 = TOROIDAL_SURFACE ( 'NONE', #91343, 4.499999999999993783, 0.5000000000000000000 ) ;
#67187 = CARTESIAN_POINT ( 'NONE',  ( -66.43731475674965736, -287.6713123412391724, -201.2348143065191834 ) ) ;
#67188 = CARTESIAN_POINT ( 'NONE',  ( -26.43631521522038597, -286.9135113304699303, -344.7324901920360389 ) ) ;
#67189 = CARTESIAN_POINT ( 'NONE',  ( 27.06766247056771135, -282.9674346090739050, -305.2157081696362297 ) ) ;
#67190 = CARTESIAN_POINT ( 'NONE',  ( -112.3597751268069374, -292.6128376636565349, -265.6370469035957740 ) ) ;
#67191 = CARTESIAN_POINT ( 'NONE',  ( 85.55100297371609486, -296.0521521680024080, -521.1711561948568487 ) ) ;
#67192 = CARTESIAN_POINT ( 'NONE',  ( -26.41588298435790350, -486.4924983417995463, -430.6442049081568939 ) ) ;
#67193 = CARTESIAN_POINT ( 'NONE',  ( -37.62722966810062530, -299.9687512229966160, -194.8016534822850190 ) ) ;
#67194 = CARTESIAN_POINT ( 'NONE',  ( 18.96691926186968402, -280.0881349738864969, -223.6304183291449590 ) ) ;
#67195 = CARTESIAN_POINT ( 'NONE',  ( 31.13025227645281845, -279.9546092520665752, -301.0923321726776862 ) ) ;
#67196 = CARTESIAN_POINT ( 'NONE',  ( 21.23790151372838864, -293.4210296920037422, -320.0862534018947372 ) ) ;
#67197 = CARTESIAN_POINT ( 'NONE',  ( -69.58890371489638937, -296.0202478865766125, -203.9792056979342760 ) ) ;
#67198 = CARTESIAN_POINT ( 'NONE',  ( 26.60023806229068555, -274.1459053420546752, -308.4759803933796434 ) ) ;
#67199 = CARTESIAN_POINT ( 'NONE',  ( -7.774641969351842263, -295.9715550941667743, -337.6580151683760960 ) ) ;
#67200 = CARTESIAN_POINT ( 'NONE',  ( 208.4306832106271088, 0.04196010845015941959, 7.500000000000013323 ) ) ;
#67201 = CARTESIAN_POINT ( 'NONE',  ( -89.74545365340810577, -271.9052102155274042, -214.6790523281290177 ) ) ;
#67203 = CARTESIAN_POINT ( 'NONE',  ( -66.55584663536464518, -293.6693983638438112, -340.5214651889994002 ) ) ;
#67202 = CIRCLE ( 'NONE', #26364, 4.499999999999990230 ) ;
#67204 = CIRCLE ( 'NONE', #85376, 2.888540232138026020 ) ;
#67205 = EDGE_CURVE ( 'NONE', #30245, #47563, #80785, .T. ) ;
#67206 = CARTESIAN_POINT ( 'NONE',  ( -32.13355566123360063, -293.5443747821661873, -196.9436946687442287 ) ) ;
#67207 = DIRECTION ( 'NONE',  ( -1.000000000000000000, 8.612884727757786904E-16, 0.000000000000000000 ) ) ;
#67208 = CARTESIAN_POINT ( 'NONE',  ( 6.765473385440317067, -293.4727160591680786, -211.9902436436635185 ) ) ;
#67209 = LINE ( 'NONE', #1391, #21789 ) ;
#67211 = CARTESIAN_POINT ( 'NONE',  ( 24.42725678660558941, -294.0907046220681877, -309.3610324079171505 ) ) ;
#67210 = CARTESIAN_POINT ( 'NONE',  ( -111.9740461264605216, -282.4344743007750367, -281.1430340061093602 ) ) ;
#67212 = VECTOR ( 'NONE', #90421, 1000.000000000000000 ) ;
#67213 = CARTESIAN_POINT ( 'NONE',  ( -61.23167197043027699, -283.3538578861689530, -343.6170021527532867 ) ) ;
#67214 = CARTESIAN_POINT ( 'NONE',  ( 23.41894926102405705, -282.8639673083965249, -225.4449996485074053 ) ) ;
#67215 = CARTESIAN_POINT ( 'NONE',  ( -20.98432085465331554, -285.9232626858099593, -195.1402403305374946 ) ) ;
#67216 = CARTESIAN_POINT ( 'NONE',  ( -101.8980960154815563, -288.0438598959605656, -308.3116207361771330 ) ) ;
#67217 = CARTESIAN_POINT ( 'NONE',  ( -112.3417001280813707, -270.0523547857346784, -270.3292895737545223 ) ) ;
#67218 = CARTESIAN_POINT ( 'NONE',  ( 11.03793403273828133, -280.8766763805475648, -329.4389598514219983 ) ) ;
#67219 = TOROIDAL_SURFACE ( 'NONE', #32402, 1.000000000000000000, 0.5000000000000000000 ) ;
#67220 = CARTESIAN_POINT ( 'NONE',  ( -81.76343465556995227, -284.1173616825222439, -211.8123948694205012 ) ) ;
#67221 = CARTESIAN_POINT ( 'NONE',  ( -109.5790508519872759, -289.1443324696557511, -296.2724259491490102 ) ) ;
#67222 = DIRECTION ( 'NONE',  ( -1.000000000000000000, 0.000000000000000000, 0.000000000000000000 ) ) ;
#67223 = CARTESIAN_POINT ( 'NONE',  ( -87.01354922164073002, -297.3578301508761683, -324.9426883259619672 ) ) ;
#67224 = CARTESIAN_POINT ( 'NONE',  ( -111.9054128004683548, -279.7669623011300928, -287.0601912528625235 ) ) ;
#67226 = CARTESIAN_POINT ( 'NONE',  ( -105.5325100142869701, -278.5692543396213523, -244.1024537456504788 ) ) ;
#67225 = CARTESIAN_POINT ( 'NONE',  ( 30.73307997374178413, -291.9968334733025017, -302.7972363169708387 ) ) ;
#67227 = CARTESIAN_POINT ( 'NONE',  ( -36.27231987935523705, -295.2058083195963718, -347.3667955588527434 ) ) ;
#67228 = CARTESIAN_POINT ( 'NONE',  ( -112.3865618798553214, -282.7442553626093513, -261.5530011744070293 ) ) ;
#67229 = EDGE_CURVE ( 'NONE', #50020, #13665, #91277, .T. ) ;
#67230 = CARTESIAN_POINT ( 'NONE',  ( -73.11975142816839934, -279.5265209563599456, -336.2918238646853411 ) ) ;
#67231 = CARTESIAN_POINT ( 'NONE',  ( -72.24724726191968216, -294.5846537082790633, -334.7571956517979288 ) ) ;
#67232 = CARTESIAN_POINT ( 'NONE',  ( -36.19614810475733435, -296.0663354996369776, -195.3614998211027682 ) ) ;
#67233 = ORIENTED_EDGE ( 'NONE', *, *, #78401, .F. ) ;
#67234 = DIRECTION ( 'NONE',  ( -0.000000000000000000, -0.000000000000000000, -1.000000000000000000 ) ) ;
#67235 = CARTESIAN_POINT ( 'NONE',  ( 28.31347594401546530, -284.0059076043989421, -305.8751244430252996 ) ) ;
#67236 = CARTESIAN_POINT ( 'NONE',  ( -73.33817941723678757, -295.0511172822161257, -333.9397458422032514 ) ) ;
#67237 = DIRECTION ( 'NONE',  ( 0.000000000000000000, 1.000000000000000000, 0.000000000000000000 ) ) ;
#67238 = CARTESIAN_POINT ( 'NONE',  ( -95.95921662488163406, -276.6952119285918457, -223.5744983911110353 ) ) ;
#67239 = CARTESIAN_POINT ( 'NONE',  ( -0.1147036217591330398, -273.7315856037491812, -203.1277831806561949 ) ) ;
#67240 = CARTESIAN_POINT ( 'NONE',  ( 38.60317270302880388, -288.9892022401427312, -280.0440473583533390 ) ) ;
#67241 = CARTESIAN_POINT ( 'NONE',  ( -109.1792958072182671, -290.2143049699486710, -283.3364735291740431 ) ) ;
#67242 = CARTESIAN_POINT ( 'NONE',  ( -96.97807113952106306, -280.6724213909766945, -227.0689592676622794 ) ) ;
#67243 = CARTESIAN_POINT ( 'NONE',  ( -79.32675617718699357, -275.0753945812171537, -209.6055766035934198 ) ) ;
#67244 = CARTESIAN_POINT ( 'NONE',  ( -83.67658917716417477, -278.1951032996797721, -213.3725173046678378 ) ) ;
#67245 = ORIENTED_EDGE ( 'NONE', *, *, #86598, .F. ) ;
#67246 = CARTESIAN_POINT ( 'NONE',  ( -5.112330907720179063, -274.2981139810358400, -200.4306685046049950 ) ) ;
#67247 = CARTESIAN_POINT ( 'NONE',  ( -2.993122102728259737, -294.4298949750158272, -204.3195448023802498 ) ) ;
#67248 = FACE_OUTER_BOUND ( 'NONE', #76556, .T. ) ;
#67249 = CARTESIAN_POINT ( 'NONE',  ( 113.5000000000000568, -298.0521521680024080, -397.9547385950631337 ) ) ;
#67250 = CARTESIAN_POINT ( 'NONE',  ( -11.55107514696371851, -290.5239656839238478, -199.0658906205357255 ) ) ;
#67251 = CARTESIAN_POINT ( 'NONE',  ( -102.0820708704232374, -272.5215621517092472, -236.3890010556425807 ) ) ;
#67252 = CARTESIAN_POINT ( 'NONE',  ( 189.9243309297870610, 250.0000000000000568, 24.72542485937348644 ) ) ;
#67253 = CARTESIAN_POINT ( 'NONE',  ( -112.6724754502308912, -291.9187502847668156, -282.5259049713156969 ) ) ;
#67254 = CARTESIAN_POINT ( 'NONE',  ( -99.90806341382572953, -293.6948066931273047, -220.5068182859052968 ) ) ;
#67255 = CARTESIAN_POINT ( 'NONE',  ( -42.83346622741892418, -287.9828744991214080, -195.7166207263345541 ) ) ;
#67256 = CARTESIAN_POINT ( 'NONE',  ( 36.43735435630544117, -273.3899329068153747, -257.7676863724011014 ) ) ;
#67257 = CARTESIAN_POINT ( 'NONE',  ( 34.64078572484808660, -277.7179406150380032, -289.3304598472988687 ) ) ;
#67258 = CARTESIAN_POINT ( 'NONE',  ( 13.91200012302444478, -290.8578076680587401, -216.3761903949640555 ) ) ;
#67259 = CARTESIAN_POINT ( 'NONE',  ( -2.971988806569705321, -282.3617651154215764, -202.8260506594240553 ) ) ;
#67260 = ORIENTED_EDGE ( 'NONE', *, *, #11852, .T. ) ;
#67261 = CARTESIAN_POINT ( 'NONE',  ( 32.32593649537962222, -281.1958750550029436, -292.6689329687255281 ) ) ;
#67262 = CARTESIAN_POINT ( 'NONE',  ( -111.1393078996293156, -279.3692440797518088, -291.2274927854888347 ) ) ;
#67263 = CARTESIAN_POINT ( 'NONE',  ( 25.59529122134308565, -280.9272285817746706, -314.0527493271473531 ) ) ;
#67264 = CIRCLE ( 'NONE', #46083, 2.999999999999993783 ) ;
#67265 = CARTESIAN_POINT ( 'NONE',  ( -39.94293719427697908, -278.0253002991465223, -347.0947659806677166 ) ) ;
#67266 = DIRECTION ( 'NONE',  ( 0.000000000000000000, 0.000000000000000000, 1.000000000000000000 ) ) ;
#67267 = CARTESIAN_POINT ( 'NONE',  ( 31.24071122881919393, -277.5070611841730397, -303.9353912762309164 ) ) ;
#67268 = CARTESIAN_POINT ( 'NONE',  ( -109.1418805571601069, -287.0519495502701943, -270.3937649182068412 ) ) ;
#67269 = ORIENTED_EDGE ( 'NONE', *, *, #79023, .F. ) ;
#67270 = EDGE_LOOP ( 'NONE', ( #74410, #66372, #376, #33343 ) ) ;
#67271 = CARTESIAN_POINT ( 'NONE',  ( -112.0447869666070488, -298.6451428507188552, -263.1315240048948567 ) ) ;
#67272 = CARTESIAN_POINT ( 'NONE',  ( -105.3948903130178962, -291.2669158378200791, -297.7551264675065568 ) ) ;
#67273 = CARTESIAN_POINT ( 'NONE',  ( -10.68979705083230058, -274.7229177476033897, -340.0857396393666932 ) ) ;
#67274 = CARTESIAN_POINT ( 'NONE',  ( -94.67874910501100771, -291.6292510843045420, -320.2253018222972401 ) ) ;
#67275 = CARTESIAN_POINT ( 'NONE',  ( -79.58285403195604601, -290.8133633878157980, -210.6368811586985146 ) ) ;
#67276 = CARTESIAN_POINT ( 'NONE',  ( 37.66104898046413751, -286.8444951715351863, -253.1528583090604911 ) ) ;
#67277 = DIRECTION ( 'NONE',  ( -0.000000000000000000, -1.000000000000000000, -0.000000000000000000 ) ) ;
#67278 = CARTESIAN_POINT ( 'NONE',  ( -109.5065926550581707, -282.7496501993414313, -285.8701209447646647 ) ) ;
#67279 = CARTESIAN_POINT ( 'NONE',  ( -108.1227528478971323, -292.1188228251868964, -292.9119394171157182 ) ) ;
#67280 = CARTESIAN_POINT ( 'NONE',  ( -98.67347127916190175, -283.5938607794312247, -229.5062333300321029 ) ) ;
#67281 = CARTESIAN_POINT ( 'NONE',  ( 2.960517666304172124, -281.9204804679612266, -208.8429654764919690 ) ) ;
#67282 = CARTESIAN_POINT ( 'NONE',  ( 38.32289856104132042, -288.3299839405026432, -257.3343895402467751 ) ) ;
#67283 = CARTESIAN_POINT ( 'NONE',  ( -93.14125524420126112, -279.7143763054685905, -223.1783463849918689 ) ) ;
#67284 = CARTESIAN_POINT ( 'NONE',  ( -4.759029756074045103, -291.2667666911273159, -201.0330694611046169 ) ) ;
#67285 = AXIS2_PLACEMENT_3D ( 'NONE', #50022, #86457, #13142 ) ;
#67286 = CARTESIAN_POINT ( 'NONE',  ( -35.16308127904952840, -286.8816498190725497, -193.5403693128261295 ) ) ;
#67287 = CARTESIAN_POINT ( 'NONE',  ( -89.84883142852483218, -285.8272468408390523, -214.0522923289053097 ) ) ;
#67288 = CARTESIAN_POINT ( 'NONE',  ( -99.02989991117676993, -284.1783019344570107, -309.4886300914752155 ) ) ;
#67289 = ORIENTED_EDGE ( 'NONE', *, *, #9862, .T. ) ;
#67290 = CYLINDRICAL_SURFACE ( 'NONE', #39766, 24.00000000000001066 ) ;
#67291 = CARTESIAN_POINT ( 'NONE',  ( 35.88259758053153803, -295.1644425481560461, -250.8558501298463455 ) ) ;
#67292 = CARTESIAN_POINT ( 'NONE',  ( -13.94885471067347282, -293.4396545293069494, -343.2039148475573711 ) ) ;
#67293 = CARTESIAN_POINT ( 'NONE',  ( -72.96691608450511524, -276.5952928440348728, -334.3618929345729498 ) ) ;
#67294 = CARTESIAN_POINT ( 'NONE',  ( -108.7908082757884358, -296.2634908557384392, -241.7867818651185985 ) ) ;
#67295 = EDGE_CURVE ( 'NONE', #83213, #11101, #9642, .T. ) ;
#67296 = CARTESIAN_POINT ( 'NONE',  ( 35.52053631844697890, -292.1805740573273624, -281.7288762314842074 ) ) ;
#67297 = CARTESIAN_POINT ( 'NONE',  ( -111.3875495933986173, -294.8137731126849985, -268.6879279365750790 ) ) ;
#67298 = CARTESIAN_POINT ( 'NONE',  ( -9.591502407463080360, -293.6279427758239535, -202.3581166651847809 ) ) ;
#67299 = CARTESIAN_POINT ( 'NONE',  ( 33.94513861798802168, -294.4065384265440457, -253.2074537107375534 ) ) ;
#67300 = CARTESIAN_POINT ( 'NONE',  ( 207.7761861081325208, 35.69891260691532153, 14.41714557868260371 ) ) ;
#67301 = CARTESIAN_POINT ( 'NONE',  ( -36.32541098104073996, -293.0393184409966238, -345.5337104244158013 ) ) ;
#67302 = CARTESIAN_POINT ( 'NONE',  ( -96.11546781232344472, -299.1925850660058472, -223.7507064996990778 ) ) ;
#67303 = CARTESIAN_POINT ( 'NONE',  ( -5.679891024229594798, -289.5664534029010611, -336.3985186978775346 ) ) ;
#67304 = CARTESIAN_POINT ( 'NONE',  ( -56.48138831106356150, -279.2773817837849037, -343.2990007930033016 ) ) ;
#67305 = CARTESIAN_POINT ( 'NONE',  ( 0.8357529046719096577, -275.3499996425079530, -336.8328046694530826 ) ) ;
#67306 = CARTESIAN_POINT ( 'NONE',  ( -83.51225683111574938, -272.7865010018898033, -208.7998246219504779 ) ) ;
#67307 = CARTESIAN_POINT ( 'NONE',  ( 6.419271446187398311, -280.5322395701727487, -330.5798157605046299 ) ) ;
#67308 = CARTESIAN_POINT ( 'NONE',  ( -37.14965647360055812, -275.4496292092017029, -346.5738013586403099 ) ) ;
#67309 = CARTESIAN_POINT ( 'NONE',  ( -105.2112596496005636, -295.6125463628455350, -242.1659700456739017 ) ) ;
#67310 = CARTESIAN_POINT ( 'NONE',  ( -50.04721132641633830, -275.8903207208568915, -196.3932448144565512 ) ) ;
#67311 = CARTESIAN_POINT ( 'NONE',  ( -74.33211428911454277, -274.1980928052942090, -207.2501019291577791 ) ) ;
#67312 = DIRECTION ( 'NONE',  ( 0.000000000000000000, 1.000000000000000000, 8.326672684688666165E-15 ) ) ;
#67314 = CARTESIAN_POINT ( 'NONE',  ( -19.26957063406313964, -274.1244116509696482, -199.5810569675059014 ) ) ;
#67313 = CARTESIAN_POINT ( 'NONE',  ( -112.6096505921947539, -288.5259291955848084, -273.9863673556396861 ) ) ;
#67315 = CARTESIAN_POINT ( 'NONE',  ( 37.50441561134613266, -287.7789892848617228, -288.5015900819303738 ) ) ;
#67316 = CARTESIAN_POINT ( 'NONE',  ( -23.75605052931431516, -300.2013042008109096, -195.0013520409553109 ) ) ;
#67317 = CARTESIAN_POINT ( 'NONE',  ( -97.56084291798067909, -295.1596666401516131, -225.9133383879100734 ) ) ;
#67318 = CARTESIAN_POINT ( 'NONE',  ( -0.4619413555700691565, -281.7719555207291933, -337.7855361320704333 ) ) ;
#67319 = LINE ( 'NONE', #52157, #60769 ) ;
#67320 = CARTESIAN_POINT ( 'NONE',  ( 36.78398702179362800, -279.4043088283045790, -258.8592749498809553 ) ) ;
#67321 = DIRECTION ( 'NONE',  ( 0.000000000000000000, 1.000000000000000000, -0.000000000000000000 ) ) ;
#67322 = CARTESIAN_POINT ( 'NONE',  ( -94.59102870938559704, -289.9929276234884696, -224.4102804452266753 ) ) ;
#67323 = CARTESIAN_POINT ( 'NONE',  ( -37.56767838799788706, -281.1946303143575960, -344.6086179463206349 ) ) ;
#67324 = CARTESIAN_POINT ( 'NONE',  ( 200.4644824113734387, 214.9910457053126720, -2.942835885954282471 ) ) ;
#67325 = FACE_OUTER_BOUND ( 'NONE', #74064, .T. ) ;
#67326 = CARTESIAN_POINT ( 'NONE',  ( -112.2414146217796969, -288.6133317072296904, -265.5835082708381378 ) ) ;
#67327 = CARTESIAN_POINT ( 'NONE',  ( -24.49441223519213295, -275.7390851462669161, -197.7442091394081274 ) ) ;
#67328 = CARTESIAN_POINT ( 'NONE',  ( -61.09389884139567073, -284.5587395081295767, -343.2439904538098290 ) ) ;
#67330 = CARTESIAN_POINT ( 'NONE',  ( -107.3549595134004306, -284.8277144478067271, -249.5183499439539787 ) ) ;
#67329 = CARTESIAN_POINT ( 'NONE',  ( 10.88574893284359923, -272.7926532337679078, -212.1258744927253588 ) ) ;
#67331 = CARTESIAN_POINT ( 'NONE',  ( 34.16335719649052294, -277.2056586243123775, -287.8039562352511780 ) ) ;
#67332 = CARTESIAN_POINT ( 'NONE',  ( 29.30556371658614978, -276.7608262536016923, -300.5396525469514017 ) ) ;
#67333 = ADVANCED_FACE ( 'NONE', ( #65686 ), #62682, .T. ) ;
#67334 = CARTESIAN_POINT ( 'NONE',  ( -44.21001317057650226, -285.1390435861709420, -345.0979394246302832 ) ) ;
#67335 = ORIENTED_EDGE ( 'NONE', *, *, #87153, .T. ) ;
#67336 = CARTESIAN_POINT ( 'NONE',  ( 199.4392256788250677, 65.82574266882504332, 7.741079165001067963 ) ) ;
#67337 = CARTESIAN_POINT ( 'NONE',  ( -114.3379425117592945, -296.3949860655756652, -269.6004187791383515 ) ) ;
#67338 = CARTESIAN_POINT ( 'NONE',  ( 31.46843160601511968, -289.1508124478490913, -241.2961993220737611 ) ) ;
#67339 = DIRECTION ( 'NONE',  ( 0.000000000000000000, 0.000000000000000000, 1.000000000000000000 ) ) ;
#67340 = CARTESIAN_POINT ( 'NONE',  ( -99.86837403722181250, -294.6952119285919025, -220.4570493818173702 ) ) ;
#67341 = CARTESIAN_POINT ( 'NONE',  ( -72.35338004339116935, -278.5202171850656327, -202.1140212282637094 ) ) ;
#67342 = CARTESIAN_POINT ( 'NONE',  ( -99.36788428090561354, -289.5444752506206783, -226.0983469922730649 ) ) ;
#67343 = CARTESIAN_POINT ( 'NONE',  ( -102.8636058403824762, -286.5264540420590720, -236.6329750986399461 ) ) ;
#67344 = AXIS2_PLACEMENT_3D ( 'NONE', #8443, #37322, #66230 ) ;
#67345 = CARTESIAN_POINT ( 'NONE',  ( -72.63234576131131348, -281.3382144144436552, -205.3031104377008376 ) ) ;
#67346 = CARTESIAN_POINT ( 'NONE',  ( -73.35150324320090931, -287.0097691400226836, -202.9088870676524436 ) ) ;
#67347 = CARTESIAN_POINT ( 'NONE',  ( 27.29527643271218906, -284.0620442482561998, -308.5040672663332657 ) ) ;
#67348 = CARTESIAN_POINT ( 'NONE',  ( 37.59235998408419022, -275.9410578058916599, -288.1347638980677175 ) ) ;
#67349 = CARTESIAN_POINT ( 'NONE',  ( -47.47155398077692467, -295.9430146026742818, -196.3544935559752673 ) ) ;
#67350 = CARTESIAN_POINT ( 'NONE',  ( -111.3366591557671370, -278.6525445484331271, -249.0598024596567370 ) ) ;
#67351 = CARTESIAN_POINT ( 'NONE',  ( -71.14284257855211990, -299.5226429488563440, -204.0235030947206099 ) ) ;
#67352 = CARTESIAN_POINT ( 'NONE',  ( 164.8901442405950206, 2.982772324107380690, 9.000000000000000000 ) ) ;
#67353 = CYLINDRICAL_SURFACE ( 'NONE', #14820, 11.60392986742922439 ) ;
#67354 = CARTESIAN_POINT ( 'NONE',  ( -15.23521048091404140, -296.4656831749665571, -194.6032272679434243 ) ) ;
#67355 = DIRECTION ( 'NONE',  ( 0.000000000000000000, 0.000000000000000000, 1.000000000000000000 ) ) ;
#67356 = CARTESIAN_POINT ( 'NONE',  ( -80.86105611716482144, -277.1688461107187322, -329.0471818799301786 ) ) ;
#67357 = CARTESIAN_POINT ( 'NONE',  ( -5.294431581063172132, -275.6696478140756312, -200.7839572271229542 ) ) ;
#67358 = CARTESIAN_POINT ( 'NONE',  ( 32.17420931639730242, -281.0305581380645208, -303.0494582179358076 ) ) ;
#67359 = CARTESIAN_POINT ( 'NONE',  ( 27.93461205222396160, -289.7825920756228015, -305.3554566858161934 ) ) ;
#67360 = CARTESIAN_POINT ( 'NONE',  ( -66.64017007673201931, -296.9491317606980374, -340.8330313381994756 ) ) ;
#67361 = CARTESIAN_POINT ( 'NONE',  ( -83.93147881670488175, -296.8808695817414218, -331.2342463426401196 ) ) ;
#67362 = CARTESIAN_POINT ( 'NONE',  ( 36.28241170012432804, -295.3789794690508188, -256.8915399723416044 ) ) ;
#67363 = CARTESIAN_POINT ( 'NONE',  ( 37.53694440331400273, -279.5648804297883885, -271.3631033876093284 ) ) ;
#67364 = CARTESIAN_POINT ( 'NONE',  ( -30.14707827695709597, -282.0639053194449275, -196.2182614113812633 ) ) ;
#67365 = CARTESIAN_POINT ( 'NONE',  ( -101.1181405841077918, -295.1512220851134316, -231.8697869987369700 ) ) ;
#67366 = CARTESIAN_POINT ( 'NONE',  ( -105.0637131644742226, -285.6960084731403526, -305.4071083088259684 ) ) ;
#67367 = CARTESIAN_POINT ( 'NONE',  ( -63.94584268494079993, -288.3276366471973233, -338.7269245778006166 ) ) ;
#67368 = CARTESIAN_POINT ( 'NONE',  ( 123.3741230786721701, 148.3115526884368762, -263.0448026886833759 ) ) ;
#67369 = VERTEX_POINT ( 'NONE', #81239 ) ;
#67370 = CARTESIAN_POINT ( 'NONE',  ( 16.25958489967095488, -286.8843587642941770, -324.8911590190015772 ) ) ;
#67371 = CARTESIAN_POINT ( 'NONE',  ( 35.01768728057285074, -287.0846437347926212, -260.1831399919752812 ) ) ;
#67372 = ORIENTED_EDGE ( 'NONE', *, *, #86489, .T. ) ;
#67373 = CARTESIAN_POINT ( 'NONE',  ( -66.44615608580583910, -284.5041065694489930, -341.3289147227118292 ) ) ;
#67374 = CARTESIAN_POINT ( 'NONE',  ( 26.65301224073414232, -275.4039328342498152, -235.0880852607534166 ) ) ;
#67375 = CARTESIAN_POINT ( 'NONE',  ( -95.41779936946916507, -290.1517639958345853, -220.2545327573945144 ) ) ;
#67376 = CARTESIAN_POINT ( 'NONE',  ( 26.64168061165032597, -282.7657468029810275, -313.0160095621785104 ) ) ;
#67377 = CARTESIAN_POINT ( 'NONE',  ( -5.253321675605685748, -281.9869382675909151, -201.1293064831605193 ) ) ;
#67378 = CARTESIAN_POINT ( 'NONE',  ( 39.39029413338710128, -281.8083722989147191, -264.2011384277763568 ) ) ;
#67379 = CARTESIAN_POINT ( 'NONE',  ( 23.68253067946291779, -280.9956187450828793, -230.2069670555943333 ) ) ;
#67380 = CARTESIAN_POINT ( 'NONE',  ( 10.59707575819633618, -273.9094976428776249, -330.5268031993606428 ) ) ;
#67381 = CARTESIAN_POINT ( 'NONE',  ( 65.59659910285013495, 47.55397664594911333, -319.0097190562326546 ) ) ;
#67382 = VERTEX_POINT ( 'NONE', #8348 ) ;
#67383 = CARTESIAN_POINT ( 'NONE',  ( -13.16970484266629704, -278.7377274720011542, -341.2375088096205218 ) ) ;
#67384 = CARTESIAN_POINT ( 'NONE',  ( -114.2697886859462244, -273.0835924068001077, -270.3678844897593194 ) ) ;
#67385 = CARTESIAN_POINT ( 'NONE',  ( 36.99273977470537744, -279.4774700638589024, -263.0139704377475596 ) ) ;
#67386 = CARTESIAN_POINT ( 'NONE',  ( -71.70559143042845562, -296.9340132534039753, -205.8254655126555974 ) ) ;
#67387 = CARTESIAN_POINT ( 'NONE',  ( 38.54454576316462067, -293.2195243526579702, -283.1217813854034375 ) ) ;
#67388 = CARTESIAN_POINT ( 'NONE',  ( 202.9739431815424950, 291.9636489454802017, -68.24819713444452418 ) ) ;
#67389 = EDGE_CURVE ( 'NONE', #10282, #80534, #45236, .T. ) ;
#67391 = CARTESIAN_POINT ( 'NONE',  ( -58.94253714722416504, -287.7360410946706111, -340.9825175202570904 ) ) ;
#67390 = CARTESIAN_POINT ( 'NONE',  ( -59.95625032498254114, -296.3395747251707348, -197.3184347503279525 ) ) ;
#67392 = CARTESIAN_POINT ( 'NONE',  ( -103.8646930921256057, -297.9719881625472340, -303.4249985040450497 ) ) ;
#67393 = EDGE_CURVE ( 'NONE', #23662, #13726, #55122, .T. ) ;
#67394 = CARTESIAN_POINT ( 'NONE',  ( -6.826924175246609217, -287.7764474206499585, -203.4885541252969006 ) ) ;
#67395 = ORIENTED_EDGE ( 'NONE', *, *, #89572, .F. ) ;
#67396 = CARTESIAN_POINT ( 'NONE',  ( 38.99081327116950035, -294.3852573785742948, -261.7403986828321081 ) ) ;
#67397 = CARTESIAN_POINT ( 'NONE',  ( -67.80431599386086816, -283.9554626635209047, -336.7690804303391019 ) ) ;
#67398 = CARTESIAN_POINT ( 'NONE',  ( -31.92891780758167641, -296.9134330854134305, -193.7592673089102391 ) ) ;
#67399 = CARTESIAN_POINT ( 'NONE',  ( -3.401908195211420072, -293.2916676576797954, -201.4100516542314949 ) ) ;
#67400 = CARTESIAN_POINT ( 'NONE',  ( 15.39142019867240130, -293.2656090547933445, -214.2634698685775447 ) ) ;
#67401 = CARTESIAN_POINT ( 'NONE',  ( -45.36034040768231534, -289.3232569012757835, -342.9193801762237968 ) ) ;
#67402 = VERTEX_POINT ( 'NONE', #1251 ) ;
#67403 = CARTESIAN_POINT ( 'NONE',  ( 159.2635086430408080, 16.43186977800937498, 9.166206881811428175 ) ) ;
#67404 = CARTESIAN_POINT ( 'NONE',  ( -75.18384841405867292, -299.4142964258866755, -204.6634285069642374 ) ) ;
#67405 = CARTESIAN_POINT ( 'NONE',  ( -67.36580020186093520, -272.4619597697749782, -199.8872779138432918 ) ) ;
#67406 = CARTESIAN_POINT ( 'NONE',  ( -36.20185349507786299, -282.0962594986025920, -343.5875421647188546 ) ) ;
#67407 = ORIENTED_EDGE ( 'NONE', *, *, #27704, .F. ) ;
#67408 = CARTESIAN_POINT ( 'NONE',  ( -91.29036041939585289, -277.3019273465229162, -325.2907126768388366 ) ) ;
#67409 = CARTESIAN_POINT ( 'NONE',  ( -64.84824277484651134, -272.0866938712898104, -201.8651549287907585 ) ) ;
#67410 = CARTESIAN_POINT ( 'NONE',  ( -104.2339240973314105, -279.9828725069102120, -302.6715332450010010 ) ) ;
#67411 = CARTESIAN_POINT ( 'NONE',  ( -41.95664951067705317, -275.2504754441462751, -344.4655445766188677 ) ) ;
#67412 = CARTESIAN_POINT ( 'NONE',  ( -110.7718532313449344, -297.7785129490447957, -268.7393526505371142 ) ) ;
#67413 = CARTESIAN_POINT ( 'NONE',  ( -54.27754474621303160, -274.7704907015208846, -199.1109557761341193 ) ) ;
#67414 = CARTESIAN_POINT ( 'NONE',  ( -98.76140316746356973, -274.9149672771766859, -225.5346578042040733 ) ) ;
#67415 = CARTESIAN_POINT ( 'NONE',  ( -10.90061306522138906, -272.4151549353603059, -199.7416152477110245 ) ) ;
#67416 = CARTESIAN_POINT ( 'NONE',  ( 35.63586220609176536, -294.1369115335231754, -265.3010335679667833 ) ) ;
#67417 = CARTESIAN_POINT ( 'NONE',  ( 15.30967845870372379, -291.3883435325480491, -218.8759821830510930 ) ) ;
#67418 = CARTESIAN_POINT ( 'NONE',  ( -74.94434090351494149, -285.8906705383787994, 74.50000000000001421 ) ) ;
#67419 = CARTESIAN_POINT ( 'NONE',  ( 29.04601499248675367, -276.5510644160094103, -309.2481104629756601 ) ) ;
#67420 = CARTESIAN_POINT ( 'NONE',  ( -67.05944909184545111, -273.8181155025218345, -203.6701768189681729 ) ) ;
#67421 = CIRCLE ( 'NONE', #6927, 0.4999999999999923395 ) ;
#67422 = CARTESIAN_POINT ( 'NONE',  ( -65.67903593495820758, -284.3740415478202976, -199.2816373236528591 ) ) ;
#67423 = CARTESIAN_POINT ( 'NONE',  ( -1.556008960157877041, -296.5791324506783440, -336.4771845926472338 ) ) ;
#67424 = PLANE ( 'NONE',  #91118 ) ;
#67425 = CARTESIAN_POINT ( 'NONE',  ( -108.8204787368435120, -283.9554336488732815, -254.7018348278834026 ) ) ;
#67426 = CARTESIAN_POINT ( 'NONE',  ( -102.8325016633909712, -282.0604138649675292, -307.3581083774112130 ) ) ;
#67427 = CARTESIAN_POINT ( 'NONE',  ( 24.46952517151419926, -274.6764295799227966, -310.3893289985350066 ) ) ;
#67428 = CARTESIAN_POINT ( 'NONE',  ( 35.95267868534529754, -283.7572755667330853, -286.3243486608157582 ) ) ;
#67429 = ADVANCED_FACE ( 'NONE', ( #80314 ), #50974, .F. ) ;
#67430 = DIRECTION ( 'NONE',  ( -0.7453559924999194619, 0.000000000000000000, -0.6666666666666782870 ) ) ;
#67431 = CARTESIAN_POINT ( 'NONE',  ( 206.9189553108847406, 30.70889394204682432, 14.49999999999999822 ) ) ;
#67432 = CARTESIAN_POINT ( 'NONE',  ( 6.788450942039863989, -273.0409238516637060, -208.1757411893995311 ) ) ;
#67433 = CARTESIAN_POINT ( 'NONE',  ( -111.9433666116181598, -280.4291977326778351, -279.9709956902827344 ) ) ;
#67434 = CARTESIAN_POINT ( 'NONE',  ( 195.7161433444922807, 19.55326545191306309, 12.92152971952034513 ) ) ;
#67435 = CARTESIAN_POINT ( 'NONE',  ( -60.09994127140250697, -287.6797357710854044, -198.2553661509792278 ) ) ;
#67436 = CARTESIAN_POINT ( 'NONE',  ( 155.6265766802774806, 17.98195150565546996, -10.85854113850068892 ) ) ;
#67437 = CARTESIAN_POINT ( 'NONE',  ( -97.00855831940396001, -289.1740740990533709, -224.8996233648030909 ) ) ;
#67438 = DIRECTION ( 'NONE',  ( 0.000000000000000000, 0.000000000000000000, -1.000000000000000000 ) ) ;
#67439 = CARTESIAN_POINT ( 'NONE',  ( -95.09533644216796233, -294.7118432871770324, -315.6562391179234055 ) ) ;
#67440 = CARTESIAN_POINT ( 'NONE',  ( 12.97592401329083422, -286.4805591809691805, -325.0111833668403278 ) ) ;
#67441 = CARTESIAN_POINT ( 'NONE',  ( -107.5886556134111913, -275.3214365662247474, -283.9876634089608274 ) ) ;
#67442 = CARTESIAN_POINT ( 'NONE',  ( -35.04653889517396692, -296.0807262379776716, -195.3618917615749524 ) ) ;
#67443 = CARTESIAN_POINT ( 'NONE',  ( 9.784413016715705069, -286.8969497366213659, -330.4436332668842056 ) ) ;
#67444 = CARTESIAN_POINT ( 'NONE',  ( 19.11942211533632374, -283.8202233078185941, -317.9052839654305558 ) ) ;
#67445 = CARTESIAN_POINT ( 'NONE',  ( -73.80962969314016675, -281.7689925138185458, -337.0836488720716488 ) ) ;
#67446 = CARTESIAN_POINT ( 'NONE',  ( -37.54995011217922496, -292.0495095374964762, -197.3489713127045491 ) ) ;
#67447 = CARTESIAN_POINT ( 'NONE',  ( 32.79842370658523265, -283.2722255939596607, -292.7923843633008687 ) ) ;
#67448 = CARTESIAN_POINT ( 'NONE',  ( -3.537702344968634005, -283.3968537755233683, -335.2588312678752800 ) ) ;
#67449 = CARTESIAN_POINT ( 'NONE',  ( -92.37396928192313794, -291.8139898961089216, -321.9130442082536661 ) ) ;
#67450 = CARTESIAN_POINT ( 'NONE',  ( -68.17940801942711460, -297.8250554485802013, -199.7491228043520550 ) ) ;
#67451 = CARTESIAN_POINT ( 'NONE',  ( -45.88765554208796260, -287.2394101657951069, -345.4884198094632097 ) ) ;
#67452 = CARTESIAN_POINT ( 'NONE',  ( 21.85085722790037721, -274.8897807495739585, -221.1143804900233647 ) ) ;
#67453 = CARTESIAN_POINT ( 'NONE',  ( -37.57995285703409394, -294.0290811345717543, -195.7039702635589151 ) ) ;
#67454 = CARTESIAN_POINT ( 'NONE',  ( -23.68628624284178130, -44.55766379199612004, 22.50000000000000000 ) ) ;
#67455 = CARTESIAN_POINT ( 'NONE',  ( -110.4683760289727132, -287.2662352645559167, -253.7030783399848985 ) ) ;
#67456 = CARTESIAN_POINT ( 'NONE',  ( -41.31366113791848704, -275.1018660200039676, -345.4356665749590434 ) ) ;
#67457 = CARTESIAN_POINT ( 'NONE',  ( -111.4911300777384895, -295.1739438182590902, -252.8025742876987465 ) ) ;
#67458 = CARTESIAN_POINT ( 'NONE',  ( -110.5809626054065404, -292.0338012384750641, -279.4413628334679629 ) ) ;
#67459 = CARTESIAN_POINT ( 'NONE',  ( -48.88336149473123271, -273.2499681043040596, -198.1248148121722750 ) ) ;
#67460 = CARTESIAN_POINT ( 'NONE',  ( -99.41545353577029687, -291.5280305657475424, -310.0795883700643003 ) ) ;
#67461 = CARTESIAN_POINT ( 'NONE',  ( -83.98809387908922020, -292.3338723566047861, -213.9029706749503532 ) ) ;
#67462 = CARTESIAN_POINT ( 'NONE',  ( -85.50444300002443754, -285.4891905527342146, -326.5600878139779866 ) ) ;
#67463 = CARTESIAN_POINT ( 'NONE',  ( -74.40907086021208272, -292.9943638093243976, -203.5433335202371268 ) ) ;
#67464 = CARTESIAN_POINT ( 'NONE',  ( -56.08429023104190492, -293.1309501595307552, -196.1309592579417256 ) ) ;
#67465 = CARTESIAN_POINT ( 'NONE',  ( -38.34442247171282503, -294.8983877821257806, -343.3542310305479077 ) ) ;
#67466 = CARTESIAN_POINT ( 'NONE',  ( 37.44837555031843834, -289.6327263595887302, -276.6236570827797436 ) ) ;
#67467 = CARTESIAN_POINT ( 'NONE',  ( 37.33073559118222562, -281.4837439913778212, -251.5720959675283268 ) ) ;
#67468 = CARTESIAN_POINT ( 'NONE',  ( -26.44372333233875949, -296.2674149621003608, -194.8046424488529738 ) ) ;
#67469 = CARTESIAN_POINT ( 'NONE',  ( -64.54520477768802778, -285.5400060928985795, -198.3124494861497169 ) ) ;
#67470 = CARTESIAN_POINT ( 'NONE',  ( 33.61770922075736934, -277.2294890997626453, -247.0301939133530595 ) ) ;
#67471 = CARTESIAN_POINT ( 'NONE',  ( -109.8932374514378552, -283.1970374644556614, -281.7964063818723162 ) ) ;
#67472 = CARTESIAN_POINT ( 'NONE',  ( 32.17862485025679575, -285.9204056158101253, -298.6404964028990321 ) ) ;
#67473 = CARTESIAN_POINT ( 'NONE',  ( -68.52893239299793038, -275.5971571780453928, -339.4235526077253553 ) ) ;
#67474 = CARTESIAN_POINT ( 'NONE',  ( 199.7589824058529473, 41.15052235409930859, 10.49999999999999822 ) ) ;
#67475 = CARTESIAN_POINT ( 'NONE',  ( -16.12061027350512887, -282.2778709951963378, -340.2728751261355455 ) ) ;
#67476 = CARTESIAN_POINT ( 'NONE',  ( -6.404871329777954259, -281.6545982453667989, -200.2689547215233006 ) ) ;
#67477 = CARTESIAN_POINT ( 'NONE',  ( 37.59263406070686386, -286.8206939588185946, -287.0843930966144626 ) ) ;
#67478 = CARTESIAN_POINT ( 'NONE',  ( 18.75492264642632634, -295.9906309964503635, -318.6623604171315378 ) ) ;
#67479 = CARTESIAN_POINT ( 'NONE',  ( 5.439153599253639726, -278.0835830056513487, -333.4185439391347927 ) ) ;
#67480 = CARTESIAN_POINT ( 'NONE',  ( 25.67030322948781418, -277.4448831468405388, -313.8439183912683461 ) ) ;
#67481 = CARTESIAN_POINT ( 'NONE',  ( -59.19702043671041736, -277.1763795744126924, -340.0127150833978931 ) ) ;
#67482 = CARTESIAN_POINT ( 'NONE',  ( -99.99615301262304001, -299.1065787197618988, -229.3472803415267265 ) ) ;
#67483 = CARTESIAN_POINT ( 'NONE',  ( 37.48819883521037610, -285.5612182979672298, -271.0785052673513746 ) ) ;
#67484 = CARTESIAN_POINT ( 'NONE',  ( -98.37600032907307934, -291.5386813156269454, -316.0034578001072987 ) ) ;
#67485 = CARTESIAN_POINT ( 'NONE',  ( 31.82715020783358284, -292.7960656610079013, -294.8008114295665223 ) ) ;
#67486 = ORIENTED_EDGE ( 'NONE', *, *, #64191, .T. ) ;
#67487 = CARTESIAN_POINT ( 'NONE',  ( 19.36489469635971616, -292.5679730829990035, -224.3364538802302093 ) ) ;
#67488 = ORIENTED_EDGE ( 'NONE', *, *, #66150, .F. ) ;
#67489 = CARTESIAN_POINT ( 'NONE',  ( -26.17592747168105660, -289.9928471740839768, -346.2348158631659203 ) ) ;
#67490 = CARTESIAN_POINT ( 'NONE',  ( -32.96518863955563461, -280.7601599396897996, -197.3903100144099483 ) ) ;
#67491 = CARTESIAN_POINT ( 'NONE',  ( -111.3202141966663135, -295.7289312489323834, -249.9493835531594925 ) ) ;
#67492 = CARTESIAN_POINT ( 'NONE',  ( 20.20494462640257893, -287.5109782763636304, -219.2756966161275614 ) ) ;
#67493 = CARTESIAN_POINT ( 'NONE',  ( -1.806709704085969870, -288.9276371305409725, -338.6473446111414773 ) ) ;
#67494 = CARTESIAN_POINT ( 'NONE',  ( -65.31987339772369694, -283.7614687864306688, -337.8232879530835930 ) ) ;
#67495 = CARTESIAN_POINT ( 'NONE',  ( -100.1937721120545604, -247.9095777054600660, -334.1646650126529039 ) ) ;
#67496 = CARTESIAN_POINT ( 'NONE',  ( -110.6743395205602383, -264.9754415880684064, -306.3209493635451963 ) ) ;
#67497 = CARTESIAN_POINT ( 'NONE',  ( 172.9423030596852300, 240.7948373491403800, -177.0476525864039274 ) ) ;
#67498 = CARTESIAN_POINT ( 'NONE',  ( -72.92947600809826270, -276.7336899014498499, -334.2982353352063001 ) ) ;
#67499 = CARTESIAN_POINT ( 'NONE',  ( -110.6598727148159185, -277.5050117346015668, -267.8841605835873452 ) ) ;
#67500 = CARTESIAN_POINT ( 'NONE',  ( 76.28016853513979356, -298.9466307878727207, -193.4317762818265010 ) ) ;
#67501 = CARTESIAN_POINT ( 'NONE',  ( -46.15978596236939779, -155.9775659802373582, -362.2499631079683695 ) ) ;
#67502 = EDGE_CURVE ( 'NONE', #82047, #12908, #59552, .T. ) ;
#67503 = CARTESIAN_POINT ( 'NONE',  ( -28.67365081324876286, -275.6293807896831254, -346.4285795038637730 ) ) ;
#67504 = VERTEX_POINT ( 'NONE', #38618 ) ;
#67505 = CARTESIAN_POINT ( 'NONE',  ( -110.3075092998461884, -291.1054381300302225, -265.7379671348173247 ) ) ;
#67506 = CARTESIAN_POINT ( 'NONE',  ( -57.35753066787983556, -298.6031769264931768, -196.1202044263708615 ) ) ;
#67507 = CARTESIAN_POINT ( 'NONE',  ( 35.61173680904107641, -286.3534648892423888, -279.2515351168862594 ) ) ;
#67508 = CARTESIAN_POINT ( 'NONE',  ( -33.34475477686601153, -298.5932824275707844, -193.4223321786282668 ) ) ;
#67509 = CARTESIAN_POINT ( 'NONE',  ( -45.08862425399878049, -295.3195275842401202, -342.9993702803830047 ) ) ;
#67510 = VERTEX_POINT ( 'NONE', #67522 ) ;
#67511 = CARTESIAN_POINT ( 'NONE',  ( 197.6806146935310551, 68.83995197827617574, -9.477423483297931384 ) ) ;
#67512 = CARTESIAN_POINT ( 'NONE',  ( -41.28438838813088552, -279.0215473313475627, -345.8311498738309524 ) ) ;
#67513 = CARTESIAN_POINT ( 'NONE',  ( 17.77780919329176612, -281.7970574513081488, -324.1155995742814184 ) ) ;
#67514 = CARTESIAN_POINT ( 'NONE',  ( -85.29710753569284520, -278.8125153487922034, -325.8765691274239202 ) ) ;
#67515 = CARTESIAN_POINT ( 'NONE',  ( -111.4906035245811893, -280.1017770074629425, -286.9717815096015556 ) ) ;
#67516 = CARTESIAN_POINT ( 'NONE',  ( -101.3100796172653730, -271.5298930917532516, -233.6695579173734529 ) ) ;
#67517 = CARTESIAN_POINT ( 'NONE',  ( 156.4851178187871312, 0.000000000000000000, 7.000000000000000000 ) ) ;
#67518 = CARTESIAN_POINT ( 'NONE',  ( -85.48577373792517164, -279.5307654605460357, -215.4871881001894849 ) ) ;
#67519 = CARTESIAN_POINT ( 'NONE',  ( -102.5873322092470801, -273.8870371167427038, -229.7758212044883805 ) ) ;
#67520 = CARTESIAN_POINT ( 'NONE',  ( -57.60636522454186803, -275.7908285814836518, -198.0967127139663546 ) ) ;
#67521 = CARTESIAN_POINT ( 'NONE',  ( 7.877640444709827605, -275.0229685168492892, -332.0205893269721855 ) ) ;
#67522 = CARTESIAN_POINT ( 'NONE',  ( 222.4306832106270804, -141.7221692137691775, 22.50000000000000000 ) ) ;
#67523 = CARTESIAN_POINT ( 'NONE',  ( -33.48973234059639026, -291.2990075363006213, -197.2885950236634756 ) ) ;
#67524 = CARTESIAN_POINT ( 'NONE',  ( -111.6205801539287137, -284.1524892136673088, -250.2623046006208654 ) ) ;
#67525 = CARTESIAN_POINT ( 'NONE',  ( 30.96519848262594721, -279.4149736307926446, -241.8630195639390763 ) ) ;
#67527 = CARTESIAN_POINT ( 'NONE',  ( -94.34228945494660934, -283.2987962867776446, -222.4837014149917991 ) ) ;
#67526 = CARTESIAN_POINT ( 'NONE',  ( 7.515752311812053499, -279.2521724994480792, -211.9598184488929462 ) ) ;
#67528 = CARTESIAN_POINT ( 'NONE',  ( 28.10842582021338387, -290.0411469132703814, -307.0891890288916102 ) ) ;
#67529 = CARTESIAN_POINT ( 'NONE',  ( 20.82122626363265994, -282.1303246469889814, -225.5723545549112714 ) ) ;
#67530 = CARTESIAN_POINT ( 'NONE',  ( -80.08899952443231030, -271.4738533049682587, -208.6729679165025004 ) ) ;
#67531 = CARTESIAN_POINT ( 'NONE',  ( 24.44652508566888471, -280.5498077183483474, -314.9776049113219187 ) ) ;
#67532 = CARTESIAN_POINT ( 'NONE',  ( -19.73151157189154858, -296.8260355642370882, -343.3178187200014690 ) ) ;
#67533 = CARTESIAN_POINT ( 'NONE',  ( -103.8951190663378981, -277.2733181421044151, -233.6921060075632397 ) ) ;
#67534 = CARTESIAN_POINT ( 'NONE',  ( -71.69475909250618884, -278.1701329456275857, -334.9024402638229390 ) ) ;
#67535 = CARTESIAN_POINT ( 'NONE',  ( -43.54108341269972726, -287.9742998348873471, -195.3985391084868297 ) ) ;
#67536 = DIRECTION ( 'NONE',  ( 0.000000000000000000, 1.000000000000000000, 0.000000000000000000 ) ) ;
#67537 = CARTESIAN_POINT ( 'NONE',  ( -47.57307327863838253, -293.8433565187115732, -195.4442292658428357 ) ) ;
#67538 = CARTESIAN_POINT ( 'NONE',  ( 17.98991791078880453, -274.2591556012564524, -321.0104213023034845 ) ) ;
#67539 = CARTESIAN_POINT ( 'NONE',  ( -74.35851822292511315, -288.7286195731140879, -337.7104857608807151 ) ) ;
#67540 = CARTESIAN_POINT ( 'NONE',  ( 7.174846915916289092, -291.0701418209096687, -211.4992674139771509 ) ) ;
#67541 = CARTESIAN_POINT ( 'NONE',  ( -48.18343439339133027, -270.6804750412892986, -438.3045224571701510 ) ) ;
#67542 = CARTESIAN_POINT ( 'NONE',  ( -3.656252300233240327, -275.2826617979363277, -335.6798295734435555 ) ) ;
#67543 = CARTESIAN_POINT ( 'NONE',  ( -94.91529874919451970, -294.0392675413422126, -317.2441618246101598 ) ) ;
#67544 = CARTESIAN_POINT ( 'NONE',  ( -99.24821154366281917, -291.3231156582584163, -309.9695428704239930 ) ) ;
#67545 = FILL_AREA_STYLE_COLOUR ( '', #30605 ) ;
#67546 = CARTESIAN_POINT ( 'NONE',  ( 164.2231345125756263, 275.0000000000000568, -7.500000000000000000 ) ) ;
#67547 = CARTESIAN_POINT ( 'NONE',  ( 23.43485513168371170, -291.4113841519857715, -224.1994090858819675 ) ) ;
#67548 = CARTESIAN_POINT ( 'NONE',  ( 31.23605002149735910, -289.5147929915862051, -297.7668382666107050 ) ) ;
#67549 = CARTESIAN_POINT ( 'NONE',  ( -48.73943081701123958, -287.4351093290842414, -345.5413519771897768 ) ) ;
#67550 = CARTESIAN_POINT ( 'NONE',  ( 33.59243902203245824, -288.7206532899338640, -250.7722736776322279 ) ) ;
#67551 = CARTESIAN_POINT ( 'NONE',  ( 164.2231345125756263, 300.2961574867697436, -4.888549259831427740 ) ) ;
#67552 = CARTESIAN_POINT ( 'NONE',  ( 8.088190097750608487, -289.2152523562324404, -327.7085398991985699 ) ) ;
#67553 = CARTESIAN_POINT ( 'NONE',  ( -32.10117638658132222, -296.9662699677179489, -345.5468485300314683 ) ) ;
#67554 = DIRECTION ( 'NONE',  ( 0.2916739763039189470, 0.000000000000000000, 0.9565177946839572565 ) ) ;
#67555 = CARTESIAN_POINT ( 'NONE',  ( 39.20833832427597798, -288.8078325527840775, -274.3866879531319682 ) ) ;
#67556 = CARTESIAN_POINT ( 'NONE',  ( -110.0614300989277865, -276.3699032099878536, -290.8831810498074901 ) ) ;
#67557 = CARTESIAN_POINT ( 'NONE',  ( -98.78398228410944171, -278.2674287703714526, -316.7572075507293903 ) ) ;
#67558 = CARTESIAN_POINT ( 'NONE',  ( -39.58239002344271995, -279.6914903587204435, -193.4018324507144087 ) ) ;
#67559 = CARTESIAN_POINT ( 'NONE',  ( 54.16810326369736828, -301.1830605561279413, -195.6852559060315855 ) ) ;
#67560 = CARTESIAN_POINT ( 'NONE',  ( -57.91931973830251934, -283.7863288936917456, -198.1852125603847412 ) ) ;
#67561 = CARTESIAN_POINT ( 'NONE',  ( 193.9153122143737562, 214.9910457053126720, 17.21343741151142481 ) ) ;
#67562 = CARTESIAN_POINT ( 'NONE',  ( -6.230496755101428086, -278.6048701084087043, -202.9457673104903392 ) ) ;
#67563 = CARTESIAN_POINT ( 'NONE',  ( -22.15647361619059907, -280.8574611639105001, -343.8077621636666663 ) ) ;
#67564 = DIRECTION ( 'NONE',  ( 0.000000000000000000, 1.000000000000000000, 0.000000000000000000 ) ) ;
#67565 = CARTESIAN_POINT ( 'NONE',  ( -45.59405117923598993, -275.6346754299837585, -346.2728215737361097 ) ) ;
#67566 = CARTESIAN_POINT ( 'NONE',  ( -109.5603440661601979, -297.8797707072158687, -285.0927333549785203 ) ) ;
#67567 = CARTESIAN_POINT ( 'NONE',  ( 33.27590120156828135, -280.8562369823500831, -300.4073268444819860 ) ) ;
#67568 = CARTESIAN_POINT ( 'NONE',  ( -108.4061707829266368, -297.7268255583422842, -252.6108878092626071 ) ) ;
#67569 = CARTESIAN_POINT ( 'NONE',  ( -54.50094873605787171, -299.1512974505319562, -195.8033654773533954 ) ) ;
#67570 = CARTESIAN_POINT ( 'NONE',  ( -43.47967123505004139, -273.6393426889883358, -197.5476769053416035 ) ) ;
#67571 = CARTESIAN_POINT ( 'NONE',  ( 37.61950827621697613, -295.5213466823255999, -267.9490897163788645 ) ) ;
#67572 = CARTESIAN_POINT ( 'NONE',  ( 5.177907832212098604, -286.7763733076425297, -206.1019507667887751 ) ) ;
#67573 = EDGE_CURVE ( 'NONE', #17873, #5311, #45927, .T. ) ;
#67574 = CARTESIAN_POINT ( 'NONE',  ( -9.371004730146431427, -278.4947637660196733, -200.1688506196131243 ) ) ;
#67575 = CARTESIAN_POINT ( 'NONE',  ( -85.16633719142839709, -289.5248581508267307, -330.7765100054237450 ) ) ;
#67576 = CARTESIAN_POINT ( 'NONE',  ( -58.76938580649515131, -288.3948114037650043, -340.4445367884876532 ) ) ;
#67577 = CARTESIAN_POINT ( 'NONE',  ( 19.80355957313269855, -290.8794933502741742, -221.7676286452262673 ) ) ;
#67578 = ORIENTED_EDGE ( 'NONE', *, *, #29388, .T. ) ;
#67579 = CARTESIAN_POINT ( 'NONE',  ( -111.8439089875458023, -277.9397250554267202, -284.5643135594219189 ) ) ;
#67580 = CARTESIAN_POINT ( 'NONE',  ( 22.79699308962910465, -287.6374045630566911, -311.8720338318446466 ) ) ;
#67581 = CARTESIAN_POINT ( 'NONE',  ( 201.2104617360081704, 41.21457449016151031, 10.00000000000000000 ) ) ;
#67582 = CARTESIAN_POINT ( 'NONE',  ( -113.6686307448715354, -285.3907036865959981, -278.5476847368751123 ) ) ;
#67583 = CARTESIAN_POINT ( 'NONE',  ( -16.67839454482242800, -291.3715271518904046, -196.4297442991912703 ) ) ;
#67584 = CARTESIAN_POINT ( 'NONE',  ( -10.85693151091996000, -284.0292260764431944, -342.1938323639706141 ) ) ;
#67585 = CARTESIAN_POINT ( 'NONE',  ( -94.28634578134034427, -283.7397928423224585, -316.0571172866168581 ) ) ;
#67586 = CARTESIAN_POINT ( 'NONE',  ( -113.6017603480666622, -296.6865266288299381, -259.6166450812182234 ) ) ;
#67587 = CARTESIAN_POINT ( 'NONE',  ( 5.450382169254740283, -275.9599185819160425, -210.5480728740110123 ) ) ;
#67588 = CARTESIAN_POINT ( 'NONE',  ( -64.65039993833117649, -289.7139660385084881, -200.8772762663025730 ) ) ;
#67589 = CARTESIAN_POINT ( 'NONE',  ( 5.420477099717874836, -273.4400744687562224, -210.6449038828786513 ) ) ;
#67590 = VERTEX_POINT ( 'NONE', #33383 ) ;
#67591 = DIRECTION ( 'NONE',  ( -1.000000000000000000, 0.000000000000000000, 0.000000000000000000 ) ) ;
#67592 = CARTESIAN_POINT ( 'NONE',  ( 19.75075446432490978, -288.8071609049449648, -222.5734352522242716 ) ) ;
#67593 = AXIS2_PLACEMENT_3D ( 'NONE', #26482, #32182, #68641 ) ;
#67594 = CARTESIAN_POINT ( 'NONE',  ( -30.60435705395638095, -296.0485136181760026, -346.7554942018302313 ) ) ;
#67595 = CARTESIAN_POINT ( 'NONE',  ( -91.60244749309605083, -285.9048202018308302, -221.3003633134682104 ) ) ;
#67596 = ADVANCED_FACE ( 'NONE', ( #32466 ), #58069, .F. ) ;
#67597 = CARTESIAN_POINT ( 'NONE',  ( 22.45016307081918328, -275.2583318846948828, -318.5249561735231509 ) ) ;
#67598 = CARTESIAN_POINT ( 'NONE',  ( 36.98192300237801788, -293.9556352588261348, -250.5793500093642763 ) ) ;
#67599 = CARTESIAN_POINT ( 'NONE',  ( 35.94352342945006740, -285.9363108606283390, -289.5856203459081257 ) ) ;
#67600 = CARTESIAN_POINT ( 'NONE',  ( 29.55839593848838476, -294.3813002014196059, -308.5492689074562236 ) ) ;
#67601 = CARTESIAN_POINT ( 'NONE',  ( -107.7734021145991079, -291.1399995802161698, -251.0877466605860207 ) ) ;
#67602 = DIRECTION ( 'NONE',  ( 0.000000000000000000, 0.000000000000000000, 1.000000000000000000 ) ) ;
#67603 = LINE ( 'NONE', #2731, #2451 ) ;
#67604 = CARTESIAN_POINT ( 'NONE',  ( -55.03721977837319201, -169.7685131377856180, -360.6694990503212352 ) ) ;
#67605 = CARTESIAN_POINT ( 'NONE',  ( -104.8280314947001841, -286.5375332614957529, -234.6346883513537875 ) ) ;
#67606 = CARTESIAN_POINT ( 'NONE',  ( 36.57525178469694538, -273.4809262143061233, -305.9938812882205070 ) ) ;
#67607 = ORIENTED_EDGE ( 'NONE', *, *, #51429, .T. ) ;
#67608 = CARTESIAN_POINT ( 'NONE',  ( -93.66836427075458005, -282.8095319023058209, -317.2816143682121606 ) ) ;
#67609 = CARTESIAN_POINT ( 'NONE',  ( -93.32153504367020957, -277.4965134882685334, -323.2770141679658877 ) ) ;
#67610 = CARTESIAN_POINT ( 'NONE',  ( 36.36862586835917455, -283.3861069338970538, -257.4453806916467329 ) ) ;
#67611 = CARTESIAN_POINT ( 'NONE',  ( -92.99569426845059184, -240.8231148737314413, -340.8140838316123222 ) ) ;
#67612 = CARTESIAN_POINT ( 'NONE',  ( 1.776775480513330452, -281.1143465880900862, -335.9991493262335780 ) ) ;
#67613 = CARTESIAN_POINT ( 'NONE',  ( 17.19299240869666079, -284.8550474041055622, -219.3734922805081169 ) ) ;
#67614 = CARTESIAN_POINT ( 'NONE',  ( -43.95887525711700761, -275.8298985963662631, -194.8333803553555015 ) ) ;
#67615 = CARTESIAN_POINT ( 'NONE',  ( -9.201388971772328063, -295.1664038117265818, -337.7995927981606314 ) ) ;
#67616 = CARTESIAN_POINT ( 'NONE',  ( 35.78780539544837325, -292.1348332891051882, -262.5661422521280315 ) ) ;
#67617 = CARTESIAN_POINT ( 'NONE',  ( -107.3297964742374688, -279.6127572436719220, -238.3741459667424465 ) ) ;
#67618 = CARTESIAN_POINT ( 'NONE',  ( 9.664048229737067786, -276.3838701438514818, -326.2132407830538909 ) ) ;
#67619 = CARTESIAN_POINT ( 'NONE',  ( 37.91806818040716109, -274.2873166390560868, -255.6146002645775468 ) ) ;
#67620 = DIRECTION ( 'NONE',  ( -0.000000000000000000, -0.000000000000000000, 1.000000000000000000 ) ) ;
#67621 = CARTESIAN_POINT ( 'NONE',  ( 36.24934055300464308, -273.7386169413551897, -284.8957898882777613 ) ) ;
#67622 = EDGE_CURVE ( 'NONE', #85761, #4348, #26287, .T. ) ;
#67623 = CARTESIAN_POINT ( 'NONE',  ( -24.98507369733978223, -296.3229290802827336, -345.8198119692100363 ) ) ;
#67624 = CARTESIAN_POINT ( 'NONE',  ( 200.9306832106271088, -142.7221692137691775, 0.000000000000000000 ) ) ;
#67625 = CARTESIAN_POINT ( 'NONE',  ( -70.34180879251273666, -284.5773425291053513, -335.8367380935204665 ) ) ;
#67626 = CARTESIAN_POINT ( 'NONE',  ( -30.28636985388002500, -284.7241938046115024, -346.0195367341307247 ) ) ;
#67627 = CARTESIAN_POINT ( 'NONE',  ( -30.51351288922421645, -285.4892176662571615, -197.5279116498812186 ) ) ;
#67628 = CARTESIAN_POINT ( 'NONE',  ( 31.01136717562667044, -274.3223346835467851, -298.3232246276980391 ) ) ;
#67629 = CARTESIAN_POINT ( 'NONE',  ( -67.03219711769824585, -285.3059087430916065, -338.4141686933419351 ) ) ;
#67630 = CARTESIAN_POINT ( 'NONE',  ( -21.52288415571240421, -275.3256493941568124, -342.3891024212062462 ) ) ;
#67631 = CARTESIAN_POINT ( 'NONE',  ( -80.99246365659742253, -278.7406116943267875, -329.2579508013222949 ) ) ;
#67632 = FACE_OUTER_BOUND ( 'NONE', #70547, .T. ) ;
#67633 = SHAPE_REPRESENTATION ( 'Square Mounting Plate', ( #18940 ), #56754 ) ;
#67634 = CARTESIAN_POINT ( 'NONE',  ( 39.02110001429821295, -282.2421584506290628, -261.3587114209443030 ) ) ;
#67635 = CARTESIAN_POINT ( 'NONE',  ( -48.11637030904267931, -280.4110576700969091, -194.1270470132709249 ) ) ;
#67636 = ORIENTED_EDGE ( 'NONE', *, *, #18958, .T. ) ;
#67637 = ORIENTED_EDGE ( 'NONE', *, *, #31148, .T. ) ;
#67638 = CARTESIAN_POINT ( 'NONE',  ( 195.5762488419090346, 41.38929653454901114, 14.52727654096534060 ) ) ;
#67639 = CARTESIAN_POINT ( 'NONE',  ( -4.053772750359502020, -288.3468017202550300, -202.2864160177626047 ) ) ;
#67640 = CARTESIAN_POINT ( 'NONE',  ( -103.8611543254021967, -296.1606551595554038, -239.7799996812944130 ) ) ;
#67641 = CARTESIAN_POINT ( 'NONE',  ( -68.28013332678875713, -291.0049469301220597, -199.9470114095400390 ) ) ;
#67642 = CARTESIAN_POINT ( 'NONE',  ( 30.34278669191611399, -286.1910138262050509, -300.4345436580528599 ) ) ;
#67644 = CARTESIAN_POINT ( 'NONE',  ( -64.42178551901656647, -289.9336815404418530, -201.4660300265077808 ) ) ;
#67643 = CARTESIAN_POINT ( 'NONE',  ( 22.42976847945794105, -286.7221924786719569, -313.2883407966180584 ) ) ;
#67645 = CARTESIAN_POINT ( 'NONE',  ( -89.95815940492823870, -286.4938518603173634, -219.1155312442799357 ) ) ;
#67646 = CARTESIAN_POINT ( 'NONE',  ( -79.13344159225331964, -275.6153139123474034, -332.7008608179157250 ) ) ;
#67647 = CARTESIAN_POINT ( 'NONE',  ( 38.29388296519224610, -286.0743698888280733, -280.0419751694623756 ) ) ;
#67648 = CARTESIAN_POINT ( 'NONE',  ( 18.77296796986961880, -288.8595077083489855, -220.5236111560628558 ) ) ;
#67649 = CARTESIAN_POINT ( 'NONE',  ( -96.72723180373841956, -287.9216386109393966, -316.4413421396330364 ) ) ;
#67650 = CARTESIAN_POINT ( 'NONE',  ( -32.11699080309450238, -283.9258833961350206, -343.4098062718335882 ) ) ;
#67651 = CARTESIAN_POINT ( 'NONE',  ( -68.87779351538624439, -293.6387011420119393, -202.1158679811317995 ) ) ;
#67652 = CARTESIAN_POINT ( 'NONE',  ( 82.17447117356790898, -297.5427909045017714, -195.1407487411256341 ) ) ;
#67653 = DIRECTION ( 'NONE',  ( -0.000000000000000000, -1.000000000000000000, -0.000000000000000000 ) ) ;
#67654 = CARTESIAN_POINT ( 'NONE',  ( -40.40679947260564120, -299.9341872900681665, -194.8121571392851479 ) ) ;
#67655 = CARTESIAN_POINT ( 'NONE',  ( -35.64883519073631390, -279.2710619372849123, -197.2067988523656936 ) ) ;
#67656 = CARTESIAN_POINT ( 'NONE',  ( 37.68878881932509017, -279.5288648190948493, -268.5602934286727077 ) ) ;
#67657 = CARTESIAN_POINT ( 'NONE',  ( 32.07973605760906821, -293.1737036938523602, -303.4217676600216009 ) ) ;
#67658 = CARTESIAN_POINT ( 'NONE',  ( -95.39375475043335939, -271.4310699340612700, -224.4488868151456415 ) ) ;
#67659 = CARTESIAN_POINT ( 'NONE',  ( -3.228936006821487847, -274.6777795793782957, -336.5248053395331453 ) ) ;
#67660 = CARTESIAN_POINT ( 'NONE',  ( -71.14280196073748641, -296.8232007806758475, -335.6341335305513667 ) ) ;
#67661 = DIRECTION ( 'NONE',  ( 0.000000000000000000, -0.7071067811865472397, -0.7071067811865479058 ) ) ;
#67662 = CARTESIAN_POINT ( 'NONE',  ( -91.73677117324264429, -271.8697296988864309, -216.6975126408426604 ) ) ;
#67663 = CARTESIAN_POINT ( 'NONE',  ( 36.47025277189471382, -292.0214278169038380, -288.4645845785557299 ) ) ;
#67664 = CARTESIAN_POINT ( 'NONE',  ( -2.173684423439532498, -293.9525609186050019, -205.7048296468088040 ) ) ;
#67665 = DIRECTION ( 'NONE',  ( -1.000000000000000000, -0.000000000000000000, -0.000000000000000000 ) ) ;
#67666 = CARTESIAN_POINT ( 'NONE',  ( 31.69582339886613198, -294.6782662871694924, -294.7290245203899417 ) ) ;
#67667 = CARTESIAN_POINT ( 'NONE',  ( 160.5350683151633291, 275.0000000000000568, 20.22542485937379908 ) ) ;
#67669 = CARTESIAN_POINT ( 'NONE',  ( -10.49000150794004682, -294.6917916147372694, -338.2432679279846184 ) ) ;
#67668 = CARTESIAN_POINT ( 'NONE',  ( -85.08025831850403620, -281.7275247512647525, -328.6658078595815482 ) ) ;
#67670 = CARTESIAN_POINT ( 'NONE',  ( -2.892840669931094677, -282.6095478170842625, -339.2399569898188929 ) ) ;
#67671 = CARTESIAN_POINT ( 'NONE',  ( -12.01548698114655878, -282.2992288453663718, -199.1170261378642294 ) ) ;
#67672 = CARTESIAN_POINT ( 'NONE',  ( -110.9045639273811474, -284.5057726810414920, -247.5046716233837003 ) ) ;
#67673 = CARTESIAN_POINT ( 'NONE',  ( -91.11647521756077595, -289.2856518755714319, -218.3197691319824116 ) ) ;
#67674 = CARTESIAN_POINT ( 'NONE',  ( 37.18415559740575560, -280.2396289614213742, -286.8105527711588820 ) ) ;
#67675 = CARTESIAN_POINT ( 'NONE',  ( -49.48664179749899716, -284.5790291060191066, -197.8265591579031195 ) ) ;
#67676 = CARTESIAN_POINT ( 'NONE',  ( 16.45926741141646943, -287.2299039735248130, -325.0879318871068904 ) ) ;
#67677 = DIRECTION ( 'NONE',  ( -0.9953184226294286008, 0.000000000000000000, 0.09665007798479081924 ) ) ;
#67678 = CARTESIAN_POINT ( 'NONE',  ( 12.91441070691149662, -295.9369819510189359, -324.4752687276510983 ) ) ;
#67679 = CARTESIAN_POINT ( 'NONE',  ( -113.4902521127258836, -279.8900259178460033, -277.2958018919841834 ) ) ;
#67681 = CARTESIAN_POINT ( 'NONE',  ( -64.82013868644347099, -279.3498227320561682, -202.7074196268862920 ) ) ;
#67680 = CARTESIAN_POINT ( 'NONE',  ( 29.43293115384220826, -292.0326663717503379, -305.2832516094761104 ) ) ;
#67682 = CARTESIAN_POINT ( 'NONE',  ( 38.60663593945798766, -293.8784451657110139, -283.1236972015734068 ) ) ;
#67683 = CARTESIAN_POINT ( 'NONE',  ( -111.5787022373148858, -282.8148365000241142, -256.0116569892018674 ) ) ;
#67684 = CARTESIAN_POINT ( 'NONE',  ( -79.09116339031255905, -279.6149906452071718, -332.7291837752894139 ) ) ;
#67685 = CARTESIAN_POINT ( 'NONE',  ( -0.6504171600917483254, -293.6109337637079761, -333.8000482619797253 ) ) ;
#67686 = CARTESIAN_POINT ( 'NONE',  ( -4.479461041248472775, -296.4633562459687255, -195.3723136117041292 ) ) ;
#67687 = ORIENTED_EDGE ( 'NONE', *, *, #44800, .F. ) ;
#67688 = DIRECTION ( 'NONE',  ( 0.000000000000000000, 1.000000000000000000, 0.000000000000000000 ) ) ;
#67689 = CARTESIAN_POINT ( 'NONE',  ( 37.07085638919105719, -283.6160204865634569, -276.8700250130047493 ) ) ;
#67690 = CARTESIAN_POINT ( 'NONE',  ( -109.1049325678878006, -296.2414166074379409, -256.5822255039538504 ) ) ;
#67691 = LINE ( 'NONE', #24585, #20167 ) ;
#67692 = CARTESIAN_POINT ( 'NONE',  ( 31.98288692825983404, -278.6237833571634610, -237.0123917617631264 ) ) ;
#67693 = CARTESIAN_POINT ( 'NONE',  ( -3.527245894643499469, -297.5245468185709115, -193.6016564146562473 ) ) ;
#67694 = CARTESIAN_POINT ( 'NONE',  ( 35.37504116671787102, -288.5642618076058170, -246.4100107637281099 ) ) ;
#67695 = CARTESIAN_POINT ( 'NONE',  ( -69.97436101230287875, -289.3277194220793263, -335.6751262217861722 ) ) ;
#67696 = CARTESIAN_POINT ( 'NONE',  ( -37.02459026532761754, -281.5763177061006672, -196.6684643728150945 ) ) ;
#67697 = CARTESIAN_POINT ( 'NONE',  ( -65.98529596308397061, -299.4322596722847152, -202.1151039421012001 ) ) ;
#67698 = CARTESIAN_POINT ( 'NONE',  ( -35.63828123159275663, -278.8688838506628258, -196.9713430945191703 ) ) ;
#67699 = EDGE_LOOP ( 'NONE', ( #70324, #69808 ) ) ;
#67700 = CARTESIAN_POINT ( 'NONE',  ( -68.16509163271760485, -297.3251750284244395, -199.7659592282151948 ) ) ;
#67701 = CARTESIAN_POINT ( 'NONE',  ( -41.70114407029316084, -293.9171053130156110, -195.9980460610264856 ) ) ;
#67702 = DIRECTION ( 'NONE',  ( 0.9531768234071980039, -0.3024135303179465994, -0.000000000000000000 ) ) ;
#67703 = CARTESIAN_POINT ( 'NONE',  ( -72.40046885151168965, -290.1806441474411713, -334.5076331176156259 ) ) ;
#67704 = CARTESIAN_POINT ( 'NONE',  ( 196.1388477366602956, 72.64613238536348661, 11.79151705418648177 ) ) ;
#67705 = EDGE_CURVE ( 'NONE', #70776, #19395, #87789, .T. ) ;
#67706 = CARTESIAN_POINT ( 'NONE',  ( 3.496032565038655893, -290.7341866847588108, -206.4821110034023093 ) ) ;
#67707 = CARTESIAN_POINT ( 'NONE',  ( -81.95368129959769021, -297.0918911847159620, -212.4882258021241341 ) ) ;
#67708 = DIRECTION ( 'NONE',  ( 0.000000000000000000, 0.000000000000000000, 1.000000000000000000 ) ) ;
#67709 = CARTESIAN_POINT ( 'NONE',  ( -101.7059337997187356, -291.5289943852437773, -311.4455487226369996 ) ) ;
#67710 = CARTESIAN_POINT ( 'NONE',  ( -111.2869819898779866, -287.4805209788416391, -234.7871824221999191 ) ) ;
#67711 = CARTESIAN_POINT ( 'NONE',  ( 33.56992404336133973, -289.2424871895032084, -246.4535881379001410 ) ) ;
#67712 = CARTESIAN_POINT ( 'NONE',  ( -3.049479776392111319, -274.5977860927958432, -336.8748162184514854 ) ) ;
#67713 = CARTESIAN_POINT ( 'NONE',  ( 34.90088029841781037, -277.2399738718721096, -252.4077401820034652 ) ) ;
#67714 = CARTESIAN_POINT ( 'NONE',  ( -60.68783329882943178, -289.8268926802805368, -199.6227246393132475 ) ) ;
#67715 = CARTESIAN_POINT ( 'NONE',  ( -94.98176857742367929, -281.0867563655821186, -221.1687522319337234 ) ) ;
#67716 = ORIENTED_EDGE ( 'NONE', *, *, #48099, .T. ) ;
#67717 = CARTESIAN_POINT ( 'NONE',  ( -36.20024906065894044, -282.3860513726920090, -343.4541392499589278 ) ) ;
#67718 = CARTESIAN_POINT ( 'NONE',  ( -111.8715035675152762, -279.4041299241476963, -288.4937178898858861 ) ) ;
#67719 = CARTESIAN_POINT ( 'NONE',  ( 16.95256563256307913, -279.5994343103488973, -216.2483896918401172 ) ) ;
#67720 = CARTESIAN_POINT ( 'NONE',  ( -1.422236905112849836, -275.4579193733644047, -202.5185621987752995 ) ) ;
#67721 = EDGE_CURVE ( 'NONE', #83547, #67504, #17788, .T. ) ;
#67723 = EDGE_CURVE ( 'NONE', #27549, #56772, #82234, .T. ) ;
#67722 = APPLICATION_PROTOCOL_DEFINITION ( 'draft international standard', 'automotive_design', 1998, #20284 ) ;
#67724 = CARTESIAN_POINT ( 'NONE',  ( -64.67001702453850953, -275.2218596178875032, -199.1019123151973247 ) ) ;
#67725 = CARTESIAN_POINT ( 'NONE',  ( -21.39648532958013050, -276.7662352645559167, -200.3538533559491555 ) ) ;
#67726 = EDGE_LOOP ( 'NONE', ( #85779, #75871, #66299, #89831 ) ) ;
#67727 = AXIS2_PLACEMENT_3D ( 'NONE', #34835, #77936, #40494 ) ;
#67728 = CARTESIAN_POINT ( 'NONE',  ( -112.2375992108470228, -298.5015950462242245, -274.3114276736488932 ) ) ;
#67729 = CARTESIAN_POINT ( 'NONE',  ( -90.80882447132154311, -290.9124185237738516, -320.5899216834986873 ) ) ;
#67730 = CARTESIAN_POINT ( 'NONE',  ( -54.25397744942461742, -291.0264746411680790, -344.4957981948597876 ) ) ;
#67731 = CARTESIAN_POINT ( 'NONE',  ( 11.00442705175344749, -292.0906104290316989, -215.4615969200426946 ) ) ;
#67732 = CARTESIAN_POINT ( 'NONE',  ( 31.36965327955490324, -286.6140204605208623, -235.7449827859915956 ) ) ;
#67733 = FACE_OUTER_BOUND ( 'NONE', #36371, .T. ) ;
#67734 = CARTESIAN_POINT ( 'NONE',  ( -36.20138663600549478, -281.4374897226920211, -344.1523105634200874 ) ) ;
#67735 = CARTESIAN_POINT ( 'NONE',  ( 21.34835292803084528, -290.0422959739304360, -315.8387562628982437 ) ) ;
#67736 = CARTESIAN_POINT ( 'NONE',  ( -89.39763245738217279, -282.2811429183595351, -322.5948919052556221 ) ) ;
#67737 = CARTESIAN_POINT ( 'NONE',  ( -7.816595296067766263, -281.7625141631157817, -203.0457080379315187 ) ) ;
#67738 = CARTESIAN_POINT ( 'NONE',  ( 23.96156132175256559, -289.1105069894522330, -316.5642601842934027 ) ) ;
#67739 = CARTESIAN_POINT ( 'NONE',  ( -96.45918423570998357, -279.6448127014732563, -227.4296433448164123 ) ) ;
#67740 = CARTESIAN_POINT ( 'NONE',  ( 15.17715963397304435, -291.5684594889823984, -214.5228877008711947 ) ) ;
#67741 = CARTESIAN_POINT ( 'NONE',  ( 28.55479088422166001, -287.8373407107815751, -230.7387650182011782 ) ) ;
#67742 = CARTESIAN_POINT ( 'NONE',  ( -18.20340191925394890, -286.7846169262814442, -195.7859127869537872 ) ) ;
#67743 = CARTESIAN_POINT ( 'NONE',  ( -90.74001278311652641, -284.0030235207151463, -320.1368169741696192 ) ) ;
#67744 = EDGE_LOOP ( 'NONE', ( #14982, #22322, #32694, #31519, #64522, #64836, #24114 ) ) ;
#67745 = CARTESIAN_POINT ( 'NONE',  ( 195.4349574838196020, 27.23211070204046180, 14.00000000000008882 ) ) ;
#67746 = CARTESIAN_POINT ( 'NONE',  ( 14.57425130791220980, -294.6334574806179489, -215.1072283240156651 ) ) ;
#67747 = CARTESIAN_POINT ( 'NONE',  ( 37.29908086244962107, -292.4491193489233183, -287.2145997093907113 ) ) ;
#67748 = CARTESIAN_POINT ( 'NONE',  ( -24.29943660481183798, -275.9404235108585226, -342.4773420176054515 ) ) ;
#67749 = CARTESIAN_POINT ( 'NONE',  ( -113.2875645272479801, -296.0528614967237218, -258.2138243589183730 ) ) ;
#67750 = CARTESIAN_POINT ( 'NONE',  ( 17.26484732444187387, -291.3289833482157292, -220.8005691610107135 ) ) ;
#67751 = CARTESIAN_POINT ( 'NONE',  ( -103.4271690398474988, -295.2395170403725615, -236.9201329468618837 ) ) ;
#67752 = CARTESIAN_POINT ( 'NONE',  ( -55.12332557170220326, -293.0234003247683177, -199.1505548600890165 ) ) ;
#67753 = CARTESIAN_POINT ( 'NONE',  ( 4.669580318944723807, -293.7135962120383397, -210.2216279416927307 ) ) ;
#67754 = CARTESIAN_POINT ( 'NONE',  ( 198.6003787446688591, 25.18134682881806796, 11.03083405179678778 ) ) ;
#67755 = CARTESIAN_POINT ( 'NONE',  ( 7.784699692153664863, -292.4373024797957896, -330.4746477644270044 ) ) ;
#67756 = CARTESIAN_POINT ( 'NONE',  ( -112.3912264470853870, -298.5590368601372120, -269.8377770872875203 ) ) ;
#67757 = CARTESIAN_POINT ( 'NONE',  ( 22.15983908085178555, -289.0883344423215817, -313.0574325810163714 ) ) ;
#67758 = CARTESIAN_POINT ( 'NONE',  ( -48.23084345033734621, -279.1698128255303004, -344.9781490221671447 ) ) ;
#67759 = CARTESIAN_POINT ( 'NONE',  ( -23.02822260613217864, -275.6680284131264784, -345.6688129934878475 ) ) ;
#67760 = CARTESIAN_POINT ( 'NONE',  ( -93.09254255074064588, -272.6257236916284796, -217.3781776140207285 ) ) ;
#67761 = CARTESIAN_POINT ( 'NONE',  ( 36.12078151329666298, -279.7875446359871603, -282.3851767820270879 ) ) ;
#67762 = CARTESIAN_POINT ( 'NONE',  ( -31.53180984173248191, -275.3799670801577122, -346.3913862438355409 ) ) ;
#67763 = CARTESIAN_POINT ( 'NONE',  ( -102.9651863840894208, -295.6844126480182240, -237.1600709593430736 ) ) ;
#67764 = CARTESIAN_POINT ( 'NONE',  ( 159.4851178187871312, 15.00000000000000000, 10.00000000000000000 ) ) ;
#67765 = CARTESIAN_POINT ( 'NONE',  ( -108.6361481453368043, -273.4163851998842460, -254.2057984095889651 ) ) ;
#67766 = CARTESIAN_POINT ( 'NONE',  ( 194.3836820389603304, 26.49645583160156193, 14.46137890893106892 ) ) ;
#67768 = CARTESIAN_POINT ( 'NONE',  ( -46.17667554310626343, -273.7702700978575194, -197.8977257495770061 ) ) ;
#67767 = CARTESIAN_POINT ( 'NONE',  ( -99.34195973377948974, -287.9943343305151302, -313.1907177047527284 ) ) ;
#67769 = CARTESIAN_POINT ( 'NONE',  ( -26.14455805463359539, -288.9133496689164531, -346.5426381130156415 ) ) ;
#67770 = CARTESIAN_POINT ( 'NONE',  ( -54.25112652680952152, -299.8159086578167489, -196.9276235907035186 ) ) ;
#67771 = CARTESIAN_POINT ( 'NONE',  ( -109.2132195524827267, -294.8209521526893582, -249.5161396050932012 ) ) ;
#67772 = CARTESIAN_POINT ( 'NONE',  ( -33.07794900383075287, -282.1969327789103659, -347.0943613475226357 ) ) ;
#67773 = CARTESIAN_POINT ( 'NONE',  ( 155.0231696494687981, 19.71747416577793643, 13.29925684039281286 ) ) ;
#67774 = CARTESIAN_POINT ( 'NONE',  ( 9.489684339936221846, -280.4085116167094611, -329.0085771338789300 ) ) ;
#67775 = FACE_BOUND ( 'NONE', #34640, .T. ) ;
#67776 = CARTESIAN_POINT ( 'NONE',  ( -108.1308130345192495, -289.6018912881219194, -250.9695734453144098 ) ) ;
#67777 = CARTESIAN_POINT ( 'NONE',  ( -26.58684975546040619, -281.0536038529025973, -343.8652996948007967 ) ) ;
#67778 = CARTESIAN_POINT ( 'NONE',  ( 175.2296996224750103, 154.6894116713782807, -24.16304133878946558 ) ) ;
#67779 = CARTESIAN_POINT ( 'NONE',  ( -36.09237171215956863, 15.36528803885690664, 22.50000000000000000 ) ) ;
#67780 = CARTESIAN_POINT ( 'NONE',  ( -55.47182832744906733, -289.8186799491717238, -197.5854414335602200 ) ) ;
#67781 = CARTESIAN_POINT ( 'NONE',  ( -46.28190640407311918, -275.4568002816404260, -197.2120888475302820 ) ) ;
#67782 = CARTESIAN_POINT ( 'NONE',  ( -21.79152322614257287, -284.0621815175651932, -345.3691223273917217 ) ) ;
#67784 = CARTESIAN_POINT ( 'NONE',  ( -65.31569641794466463, -283.4282414377342434, -337.8021258867885876 ) ) ;
#67783 = CARTESIAN_POINT ( 'NONE',  ( -78.04487814606238771, -271.5894186498043155, -206.7013544275120864 ) ) ;
#67785 = CARTESIAN_POINT ( 'NONE',  ( 32.61634727392659272, -276.6749586450051765, -247.3664955464804223 ) ) ;
#67786 = CARTESIAN_POINT ( 'NONE',  ( -40.50253187497059315, -277.8957125937656087, -343.4667756798746154 ) ) ;
#67787 = ADVANCED_FACE ( 'NONE', ( #53772 ), #69374, .T. ) ;
#67788 = CARTESIAN_POINT ( 'NONE',  ( -33.14452843634265378, -284.9994731462925870, -345.2563822137155398 ) ) ;
#67789 = CIRCLE ( 'NONE', #60305, 1.000000000000000888 ) ;
#67790 = ORIENTED_EDGE ( 'NONE', *, *, #9225, .F. ) ;
#67791 = CARTESIAN_POINT ( 'NONE',  ( -112.3417001281054723, -270.5523139186827279, -270.3356821209761165 ) ) ;
#67792 = CARTESIAN_POINT ( 'NONE',  ( -0.7080456332996576396, -294.4126420152652486, -338.1032159629180569 ) ) ;
#67793 = CARTESIAN_POINT ( 'NONE',  ( -33.17142365197523191, -288.0846860420366511, -195.7819544807134378 ) ) ;
#67794 = FACE_OUTER_BOUND ( 'NONE', #57397, .T. ) ;
#67795 = CARTESIAN_POINT ( 'NONE',  ( -37.37352853689063181, -286.5523547857346784, -350.3611179825600175 ) ) ;
#67796 = CARTESIAN_POINT ( 'NONE',  ( -114.0682601330215107, -277.4930007894196251, -268.7270557508198294 ) ) ;
#67797 = CARTESIAN_POINT ( 'NONE',  ( -107.6213552519863583, -289.3305374004335704, -240.9126801753092479 ) ) ;
#67798 = CARTESIAN_POINT ( 'NONE',  ( -108.0517734583732761, -285.7997242717115682, -291.1616919183630330 ) ) ;
#67799 = CARTESIAN_POINT ( 'NONE',  ( -94.37272237598270408, -279.6524442625789106, -317.5554998544593559 ) ) ;
#67800 = CARTESIAN_POINT ( 'NONE',  ( -65.67586712538583527, -287.1140455144932275, -199.3838312484235757 ) ) ;
#67801 = CARTESIAN_POINT ( 'NONE',  ( -37.52039300842150027, -285.0545814174431598, -345.3736788903798924 ) ) ;
#67802 = CARTESIAN_POINT ( 'NONE',  ( -34.28897043574578163, -277.1814415574908139, -347.3005801976481735 ) ) ;
#67803 = CARTESIAN_POINT ( 'NONE',  ( 10.26600815775594633, -296.6710508435074303, -195.7324710267420755 ) ) ;
#67804 = CARTESIAN_POINT ( 'NONE',  ( -25.39349840143035664, -280.0337503176937730, -194.2937762386257532 ) ) ;
#67805 = CARTESIAN_POINT ( 'NONE',  ( -94.73925213247066779, -299.1314114095068817, -222.9404875693416557 ) ) ;
#67806 = CARTESIAN_POINT ( 'NONE',  ( 212.7238915819278589, 32.98517505407394168, 12.09245862095555601 ) ) ;
#67807 = CARTESIAN_POINT ( 'NONE',  ( -37.37352853689063892, -276.5519495502701943, -195.3611179825600175 ) ) ;
#67808 = CARTESIAN_POINT ( 'NONE',  ( -112.5381433073586805, -270.9350727805710335, -259.0727742121037522 ) ) ;
#67809 = DIRECTION ( 'NONE',  ( -0.000000000000000000, -0.000000000000000000, 1.000000000000000000 ) ) ;
#67810 = CARTESIAN_POINT ( 'NONE',  ( -41.86665514001207811, -276.6183232892640262, -343.2950060033076056 ) ) ;
#67811 = CARTESIAN_POINT ( 'NONE',  ( -66.09250230434403761, -274.8892274802209386, -199.3442019789883375 ) ) ;
#67812 = CARTESIAN_POINT ( 'NONE',  ( 15.58261763641016806, -281.3838802044789418, -325.9654056018807751 ) ) ;
#67813 = CARTESIAN_POINT ( 'NONE',  ( -7.793618437226421669, -290.4198249741118047, -338.2752188013716363 ) ) ;
#67814 = CARTESIAN_POINT ( 'NONE',  ( -109.6822048469219908, -297.7637299367515880, -294.6419567075516852 ) ) ;
#67815 = CARTESIAN_POINT ( 'NONE',  ( -69.34795967050554566, -296.6690523070229233, -339.9715099452233744 ) ) ;
#67816 = CARTESIAN_POINT ( 'NONE',  ( -5.278652740791745401, -294.4751928973149688, -202.7305049653961362 ) ) ;
#67817 = CARTESIAN_POINT ( 'NONE',  ( 4.392047730498685354, -280.4881251823759385, -332.5391834806800375 ) ) ;
#67818 = CARTESIAN_POINT ( 'NONE',  ( -49.39876358561404146, -281.8174174048526197, -196.9040460542461233 ) ) ;
#67819 = CARTESIAN_POINT ( 'NONE',  ( -111.9855616574490824, -270.6085108309786733, -267.5507348244821060 ) ) ;
#67820 = CARTESIAN_POINT ( 'NONE',  ( -97.40116728422712811, -285.5190525078500627, -317.2578217399354230 ) ) ;
#67821 = CARTESIAN_POINT ( 'NONE',  ( 15.26083122062464703, -285.7373727780189370, -219.3003721083325956 ) ) ;
#67822 = CARTESIAN_POINT ( 'NONE',  ( 23.67150155679529178, -280.2753533880368195, -223.5346683830870234 ) ) ;
#67823 = CARTESIAN_POINT ( 'NONE',  ( -76.02243030850807770, -209.4518847369260754, -356.5868710737057086 ) ) ;
#67824 = ORIENTED_EDGE ( 'NONE', *, *, #66944, .F. ) ;
#67825 = CARTESIAN_POINT ( 'NONE',  ( 21.93644909056341064, -286.7789687740857403, -318.5969222939634733 ) ) ;
#67826 = CARTESIAN_POINT ( 'NONE',  ( -42.67143833779803686, -285.6498094414148454, -197.5221104102778895 ) ) ;
#67827 = ORIENTED_EDGE ( 'NONE', *, *, #62258, .F. ) ;
#67828 = CARTESIAN_POINT ( 'NONE',  ( -97.79224851240952887, -284.9986797636298661, -317.5545890481214428 ) ) ;
#67829 = CARTESIAN_POINT ( 'NONE',  ( 28.05132950365664612, -276.3272678145984855, -302.9687985350306576 ) ) ;
#67830 = CARTESIAN_POINT ( 'NONE',  ( -90.56149097500754408, -290.2400402312915162, -215.0683518601522621 ) ) ;
#67831 = CARTESIAN_POINT ( 'NONE',  ( 33.07627213693600510, -281.8090052431759318, -239.4641607154334793 ) ) ;
#67832 = CARTESIAN_POINT ( 'NONE',  ( 196.7071296363290855, 19.50333209967908132, -12.79999999999999361 ) ) ;
#67833 = CARTESIAN_POINT ( 'NONE',  ( -108.9622107912893512, -280.4097785535952880, -243.8795769879390889 ) ) ;
#67834 = CARTESIAN_POINT ( 'NONE',  ( 33.15188035396288058, -281.4909244181411054, -239.4354101933971037 ) ) ;
#67835 = CARTESIAN_POINT ( 'NONE',  ( -92.05005921254146983, -288.6952119285918457, -226.6919474004047572 ) ) ;
#67836 = CARTESIAN_POINT ( 'NONE',  ( 26.08411754451436693, -23.25919466593375873, -345.2244097993914806 ) ) ;
#67837 = ORIENTED_EDGE ( 'NONE', *, *, #75080, .T. ) ;
#67838 = CARTESIAN_POINT ( 'NONE',  ( -18.53213648314174122, -278.8094562997310959, -342.7919728649139870 ) ) ;
#67839 = CARTESIAN_POINT ( 'NONE',  ( -104.8592795955056118, -255.4662412201343500, -326.3873165879509770 ) ) ;
#67840 = CARTESIAN_POINT ( 'NONE',  ( 17.00650590315697031, -280.2933951682540510, -321.6032218939701579 ) ) ;
#67841 = CARTESIAN_POINT ( 'NONE',  ( -39.16256298938664315, -297.3773215372942786, -197.2694392661224185 ) ) ;
#67842 = CARTESIAN_POINT ( 'NONE',  ( 25.66065556470347531, -293.6444961109544920, -314.5455173815605576 ) ) ;
#67843 = CARTESIAN_POINT ( 'NONE',  ( -76.15440596507517057, -208.4761271767036419, -353.6627180100991268 ) ) ;
#67845 = CARTESIAN_POINT ( 'NONE',  ( -75.14298698906080176, -287.9647261292154212, -333.7597444371619417 ) ) ;
#67844 = CARTESIAN_POINT ( 'NONE',  ( -111.3369717193388908, -271.4842549895164439, -250.7163547451768295 ) ) ;
#67846 = CARTESIAN_POINT ( 'NONE',  ( -34.22603441533227198, -296.8729777861386765, -344.5309104142584147 ) ) ;
#67847 = CARTESIAN_POINT ( 'NONE',  ( -37.29727805885298153, -287.3678590389684473, -196.8554559647179190 ) ) ;
#67848 = ORIENTED_EDGE ( 'NONE', *, *, #84552, .F. ) ;
#67849 = CARTESIAN_POINT ( 'NONE',  ( -2.174344376177569149, -293.4473542348166006, -202.1109315974390199 ) ) ;
#67850 = CARTESIAN_POINT ( 'NONE',  ( -108.4837844942666010, -284.8245598614978462, -287.0528345518507649 ) ) ;
#67851 = CARTESIAN_POINT ( 'NONE',  ( -29.09726686348604119, -296.9481435779741219, -193.7598320506033929 ) ) ;
#67852 = CARTESIAN_POINT ( 'NONE',  ( -19.43435153304433882, -293.0795312831044725, -195.5836872514845197 ) ) ;
#67853 = EDGE_CURVE ( 'NONE', #59112, #50020, #32471, .T. ) ;
#67854 = CARTESIAN_POINT ( 'NONE',  ( -30.70882872728190094, -292.6260867691669318, -193.6563834882051935 ) ) ;
#67855 = CARTESIAN_POINT ( 'NONE',  ( -106.9514523044458087, -290.4253601445953450, -292.5165272901649018 ) ) ;
#67856 = EDGE_LOOP ( 'NONE', ( #53021, #86648, #87220, #66549 ) ) ;
#67857 = CARTESIAN_POINT ( 'NONE',  ( 85.55100297371598117, -373.0521521680024648, -417.1172536214571096 ) ) ;
#67858 = CARTESIAN_POINT ( 'NONE',  ( -34.13637962752525112, -299.9522818879969464, -194.5953074871426338 ) ) ;
#67859 = CARTESIAN_POINT ( 'NONE',  ( -76.21790563120529782, -272.3399534283387311, -204.2949139669707677 ) ) ;
#67860 = ADVANCED_FACE ( 'NONE', ( #82638 ), #36897, .T. ) ;
#67861 = CARTESIAN_POINT ( 'NONE',  ( 1.215027249381221086, -281.5826070308897329, -332.6841806656848917 ) ) ;
#67862 = EDGE_LOOP ( 'NONE', ( #44553, #11540, #33262, #13582 ) ) ;
#67863 = CARTESIAN_POINT ( 'NONE',  ( -77.78789002591544488, -277.0872178091924525, -335.8724981378930465 ) ) ;
#67864 = VECTOR ( 'NONE', #36212, 1000.000000000000000 ) ;
#67865 = CARTESIAN_POINT ( 'NONE',  ( -102.7299144268593096, -271.4139592284410583, -236.0332178671868633 ) ) ;
#67866 = CARTESIAN_POINT ( 'NONE',  ( -97.41904388694345585, -281.0126603772627618, -226.7540285483705418 ) ) ;
#67867 = CARTESIAN_POINT ( 'NONE',  ( 33.26583397292183975, -273.9908022776962753, -293.2836311160724563 ) ) ;
#67868 = CARTESIAN_POINT ( 'NONE',  ( -106.3553288552089668, -297.4244227226124622, -295.4954613460365636 ) ) ;
#67869 = CARTESIAN_POINT ( 'NONE',  ( -72.02972481751037037, -274.5231957475813260, -205.8053883274620830 ) ) ;
#67870 = CARTESIAN_POINT ( 'NONE',  ( -82.51290234280770619, -299.0471689013976402, -208.9277779076990953 ) ) ;
#67871 = CARTESIAN_POINT ( 'NONE',  ( 23.17436010557835502, -272.9622424397318809, -225.4588545732813714 ) ) ;
#67872 = CARTESIAN_POINT ( 'NONE',  ( 34.58197312765408782, -294.0304501379856674, -257.2195276941404813 ) ) ;
#67873 = CARTESIAN_POINT ( 'NONE',  ( -14.64758602862610992, -290.9268476257366842, -200.3586030174679138 ) ) ;
#67874 = DIRECTION ( 'NONE',  ( 0.000000000000000000, 0.000000000000000000, 1.000000000000000000 ) ) ;
#67875 = CARTESIAN_POINT ( 'NONE',  ( -22.94426238458952483, -277.3651781578207647, -345.9946271480175142 ) ) ;
#67876 = CARTESIAN_POINT ( 'NONE',  ( -54.21359685667891171, -273.9960433975784895, -199.3376070494722967 ) ) ;
#67877 = CARTESIAN_POINT ( 'NONE',  ( 23.00354655200976595, -280.8695673351771802, -317.4115236475249162 ) ) ;
#67878 = CARTESIAN_POINT ( 'NONE',  ( 36.55959091783275028, -295.7291575834854029, -284.1649664084121696 ) ) ;
#67879 = FACE_OUTER_BOUND ( 'NONE', #13027, .T. ) ;
#67880 = CARTESIAN_POINT ( 'NONE',  ( -108.5202381618143050, -283.9726576883808207, -253.3892338750122235 ) ) ;
#67881 = CARTESIAN_POINT ( 'NONE',  ( -109.7328760552722287, -282.2922277438636911, -290.5983627637394875 ) ) ;
#67882 = CARTESIAN_POINT ( 'NONE',  ( 23.55001489868414666, -273.5565685099415418, -229.0157055706463893 ) ) ;
#67883 = CARTESIAN_POINT ( 'NONE',  ( 35.73046154822215215, -283.3347252669242380, -253.4097918303002075 ) ) ;
#67884 = ADVANCED_BREP_SHAPE_REPRESENTATION ( '', ( #91539, #18940 ), #2252 ) ;
#67885 = DIRECTION ( 'NONE',  ( 0.9531768234071978929, -0.3024135303179465439, 0.000000000000000000 ) ) ;
#67886 = DIRECTION ( 'NONE',  ( 0.3262578496237564796, 0.000000000000000000, 0.9452808130703185263 ) ) ;
#67887 = CARTESIAN_POINT ( 'NONE',  ( -96.30394343284984870, -271.6071262299524847, -222.0717842561393525 ) ) ;
#67888 = CARTESIAN_POINT ( 'NONE',  ( -74.40939965479820728, -279.5441218691685776, -335.7523565334744831 ) ) ;
#67889 = DIRECTION ( 'NONE',  ( 0.000000000000000000, 1.000000000000000000, 0.000000000000000000 ) ) ;
#67890 = CARTESIAN_POINT ( 'NONE',  ( -26.84578467067315444, -288.1046494482942535, -195.4811529616483483 ) ) ;
#67891 = CARTESIAN_POINT ( 'NONE',  ( 156.1688672180497690, 17.06233518523552917, -10.31625060074404487 ) ) ;
#67892 = CARTESIAN_POINT ( 'NONE',  ( -72.57218199827893557, -287.5183519005814787, -336.5857462262574700 ) ) ;
#67893 = DIRECTION ( 'NONE',  ( 0.000000000000000000, 0.000000000000000000, 1.000000000000000000 ) ) ;
#67894 = CARTESIAN_POINT ( 'NONE',  ( -104.0732405473320483, -295.7584767285530916, -239.6769061020408174 ) ) ;
#67895 = CARTESIAN_POINT ( 'NONE',  ( -0.3969470701810811075, -286.6954378144469615, -334.8093351585907840 ) ) ;
#67896 = CARTESIAN_POINT ( 'NONE',  ( 133.9787772367566561, 181.9811788097603937, -239.6702418147338562 ) ) ;
#67897 = CARTESIAN_POINT ( 'NONE',  ( -98.83747485365626062, -293.9693470199541707, -313.2944423443192932 ) ) ;
#67898 = CARTESIAN_POINT ( 'NONE',  ( 26.56774214911342114, -285.4793481802478823, -228.6683015739363043 ) ) ;
#67899 = CARTESIAN_POINT ( 'NONE',  ( 35.93663529450428484, -283.2720286767190601, -279.5377115546359050 ) ) ;
#67900 = CARTESIAN_POINT ( 'NONE',  ( -5.895603417133877144, -280.8842764895841242, -339.5356582282058753 ) ) ;
#67901 = CARTESIAN_POINT ( 'NONE',  ( -78.17441562460498972, -289.6179411365828287, -330.9338669709941314 ) ) ;
#67902 = CARTESIAN_POINT ( 'NONE',  ( -4.097492321258143555, -281.9246379407643417, -204.6950212470591453 ) ) ;
#67903 = CARTESIAN_POINT ( 'NONE',  ( 25.70335987136919087, -282.8649091829875033, -307.5816233393840662 ) ) ;
#67904 = CARTESIAN_POINT ( 'NONE',  ( 11.37215196813228069, -290.3605622479366275, -327.8534428077932716 ) ) ;
#67905 = CARTESIAN_POINT ( 'NONE',  ( -113.8421273244509280, -272.9926298029299119, -261.7920497570210046 ) ) ;
#67906 = CARTESIAN_POINT ( 'NONE',  ( -94.14526433434653541, -273.2593801714742199, -218.3574691540785579 ) ) ;
#67907 = CARTESIAN_POINT ( 'NONE',  ( -41.71383107583249483, -293.9768337946600241, -195.7934981620775261 ) ) ;
#67908 = DIRECTION ( 'NONE',  ( 0.000000000000000000, -1.000000000000000000, 0.000000000000000000 ) ) ;
#67909 = CARTESIAN_POINT ( 'NONE',  ( 35.78497577281001440, -284.2662352645559167, -287.0191576251351080 ) ) ;
#67910 = EDGE_CURVE ( 'NONE', #75307, #26750, #48993, .T. ) ;
#67911 = CARTESIAN_POINT ( 'NONE',  ( 36.92034388086303665, -273.7051210497410239, -282.3136704404327020 ) ) ;
#67912 = EDGE_CURVE ( 'NONE', #68073, #22603, #76226, .T. ) ;
#67913 = DIRECTION ( 'NONE',  ( 8.659560562355027768E-17, 0.7071067811865398012, -0.7071067811865552333 ) ) ;
#67914 = CARTESIAN_POINT ( 'NONE',  ( -103.1485327335104500, -295.4583696193757305, -231.8397191248259617 ) ) ;
#67915 = CARTESIAN_POINT ( 'NONE',  ( -105.8481477381913578, -291.7872890314100687, -297.9446155939880327 ) ) ;
#67916 = CARTESIAN_POINT ( 'NONE',  ( -8.923555251079450912, -273.7824066312638251, -202.9550551376902376 ) ) ;
#67917 = CARTESIAN_POINT ( 'NONE',  ( -96.31160387745562446, -291.4574693901413411, -314.5778509817639588 ) ) ;
#67918 = CARTESIAN_POINT ( 'NONE',  ( -75.11119822966473691, -292.4771540352930401, -207.5573976376408893 ) ) ;
#67919 = CARTESIAN_POINT ( 'NONE',  ( -48.45907662313171471, -284.9557535613526511, -343.5347331148200851 ) ) ;
#67920 = CARTESIAN_POINT ( 'NONE',  ( -64.19883188903861537, -293.1339156866479811, -198.7700573036570120 ) ) ;
#67921 = CARTESIAN_POINT ( 'NONE',  ( -39.21650298078071728, -293.3442860848596752, -193.8642898326153272 ) ) ;
#67922 = CARTESIAN_POINT ( 'NONE',  ( 24.42612397261670765, -293.9240514454459685, -309.3628266954221431 ) ) ;
#67923 = CARTESIAN_POINT ( 'NONE',  ( 0.02656974400907759562, -290.5553912152586236, -335.4486944531389554 ) ) ;
#67924 = CARTESIAN_POINT ( 'NONE',  ( 33.17209381374411237, -281.3243500973783853, -239.4288554009896188 ) ) ;
#67925 = CARTESIAN_POINT ( 'NONE',  ( -40.35782140593648393, -296.0944997354601469, -194.8101823289173353 ) ) ;
#67926 = CARTESIAN_POINT ( 'NONE',  ( -106.6781908969197730, -284.8151411543809104, -236.8730446974805091 ) ) ;
#67927 = CARTESIAN_POINT ( 'NONE',  ( 25.37985504928040470, -278.0810450631452113, -310.9268726455360934 ) ) ;
#67928 = CARTESIAN_POINT ( 'NONE',  ( -78.61250283441957265, -282.4167719108331767, -331.0558570297703795 ) ) ;
#67929 = AXIS2_PLACEMENT_3D ( 'NONE', #86745, #21429, #35652 ) ;
#67930 = CARTESIAN_POINT ( 'NONE',  ( -10.68046693611383269, -284.3995729524770013, -200.2045769020429873 ) ) ;
#67931 = CARTESIAN_POINT ( 'NONE',  ( -69.79380305693813114, -275.6144242129291797, -338.8382095829550167 ) ) ;
#67932 = CARTESIAN_POINT ( 'NONE',  ( 128.9467878515196162, -299.5541904835127980, -190.0176033293537898 ) ) ;
#67933 = CARTESIAN_POINT ( 'NONE',  ( -6.012240014580857661, -282.1366229225249072, -336.3783140037922976 ) ) ;
#67934 = CARTESIAN_POINT ( 'NONE',  ( -5.125019354807623273, -281.6719430170912801, -200.8622388538459234 ) ) ;
#67935 = CARTESIAN_POINT ( 'NONE',  ( 31.21705024087159686, -286.1651879147840418, -235.8282646377669209 ) ) ;
#67936 = CARTESIAN_POINT ( 'NONE',  ( 32.50368154035151491, -295.6354206608824029, -295.0013746899238072 ) ) ;
#67937 = CARTESIAN_POINT ( 'NONE',  ( 24.66393884032850181, -276.5591347244908320, -226.0472569867062589 ) ) ;
#67938 = CARTESIAN_POINT ( 'NONE',  ( 32.09837933787137132, -276.4523561422292914, -238.1200121733180026 ) ) ;
#67939 = CARTESIAN_POINT ( 'NONE',  ( -48.60993446628410197, -277.0328083270072739, -342.5375853563188002 ) ) ;
#67940 = CARTESIAN_POINT ( 'NONE',  ( -36.48184718728297327, -300.0630971103087177, -195.5274819368085275 ) ) ;
#67941 = CARTESIAN_POINT ( 'NONE',  ( 10.21471392157809177, -284.7097257643019361, -212.5820914579276746 ) ) ;
#67942 = CARTESIAN_POINT ( 'NONE',  ( -108.0484753211601259, -291.7879597478672622, -298.7687288566094139 ) ) ;
#67943 = CARTESIAN_POINT ( 'NONE',  ( 33.95158964912825894, -292.2475451420747277, -253.2342829545661118 ) ) ;
#67944 = EDGE_LOOP ( 'NONE', ( #62761, #6231, #78786 ) ) ;
#67945 = CARTESIAN_POINT ( 'NONE',  ( -0.07651123015015320883, -292.2296127269679573, -207.5646755421059311 ) ) ;
#67946 = EDGE_LOOP ( 'NONE', ( #5888, #35959, #50605, #86560 ) ) ;
#67947 = CARTESIAN_POINT ( 'NONE',  ( 12.22654771181180422, -289.4604863441891212, -328.8801859431951584 ) ) ;
#67948 = CARTESIAN_POINT ( 'NONE',  ( -69.79300284164453672, -280.2645642908326522, -204.8430110196242993 ) ) ;
#67949 = CARTESIAN_POINT ( 'NONE',  ( -110.5090319631680558, -295.1820766518945902, -293.3840905849748424 ) ) ;
#67950 = CARTESIAN_POINT ( 'NONE',  ( 37.61840056338752447, -287.9880703834617179, -253.1476460686504311 ) ) ;
#67951 = CARTESIAN_POINT ( 'NONE',  ( -103.0298307889525802, -284.4524052199699327, -302.3701277377415977 ) ) ;
#67952 = CARTESIAN_POINT ( 'NONE',  ( -71.36758396777378266, -196.0736500916017349, -360.3844923773536379 ) ) ;
#67953 = CARTESIAN_POINT ( 'NONE',  ( 200.3228602561044909, 293.1909332922194835, -82.91689554719077648 ) ) ;
#67954 = CARTESIAN_POINT ( 'NONE',  ( 183.8917990829111204, 260.9239217872068934, -151.0172562811493435 ) ) ;
#67955 = CARTESIAN_POINT ( 'NONE',  ( -24.31086291543331512, -276.0788206443075978, -342.4043408777426407 ) ) ;
#67956 = CARTESIAN_POINT ( 'NONE',  ( -100.8574957138548740, -276.9714722583235584, -307.0687015684266612 ) ) ;
#67957 = CARTESIAN_POINT ( 'NONE',  ( -64.88855040576572719, -273.3687554889528428, -198.4656779917778522 ) ) ;
#67958 = CARTESIAN_POINT ( 'NONE',  ( 197.7401110981591046, 281.6830570221753192, -110.4716931870877232 ) ) ;
#67959 = CARTESIAN_POINT ( 'NONE',  ( -111.3546582770964619, -276.9923150778280387, -289.7873722607557170 ) ) ;
#67960 = VERTEX_POINT ( 'NONE', #47102 ) ;
#67961 = CARTESIAN_POINT ( 'NONE',  ( -90.63335162943880619, -290.3251890686217394, -320.4148713803528494 ) ) ;
#67962 = CARTESIAN_POINT ( 'NONE',  ( -85.12400900874098397, -298.2141399372649175, -210.1862912023570118 ) ) ;
#67963 = CARTESIAN_POINT ( 'NONE',  ( -60.13584441126318580, -298.2568854244454997, -196.8212600872328721 ) ) ;
#67964 = CARTESIAN_POINT ( 'NONE',  ( -61.01115929978592334, -295.5346636623442009, -339.4708770377285418 ) ) ;
#67965 = ORIENTED_EDGE ( 'NONE', *, *, #29049, .T. ) ;
#67966 = CARTESIAN_POINT ( 'NONE',  ( -7.127621448421942674, -278.5790495386513044, -339.6313273649662960 ) ) ;
#67967 = CARTESIAN_POINT ( 'NONE',  ( -37.32056822534475060, -282.5595136838723533, -347.3126315705792990 ) ) ;
#67968 = CARTESIAN_POINT ( 'NONE',  ( -92.95218477867335594, -278.9545911955683550, -318.1282622478202597 ) ) ;
#67969 = CARTESIAN_POINT ( 'NONE',  ( 19.13921014235693008, -278.0116105886222613, -321.2124846674767582 ) ) ;
#67970 = CARTESIAN_POINT ( 'NONE',  ( -109.8079439713880276, -271.2105919967353884, -256.6963271181957680 ) ) ;
#67971 = FACE_OUTER_BOUND ( 'NONE', #27218, .T. ) ;
#67972 = CARTESIAN_POINT ( 'NONE',  ( -99.46884663712525310, -279.2485240209946369, -231.9343046221575548 ) ) ;
#67973 = CARTESIAN_POINT ( 'NONE',  ( -73.87711823577588177, -274.3827969602620556, -202.7052058461952413 ) ) ;
#67974 = CARTESIAN_POINT ( 'NONE',  ( -43.16159424032478853, -287.8090210531993307, -346.6462876116061693 ) ) ;
#67975 = EDGE_CURVE ( 'NONE', #29329, #56700, #53580, .T. ) ;
#67976 = CARTESIAN_POINT ( 'NONE',  ( -94.51991033661415997, -275.2241708475329460, -221.8062666635315736 ) ) ;
#67977 = CARTESIAN_POINT ( 'NONE',  ( 20.36325729342618374, -274.8091730481162358, -320.4682806281419403 ) ) ;
#67978 = CARTESIAN_POINT ( 'NONE',  ( 208.6208076322478746, 32.98517505407394168, 12.09245862095555601 ) ) ;
#67979 = CARTESIAN_POINT ( 'NONE',  ( -110.2845109548321005, -289.6667531334592240, -276.6335987572646786 ) ) ;
#67980 = CARTESIAN_POINT ( 'NONE',  ( -113.8033912855467804, -283.7982951701727643, -278.5417397048719295 ) ) ;
#67981 = CARTESIAN_POINT ( 'NONE',  ( 21.80639121950892800, -280.4084696783950221, -314.8733706511301307 ) ) ;
#67983 = CARTESIAN_POINT ( 'NONE',  ( -68.12122013930522257, -283.7246268291344222, -202.5825420988205678 ) ) ;
#67982 = CARTESIAN_POINT ( 'NONE',  ( 18.42281383825081775, -279.4483301238203694, -222.3241270821210094 ) ) ;
#67984 = CARTESIAN_POINT ( 'NONE',  ( -86.25476746883335011, -291.7304969609512568, -327.2838668155660002 ) ) ;
#67985 = CARTESIAN_POINT ( 'NONE',  ( 26.79843078234099352, -282.2720014819543053, -234.6795525648647356 ) ) ;
#67986 = CARTESIAN_POINT ( 'NONE',  ( 212.3569123273291268, -142.7221692137691775, -10.75739200365177695 ) ) ;
#67987 = CARTESIAN_POINT ( 'NONE',  ( -44.36597912735508231, -281.5393353125747353, -346.2894771678300003 ) ) ;
#67988 = CARTESIAN_POINT ( 'NONE',  ( 34.77388202715069099, -295.2866542647110464, -249.7147806820009919 ) ) ;
#67989 = CARTESIAN_POINT ( 'NONE',  ( -79.33189979869551678, -277.7340169711944782, -206.9671569916252736 ) ) ;
#67990 = CIRCLE ( 'NONE', #48305, 4.025000000000000355 ) ;
#67991 = CARTESIAN_POINT ( 'NONE',  ( -30.35922307239078322, -284.9641743501890119, -345.2027737658839897 ) ) ;
#67992 = CARTESIAN_POINT ( 'NONE',  ( -39.80257052418233599, -229.5268262511776527, 22.47499999999998721 ) ) ;
#67993 = CARTESIAN_POINT ( 'NONE',  ( -58.55821692027766545, -293.7000674796388466, -197.8409579521736532 ) ) ;
#67994 = CARTESIAN_POINT ( 'NONE',  ( 25.65071260390737251, -274.1016340842912200, -311.1625599911782274 ) ) ;
#67995 = CARTESIAN_POINT ( 'NONE',  ( 16.19402474984885387, -285.9860469761973150, -215.2422919611237830 ) ) ;
#67996 = CARTESIAN_POINT ( 'NONE',  ( -84.32281430234569086, -289.7929009646389886, -213.4470131931893491 ) ) ;
#67997 = CARTESIAN_POINT ( 'NONE',  ( -48.18343439339133027, -283.1093320178187582, -435.6442049081568939 ) ) ;
#67998 = CARTESIAN_POINT ( 'NONE',  ( -13.64210883320424550, -275.4229271545212328, -339.9816481934057606 ) ) ;
#67999 = CARTESIAN_POINT ( 'NONE',  ( -42.49878882750282827, -293.2574717372093573, -344.4169747200843972 ) ) ;
#68000 = CARTESIAN_POINT ( 'NONE',  ( 209.8744251295252354, 28.03846817292548366, 10.50000000000000000 ) ) ;
#68001 = CARTESIAN_POINT ( 'NONE',  ( 1.365254254040420667, -291.0388908463314692, -204.5399510668778760 ) ) ;
#68002 = CARTESIAN_POINT ( 'NONE',  ( -101.6988352794953272, -286.6423603212411422, -234.1370966021339086 ) ) ;
#68003 = CARTESIAN_POINT ( 'NONE',  ( -23.51857418612149075, -287.1177954561270553, -345.1332922237016305 ) ) ;
#68004 = CARTESIAN_POINT ( 'NONE',  ( 18.20915749410774254, -288.2948384041913528, -222.0964607717205865 ) ) ;
#68005 = CARTESIAN_POINT ( 'NONE',  ( 191.4749582765727212, 14.19731191252289015, 13.00000000000000178 ) ) ;
#68006 = CARTESIAN_POINT ( 'NONE',  ( 33.24040722790052627, -288.6110441941652311, -289.8045471496445771 ) ) ;
#68007 = CARTESIAN_POINT ( 'NONE',  ( 32.92701375854250045, -295.8843552410523330, -297.5771913473021755 ) ) ;
#68008 = CARTESIAN_POINT ( 'NONE',  ( 179.7289557593406357, 276.0000000000000568, -24.91818181818184641 ) ) ;
#68009 = CARTESIAN_POINT ( 'NONE',  ( 39.24273979168306425, -288.7360698089669881, -268.6781801777773353 ) ) ;
#68010 = CARTESIAN_POINT ( 'NONE',  ( -20.47184734261383809, -274.9171282316470979, -344.0675230881357720 ) ) ;
#68011 = CARTESIAN_POINT ( 'NONE',  ( -108.6352528280842620, -278.5165877008970483, -299.3951262290981390 ) ) ;
#68012 = CARTESIAN_POINT ( 'NONE',  ( 15.15001990267774445, -280.4353872017491085, -213.9822642933030465 ) ) ;
#68013 = CARTESIAN_POINT ( 'NONE',  ( -41.99552101784625080, -299.9730955149311171, -195.8615290241952778 ) ) ;
#68014 = CARTESIAN_POINT ( 'NONE',  ( -43.30930410892831617, -271.8587292610232566, -505.8153911613401306 ) ) ;
#68015 = CARTESIAN_POINT ( 'NONE',  ( -16.59483519063446622, -284.3199027427820056, -198.2334636998320150 ) ) ;
#68016 = CARTESIAN_POINT ( 'NONE',  ( 160.5350683151633291, 215.0000000000000568, 20.22542485937379908 ) ) ;
#68017 = CARTESIAN_POINT ( 'NONE',  ( -107.4382629279140815, -276.3702192487625098, -294.9576466081902595 ) ) ;
#68018 = EDGE_CURVE ( 'NONE', #16726, #11326, #39144, .T. ) ;
#68019 = CARTESIAN_POINT ( 'NONE',  ( 23.47030784637063050, -280.1498402592361572, -314.2793817525225677 ) ) ;
#68020 = ADVANCED_FACE ( 'NONE', ( #18721, #47584 ), #39065, .F. ) ;
#68021 = CARTESIAN_POINT ( 'NONE',  ( 219.8344101925596021, 35.72494958537217968, -7.000000000000000000 ) ) ;
#68022 = CARTESIAN_POINT ( 'NONE',  ( -41.36740103434616600, -275.5818269897894766, -346.5746112612732190 ) ) ;
#68023 = CARTESIAN_POINT ( 'NONE',  ( -96.95801376481071543, -297.4714418944759018, -313.7024241678608973 ) ) ;
#68024 = CARTESIAN_POINT ( 'NONE',  ( -16.24014190140286118, -281.7060405804369907, -344.1468828225698644 ) ) ;
#68025 = CARTESIAN_POINT ( 'NONE',  ( -68.15742442424215142, -298.5785342241073295, -203.9109760038682566 ) ) ;
#68026 = CARTESIAN_POINT ( 'NONE',  ( -48.91205145469294280, -299.2230245407114353, -194.6809123958559269 ) ) ;
#68027 = CARTESIAN_POINT ( 'NONE',  ( -65.81747857712534255, -273.3357858488736838, -203.1211185138928386 ) ) ;
#68028 = CARTESIAN_POINT ( 'NONE',  ( 32.45594189482856251, -295.9111951901935527, -297.9494606870847520 ) ) ;
#68029 = CARTESIAN_POINT ( 'NONE',  ( 39.09083458752916584, -287.8408934426537940, -280.1210784354585712 ) ) ;
#68030 = CARTESIAN_POINT ( 'NONE',  ( -107.1723533280117664, -277.0058302471460365, -241.4994813475094304 ) ) ;
#68031 = CARTESIAN_POINT ( 'NONE',  ( -75.66552285833041935, -289.3822901575002788, -337.1464802698899348 ) ) ;
#68032 = CARTESIAN_POINT ( 'NONE',  ( 5.974172654105434077, -287.5073803721600143, -329.4763519531848601 ) ) ;
#68033 = CARTESIAN_POINT ( 'NONE',  ( -33.61265125226293549, -290.0989374305921160, -195.4538763760898235 ) ) ;
#68034 = EDGE_LOOP ( 'NONE', ( #48854, #87851, #11703, #9827, #74971 ) ) ;
#68035 = CARTESIAN_POINT ( 'NONE',  ( -114.4693872376281121, -273.8646567567205921, -270.3778293100139649 ) ) ;
#68036 = CARTESIAN_POINT ( 'NONE',  ( 10.15051113916259773, -287.8843490789424777, -325.9480786204479728 ) ) ;
#68037 = DIRECTION ( 'NONE',  ( -0.8457827187922973833, -0.5335274993777826547, 0.000000000000000000 ) ) ;
#68038 = CARTESIAN_POINT ( 'NONE',  ( -113.9726313964366398, -285.4262601498192566, -275.7133541240098111 ) ) ;
#68039 = CARTESIAN_POINT ( 'NONE',  ( 27.85886593504272213, -292.0781285254188901, -229.7426767115387634 ) ) ;
#68040 = CARTESIAN_POINT ( 'NONE',  ( 33.57236284135233007, -282.7933954745735150, -242.3310736313474365 ) ) ;
#68041 = CARTESIAN_POINT ( 'NONE',  ( -28.30001377769427862, -281.4796305174583040, -194.3371446734178107 ) ) ;
#68042 = CARTESIAN_POINT ( 'NONE',  ( -88.89579363589730576, -283.6343667361678058, -322.1154870453477201 ) ) ;
#68043 = CARTESIAN_POINT ( 'NONE',  ( -110.3457092059037734, -296.2438530954198086, -294.8440642628838191 ) ) ;
#68044 = CARTESIAN_POINT ( 'NONE',  ( -76.84330527862451277, -274.8261163084321765, -208.3863919401575515 ) ) ;
#68045 = CARTESIAN_POINT ( 'NONE',  ( 21.49459017924854720, -290.9388526922273286, -224.4041811176136605 ) ) ;
#68046 = CARTESIAN_POINT ( 'NONE',  ( -38.07099108983459956, -272.8377349151577391, -196.9676670429302874 ) ) ;
#68047 = VERTEX_POINT ( 'NONE', #53288 ) ;
#68048 = CARTESIAN_POINT ( 'NONE',  ( 140.6539576904058606, 275.0000000000000568, -12.50000000000000000 ) ) ;
#68049 = CARTESIAN_POINT ( 'NONE',  ( -76.87149117972481349, -285.5057223933551427, -333.4990821760551967 ) ) ;
#68050 = CARTESIAN_POINT ( 'NONE',  ( 21.14088101435581990, -295.3032293000255777, -319.9724091729534621 ) ) ;
#68051 = CARTESIAN_POINT ( 'NONE',  ( -105.3056440876494264, -284.8422927826481441, -297.4208877177229624 ) ) ;
#68052 = CARTESIAN_POINT ( 'NONE',  ( -20.19037303947784778, -275.8958727986864687, -345.2398092751535614 ) ) ;
#68053 = CARTESIAN_POINT ( 'NONE',  ( -4.655015081991387582, -293.1229551579453982, -200.7558494476321869 ) ) ;
#68054 = CARTESIAN_POINT ( 'NONE',  ( 38.46619441944143603, -285.7069203248997837, -271.5558411501484102 ) ) ;
#68055 = AXIS2_PLACEMENT_3D ( 'NONE', #78640, #84776, #27035 ) ;
#68056 = CARTESIAN_POINT ( 'NONE',  ( 13.26138474120823929, -293.0707595175329061, -212.3518765364509306 ) ) ;
#68057 = CARTESIAN_POINT ( 'NONE',  ( -100.3200380702444647, -290.3769257703779658, -307.4176524460082192 ) ) ;
#68058 = CARTESIAN_POINT ( 'NONE',  ( 184.3556211049944409, 2.982772324107381579, 9.000000000000000000 ) ) ;
#68059 = DIRECTION ( 'NONE',  ( -0.000000000000000000, -0.000000000000000000, 1.000000000000000000 ) ) ;
#68060 = CARTESIAN_POINT ( 'NONE',  ( 199.1258471188012891, 285.7378598522153084, -96.31343096893938593 ) ) ;
#68061 = VECTOR ( 'NONE', #20806, 1000.000000000000000 ) ;
#68062 = CARTESIAN_POINT ( 'NONE',  ( -105.1589923710728129, -285.6160149279586449, -305.4552379626754828 ) ) ;
#68063 = CARTESIAN_POINT ( 'NONE',  ( -55.56934967048407970, -277.3380690714490129, -190.3538533559490702 ) ) ;
#68064 = VERTEX_POINT ( 'NONE', #3104 ) ;
#68065 = CARTESIAN_POINT ( 'NONE',  ( -104.4015821500162389, -283.0755834202888082, -299.9786515715932751 ) ) ;
#68066 = CARTESIAN_POINT ( 'NONE',  ( -113.2790060983146390, -278.0609958136691944, -282.9813340477207930 ) ) ;
#68067 = CARTESIAN_POINT ( 'NONE',  ( -86.71234504026892864, -281.3639507542870319, -214.1244053769936500 ) ) ;
#68068 = CARTESIAN_POINT ( 'NONE',  ( 181.7509201127585641, 251.9238600837264812, -165.7362594150378072 ) ) ;
#68069 = CARTESIAN_POINT ( 'NONE',  ( 0.5601939280280614497, -281.1320317273629712, -336.7241987376779093 ) ) ;
#68070 = CARTESIAN_POINT ( 'NONE',  ( -22.09988701013485368, -284.2683207579281088, -197.2359498752210527 ) ) ;
#68071 = CARTESIAN_POINT ( 'NONE',  ( -92.29287814772024490, -275.1371476508344358, -218.1821028393644895 ) ) ;
#68072 = CARTESIAN_POINT ( 'NONE',  ( -66.07156677837504333, -295.9309451761309333, -337.5368814992067996 ) ) ;
#68073 = VERTEX_POINT ( 'NONE', #39522 ) ;
#68074 = CARTESIAN_POINT ( 'NONE',  ( 36.13426802308160291, -292.2784513809542091, -273.5268045503592589 ) ) ;
#68075 = CARTESIAN_POINT ( 'NONE',  ( -112.6920800975441210, -279.0105158767562443, -285.7765014058771271 ) ) ;
#68076 = CARTESIAN_POINT ( 'NONE',  ( -21.93402851751446292, -274.2551363543284424, -199.0056440822282298 ) ) ;
#68077 = CARTESIAN_POINT ( 'NONE',  ( 34.43729592382244675, -274.1294622653417719, -243.3561511257005918 ) ) ;
#68078 = DIRECTION ( 'NONE',  ( 0.000000000000000000, 0.000000000000000000, 1.000000000000000000 ) ) ;
#68079 = CARTESIAN_POINT ( 'NONE',  ( -9.249494481875080609, -272.4190927161547506, -200.7666451320033332 ) ) ;
#68080 = CARTESIAN_POINT ( 'NONE',  ( -6.022488948093698724, -296.0737774010196972, -340.0584156749062004 ) ) ;
#68081 = CARTESIAN_POINT ( 'NONE',  ( 153.3309649087729838, 129.0860594806759423, 12.69538652463440442 ) ) ;
#68082 = CARTESIAN_POINT ( 'NONE',  ( -43.21052260110369758, -280.7959546627067766, -507.6442049081571213 ) ) ;
#68083 = CARTESIAN_POINT ( 'NONE',  ( -76.27970941358364598, -284.6653751929001146, -332.5344097842944393 ) ) ;
#68084 = CARTESIAN_POINT ( 'NONE',  ( -112.8939062428196252, -286.2094609425076897, -278.4751899405060271 ) ) ;
#68085 = CARTESIAN_POINT ( 'NONE',  ( -97.62110101696028153, -283.3248167661758998, -311.8049650682105494 ) ) ;
#68086 = CARTESIAN_POINT ( 'NONE',  ( 18.02203024092520423, -274.6415159115558140, -319.1787189590065736 ) ) ;
#68087 = CARTESIAN_POINT ( 'NONE',  ( 29.26971607245713258, -283.8505789622883526, -303.2465046600732421 ) ) ;
#68088 = CARTESIAN_POINT ( 'NONE',  ( -71.99719536520285601, -275.9989487384877975, -335.4115308088791494 ) ) ;
#68089 = CARTESIAN_POINT ( 'NONE',  ( 22.52535353554809205, -276.0434627677731214, -228.0290874512854487 ) ) ;
#68090 = CARTESIAN_POINT ( 'NONE',  ( 185.2519943799831879, 3.000000000000000444, -9.000000000000001776 ) ) ;
#68091 = CARTESIAN_POINT ( 'NONE',  ( -25.43072538397962035, -281.0031068117947370, -194.4513854001695279 ) ) ;
#68092 = CARTESIAN_POINT ( 'NONE',  ( -1.169915738527468330, -281.0113986848400600, -202.4558242459682162 ) ) ;
#68093 = ORIENTED_EDGE ( 'NONE', *, *, #5615, .T. ) ;
#68094 = ADVANCED_FACE ( 'NONE', ( #12079 ), #67186, .T. ) ;
#68095 = FACE_OUTER_BOUND ( 'NONE', #36012, .T. ) ;
#68096 = CARTESIAN_POINT ( 'NONE',  ( -5.317921177660586807, -288.3294705759100793, -201.6968400351543096 ) ) ;
#68097 = CARTESIAN_POINT ( 'NONE',  ( -66.12606293550669534, -294.6359747032634573, -337.6222671332523078 ) ) ;
#68098 = CARTESIAN_POINT ( 'NONE',  ( -111.1320119292167732, -290.1725358431882569, -248.7208159749096126 ) ) ;
#68099 = CARTESIAN_POINT ( 'NONE',  ( 35.27405704044780776, -285.9791160856950114, -284.7417650910822431 ) ) ;
#68101 = CARTESIAN_POINT ( 'NONE',  ( -101.9981422329643408, -289.2790634579071138, -234.2348233834122198 ) ) ;
#68100 = CARTESIAN_POINT ( 'NONE',  ( 35.33833199506874934, -286.2788330938241756, -281.9733345030993519 ) ) ;
#68102 = CARTESIAN_POINT ( 'NONE',  ( -4.430195664870769434, -287.7010193353468139, -204.7565192107494738 ) ) ;
#68103 = CARTESIAN_POINT ( 'NONE',  ( -111.3304271840530646, -276.3943856895510294, -282.6358448095689369 ) ) ;
#68104 = CARTESIAN_POINT ( 'NONE',  ( -3.435204156061415492, -287.0119727073325748, -338.6162696419744407 ) ) ;
#68105 = CARTESIAN_POINT ( 'NONE',  ( -1.936776624305429628, -288.5212814234006942, -204.2438581886043210 ) ) ;
#68106 = CARTESIAN_POINT ( 'NONE',  ( 27.31350747876188834, -286.0636770670988085, -308.6982090815802167 ) ) ;
#68107 = CARTESIAN_POINT ( 'NONE',  ( 19.54236240378520861, -283.1441324987565054, -316.5069319659992289 ) ) ;
#68108 = CARTESIAN_POINT ( 'NONE',  ( -48.56938332891684951, -291.1948055548065213, -344.7371740285177566 ) ) ;
#68109 = DIRECTION ( 'NONE',  ( 0.000000000000000000, 0.000000000000000000, 1.000000000000000000 ) ) ;
#68110 = CARTESIAN_POINT ( 'NONE',  ( 154.4590814691992193, 20.78850955393007638, -13.92316269559726472 ) ) ;
#68111 = CARTESIAN_POINT ( 'NONE',  ( -112.6870074786758096, -298.5531716504414703, -264.0161821276322485 ) ) ;
#68112 = CARTESIAN_POINT ( 'NONE',  ( 13.24747034815653635, -280.3445444988888084, -325.7302111383315264 ) ) ;
#68113 = CARTESIAN_POINT ( 'NONE',  ( -42.03386674233713194, -291.1915918114947885, -193.6659917156558777 ) ) ;
#68114 = CARTESIAN_POINT ( 'NONE',  ( -104.4375144098692232, -295.3634876448812179, -239.5039730179465209 ) ) ;
#68115 = CARTESIAN_POINT ( 'NONE',  ( 17.44152136826783561, -279.5408207855496698, -221.3708932315629738 ) ) ;
#68116 = CARTESIAN_POINT ( 'NONE',  ( -66.35222538564052286, -271.7491693495936715, -201.8067335575473180 ) ) ;
#68117 = CARTESIAN_POINT ( 'NONE',  ( -100.5823470951192320, -297.3551008953662631, -307.9027602475997583 ) ) ;
#68118 =( NAMED_UNIT ( * ) SI_UNIT ( $, .STERADIAN. ) SOLID_ANGLE_UNIT ( ) );
#68119 = CARTESIAN_POINT ( 'NONE',  ( -37.23494835315388229, -296.5333528485438137, -194.0537167287832858 ) ) ;
#68120 = CARTESIAN_POINT ( 'NONE',  ( 21.48768313162443988, -292.4464461992631072, -318.4760026626552758 ) ) ;
#68121 = CARTESIAN_POINT ( 'NONE',  ( -3.380336603583590449, -293.9350932193924564, -205.0771175991985444 ) ) ;
#68122 = EDGE_CURVE ( 'NONE', #30954, #93112, #24409, .T. ) ;
#68123 = CYLINDRICAL_SURFACE ( 'NONE', #74754, 2.999999999999997335 ) ;
#68124 = CARTESIAN_POINT ( 'NONE',  ( 34.10528807209895064, -294.1469700896925019, -254.5574449005835049 ) ) ;
#68125 = AXIS2_PLACEMENT_3D ( 'NONE', #86529, #85615, #62938 ) ;
#68126 = CARTESIAN_POINT ( 'NONE',  ( 195.8725848201698341, 20.33787691583836121, 12.24547402278110475 ) ) ;
#68128 = CARTESIAN_POINT ( 'NONE',  ( -73.30240448022638589, -295.5433849891717841, -333.8892829371502557 ) ) ;
#68127 = CARTESIAN_POINT ( 'NONE',  ( -22.08418670521753313, -280.8777261988713008, -344.1555289087579581 ) ) ;
#68129 = CARTESIAN_POINT ( 'NONE',  ( 6.925008835452445943, -282.4682459897093736, -333.4299571026047602 ) ) ;
#68130 = CARTESIAN_POINT ( 'NONE',  ( -6.834608772088241579, -282.3695609618431490, -201.2194681513061028 ) ) ;
#68131 = AXIS2_PLACEMENT_3D ( 'NONE', #12004, #62702, #11538 ) ;
#68132 = CARTESIAN_POINT ( 'NONE',  ( -4.779032676873494978, -286.1361284858115823, -200.6085769527804530 ) ) ;
#68133 = CARTESIAN_POINT ( 'NONE',  ( -66.00622989085336201, -289.6760666325096167, -201.2214890212815419 ) ) ;
#68134 = EDGE_CURVE ( 'NONE', #45831, #63777, #57072, .T. ) ;
#68135 = DIRECTION ( 'NONE',  ( 0.000000000000000000, 0.000000000000000000, 1.000000000000000000 ) ) ;
#68136 = CARTESIAN_POINT ( 'NONE',  ( -4.480114855683805963, -281.1068724959789620, -339.2436382176995266 ) ) ;
#68137 = CARTESIAN_POINT ( 'NONE',  ( -38.92762112559048404, -287.9919465014788216, -347.0356076482782441 ) ) ;
#68138 = CARTESIAN_POINT ( 'NONE',  ( 221.8344101925596306, -43.55766379199612004, 22.50000000000000000 ) ) ;
#68139 = CARTESIAN_POINT ( 'NONE',  ( -42.42470478329951078, -296.7174574360030306, -343.9858657197873413 ) ) ;
#68140 = CARTESIAN_POINT ( 'NONE',  ( -5.513536827198955770, -278.0668759923802895, -339.8274718220787349 ) ) ;
#68142 = CARTESIAN_POINT ( 'NONE',  ( -104.4598356075898806, -278.6051343877720683, -241.5992790906739742 ) ) ;
#68141 = CARTESIAN_POINT ( 'NONE',  ( 37.85882738418492721, -291.6435903541458288, -275.9429713176689916 ) ) ;
#68143 = CARTESIAN_POINT ( 'NONE',  ( -11.15524869941154229, -292.5507348674066179, -197.8946551662417335 ) ) ;
#68144 = CARTESIAN_POINT ( 'NONE',  ( -112.4746515569167542, -282.5297587967270374, -278.3832004006295620 ) ) ;
#68145 = EDGE_CURVE ( 'NONE', #43024, #87978, #6702, .T. ) ;
#68146 = CARTESIAN_POINT ( 'NONE',  ( -81.35156202801275072, -279.6507961037555674, -331.0911163483391988 ) ) ;
#68147 = CARTESIAN_POINT ( 'NONE',  ( -42.41796037625191929, -294.1764873077721063, -343.4202723044344907 ) ) ;
#68148 = CARTESIAN_POINT ( 'NONE',  ( -107.4472716918866126, -270.9055020910105895, -243.1027146468452429 ) ) ;
#68149 = ORIENTED_EDGE ( 'NONE', *, *, #2808, .F. ) ;
#68150 = CARTESIAN_POINT ( 'NONE',  ( 197.1933712184921603, 24.89666632552609826, 12.64285714285712992 ) ) ;
#68151 = CARTESIAN_POINT ( 'NONE',  ( -35.65547483204182555, -294.5381148762191970, -343.4157022015315306 ) ) ;
#68152 = CARTESIAN_POINT ( 'NONE',  ( 175.2296996224750103, 249.5000000000000568, 0.000000000000000000 ) ) ;
#68153 = CARTESIAN_POINT ( 'NONE',  ( -82.13390479932374433, -287.1952119285918457, -326.4764044574609443 ) ) ;
#68154 = CARTESIAN_POINT ( 'NONE',  ( -78.06745106268971313, -296.5775661449000040, -205.2901304115516439 ) ) ;
#68155 = CARTESIAN_POINT ( 'NONE',  ( 2.470005846205419964, -287.8892437244465441, -205.0286885176707017 ) ) ;
#68156 = CARTESIAN_POINT ( 'NONE',  ( 23.50832415670129194, -287.9453286307909252, -310.7110436777061295 ) ) ;
#68157 = CARTESIAN_POINT ( 'NONE',  ( -110.8585195312119254, -279.9966025379366101, -276.1524647362191445 ) ) ;
#68158 = CARTESIAN_POINT ( 'NONE',  ( -99.30808309524991273, -298.8665981674900536, -229.7943730339071919 ) ) ;
#68159 = CARTESIAN_POINT ( 'NONE',  ( -71.11077110766973419, -278.3910264473072402, -205.1796293333489984 ) ) ;
#68160 = ORIENTED_EDGE ( 'NONE', *, *, #75186, .F. ) ;
#68161 = CARTESIAN_POINT ( 'NONE',  ( -73.26697940214680216, -297.2561194965205686, -202.2205851647523502 ) ) ;
#68162 = CARTESIAN_POINT ( 'NONE',  ( -19.75521800301713071, -294.2000285052232584, -197.9750500273278817 ) ) ;
#68163 = CARTESIAN_POINT ( 'NONE',  ( 35.92924609118153256, -294.8866867874316426, -249.3897366780731488 ) ) ;
#68164 = CARTESIAN_POINT ( 'NONE',  ( 175.2296996224749250, 275.0000000000000568, -24.99999999999999289 ) ) ;
#68165 = CARTESIAN_POINT ( 'NONE',  ( -104.1374862354397948, -290.8027716561011289, -300.1882116075222484 ) ) ;
#68166 = CARTESIAN_POINT ( 'NONE',  ( 156.8306017167579114, 275.6568570078858329, 16.89650703334504911 ) ) ;
#68167 = CARTESIAN_POINT ( 'NONE',  ( -16.93614702093297097, -290.4525111718118637, -197.3959284710996371 ) ) ;
#68168 = CARTESIAN_POINT ( 'NONE',  ( -71.67118871967464599, -297.2520938694800634, -205.8986914482326256 ) ) ;
#68169 = CARTESIAN_POINT ( 'NONE',  ( 154.1407330040854333, 128.0000000000000568, -13.42592592592592737 ) ) ;
#68170 = CARTESIAN_POINT ( 'NONE',  ( 73.43068321062709458, -134.2391364535880598, 0.000000000000000000 ) ) ;
#68171 = CARTESIAN_POINT ( 'NONE',  ( -111.9660414447004513, -292.2741067489715761, -254.3646712383266220 ) ) ;
#68172 = CARTESIAN_POINT ( 'NONE',  ( 25.18497378105907814, -295.4090924074130839, -220.4570493818173702 ) ) ;
#68173 = CARTESIAN_POINT ( 'NONE',  ( -35.92363991557247260, -288.0701400896182349, -195.5412173182348283 ) ) ;
#68174 = CARTESIAN_POINT ( 'NONE',  ( -10.81714863463806786, -272.3985159329216117, -200.3308781809405161 ) ) ;
#68175 = CARTESIAN_POINT ( 'NONE',  ( 5.995614212063472337, -276.5648012480422722, -209.7731193528359768 ) ) ;
#68176 = CARTESIAN_POINT ( 'NONE',  ( -65.85638376163679197, -289.7560601331077805, -201.5852350712984560 ) ) ;
#68177 = CARTESIAN_POINT ( 'NONE',  ( -92.41950375270855034, -279.6898567445617232, -322.4627236557338392 ) ) ;
#68178 =( BOUNDED_CURVE ( )  B_SPLINE_CURVE ( 3, ( #4380, #70667, #5796, #41271 ),
 .UNSPECIFIED., .F., .T. ) 
 B_SPLINE_CURVE_WITH_KNOTS ( ( 4, 4 ),
 ( 3.141592653589793116, 4.712388980384689674 ),
 .UNSPECIFIED. ) 
 CURVE ( )  GEOMETRIC_REPRESENTATION_ITEM ( )  RATIONAL_B_SPLINE_CURVE ( ( 1.000000000000000000, 0.8047378541243649375, 0.8047378541243649375, 1.000000000000000000 ) ) 
 REPRESENTATION_ITEM ( '' )  );
#68179 = ORIENTED_EDGE ( 'NONE', *, *, #34788, .T. ) ;
#68180 = CARTESIAN_POINT ( 'NONE',  ( -4.789213084710878476, -281.9602129049083032, -335.8151343286834276 ) ) ;
#68181 = CARTESIAN_POINT ( 'NONE',  ( -101.8295820842718200, -279.0839187408105886, -311.9646886768086915 ) ) ;
#68182 =( BOUNDED_SURFACE ( )  B_SPLINE_SURFACE ( 3, 2, ( 
 ( #4229, #11792, #47767 ),
 ( #26941, #41107, #33106 ),
 ( #26478, #39712, #54876 ),
 ( #62475, #10848, #75726 ),
 ( #77133, #76665, #3769 ),
 ( #40642, #90831, #12264 ),
 ( #91317, #32654, #69562 ),
 ( #82819, #40183, #70038 ),
 ( #25990, #4690, #90375 ),
 ( #18427, #61995, #19366 ),
 ( #33565, #25530, #55367 ),
 ( #84219, #76203, #11332 ),
 ( #48231, #34054, #69102 ),
 ( #5179, #62956, #91790 ),
 ( #55829, #53952, #83115 ),
 ( #88819, #25365, #75105 ),
 ( #74636, #54245, #37697 ),
 ( #32005, #60441, #9763 ),
 ( #66603, #44806, #60903 ),
 ( #38638, #89751, #53788 ),
 ( #81259, #31549, #23967 ),
 ( #73707, #24911, #82195 ),
 ( #74160, #2208, #46200 ),
 ( #9276, #10684, #39542 ),
 ( #67541, #61383, #45256 ),
 ( #3125, #52841, #89277 ),
 ( #10215, #53310, #1725 ),
 ( #81718, #90216, #16867 ),
 ( #16404, #8817, #45726 ),
 ( #82656, #2670, #24428 ),
 ( #46658, #75562, #17349 ),
 ( #17805, #68464, #30612 ),
 ( #39083, #59514, #38159 ),
 ( #67997, #3599, #32486 ) ),
 .UNSPECIFIED., .F., .F., .F. ) 
 B_SPLINE_SURFACE_WITH_KNOTS ( ( 4, 2, 2, 2, 2, 2, 2, 2, 2, 2, 2, 2, 2, 2, 2, 2, 4 ),
 ( 3, 3 ),
 ( 0.000000000000000000, 0.005866933686059443154, 0.008800400529089164731, 0.01026713395060402552, 0.01173386737211888631, 0.01760080105817832946, 0.01906753447969319198, 0.02053426790120805104, 0.02346773474423777261, 0.02933466843029721577, 0.03080140185181207482, 0.03226813527332693388, 0.03520160211635665892, 0.03813506895938638397, 0.03960180238090124649, 0.04106853580241610208, 0.04693546948847554523 ),
 ( 0.000000000000000000, 1.000000000000000000 ),
 .UNSPECIFIED. ) 
 GEOMETRIC_REPRESENTATION_ITEM ( )  RATIONAL_B_SPLINE_SURFACE ( (
 ( 1.000000000000000000, 0.7319951502423088785, 1.000000000000000000),
 ( 1.000000000000000000, 0.7319945071636718703, 1.000000000000000000),
 ( 1.000000000000000000, 0.7318569880056964294, 1.000000000000000000),
 ( 1.000000000000000000, 0.7314477122716916968, 1.000000000000000000),
 ( 1.000000000000000000, 0.7312773020566604165, 1.000000000000000000),
 ( 1.000000000000000000, 0.7309684991269558285, 1.000000000000000000),
 ( 1.000000000000000000, 0.7308564438270946928, 1.000000000000000000),
 ( 1.000000000000000000, 0.7306150055450980618, 1.000000000000000000),
 ( 1.000000000000000000, 0.7304861486422284944, 1.000000000000000000),
 ( 1.000000000000000000, 0.7298013683911470650, 1.000000000000000000),
 ( 1.000000000000000000, 0.7291253948077436320, 1.000000000000000000),
 ( 1.000000000000000000, 0.7281088291350222841, 1.000000000000000000),
 ( 1.000000000000000000, 0.7278968450267667700, 1.000000000000000000),
 ( 1.000000000000000000, 0.7274548661943022188, 1.000000000000000000),
 ( 1.000000000000000000, 0.7272241993259396242, 1.000000000000000000),
 ( 1.000000000000000000, 0.7265094949468547947, 1.000000000000000000),
 ( 1.000000000000000000, 0.7260037385991419123, 1.000000000000000000),
 ( 1.000000000000000000, 0.7243961799752839381, 1.000000000000000000),
 ( 1.000000000000000000, 0.7232051185136439964, 1.000000000000000000),
 ( 1.000000000000000000, 0.7215445644803780700, 1.000000000000000000),
 ( 1.000000000000000000, 0.7212028694993208866, 1.000000000000000000),
 ( 1.000000000000000000, 0.7205081462822442440, 1.000000000000000000),
 ( 1.000000000000000000, 0.7201546886187416563, 1.000000000000000000),
 ( 1.000000000000000000, 0.7190756474479115257, 1.000000000000000000),
 ( 1.000000000000000000, 0.7183314332535508662, 1.000000000000000000),
 ( 1.000000000000000000, 0.7167903837648086363, 1.000000000000000000),
 ( 1.000000000000000000, 0.7159935541304642825, 1.000000000000000000),
 ( 1.000000000000000000, 0.7147557110474020980, 1.000000000000000000),
 ( 1.000000000000000000, 0.7143359865066217784, 1.000000000000000000),
 ( 1.000000000000000000, 0.7134816549837853517, 1.000000000000000000),
 ( 1.000000000000000000, 0.7130464429203826615, 1.000000000000000000),
 ( 1.000000000000000000, 0.7108513879084432663, 1.000000000000000000),
 ( 1.000000000000000000, 0.7090209741736491766, 1.000000000000000000),
 ( 1.000000000000000000, 0.7071067811865441310, 1.000000000000000000) ) ) 
 REPRESENTATION_ITEM ( '' )  SURFACE ( )  );
#68183 = CARTESIAN_POINT ( 'NONE',  ( 39.01713346955680350, -280.2702631687407120, -264.2506966091918912 ) ) ;
#68184 = CARTESIAN_POINT ( 'NONE',  ( -23.25451841258840702, -108.0230548315861228, -359.5793218185942237 ) ) ;
#68185 = CARTESIAN_POINT ( 'NONE',  ( 34.98333684742553373, -276.8208671833418180, -296.2454659780066777 ) ) ;
#68186 = APPLICATION_PROTOCOL_DEFINITION ( 'draft international standard', 'automotive_design', 1998, #52342 ) ;
#68187 = CARTESIAN_POINT ( 'NONE',  ( -18.73791950962220909, -275.8074798397020118, -196.3024849677360066 ) ) ;
#68188 = CARTESIAN_POINT ( 'NONE',  ( -85.28047601435908120, -298.1948066931273615, -330.5268031993605859 ) ) ;
#68189 = ORIENTED_EDGE ( 'NONE', *, *, #38083, .F. ) ;
#68190 = ORIENTED_EDGE ( 'NONE', *, *, #40288, .T. ) ;
#68191 = DIRECTION ( 'NONE',  ( 0.000000000000000000, 0.000000000000000000, 1.000000000000000000 ) ) ;
#68192 = VECTOR ( 'NONE', #72592, 1000.000000000000000 ) ;
#68193 = CARTESIAN_POINT ( 'NONE',  ( -58.76639227940843568, -290.4154094221062223, -340.5226909414288343 ) ) ;
#68194 = CARTESIAN_POINT ( 'NONE',  ( -43.08307500583523364, -290.8838399972848947, -346.1305750769485030 ) ) ;
#68195 = CARTESIAN_POINT ( 'NONE',  ( -110.4390666189930243, -289.8899706868205044, -271.1782348167046734 ) ) ;
#68196 = CARTESIAN_POINT ( 'NONE',  ( -71.03362207790604543, -285.1270369143106791, -201.1918957886914541 ) ) ;
#68197 = CARTESIAN_POINT ( 'NONE',  ( 151.7489156927950376, 20.88249531811356263, -8.613363710899797354 ) ) ;
#68198 = CARTESIAN_POINT ( 'NONE',  ( 28.85978928636847485, -280.3905914401466362, -303.0930240330241645 ) ) ;
#68199 = CARTESIAN_POINT ( 'NONE',  ( 34.90863849092423976, -289.6337747367565498, -287.4126297407460697 ) ) ;
#68200 = CARTESIAN_POINT ( 'NONE',  ( -69.32744702836673412, -281.9607209728453654, -336.7649611624587465 ) ) ;
#68201 = CARTESIAN_POINT ( 'NONE',  ( -24.80864878983320665, -281.5305769905262423, -197.9445031696770343 ) ) ;
#68202 = CARTESIAN_POINT ( 'NONE',  ( 37.59787051185729467, -288.7028931890693002, -287.0609102581877323 ) ) ;
#68203 = CARTESIAN_POINT ( 'NONE',  ( -107.2878432503601687, -279.3237200250767387, -249.2536429075893523 ) ) ;
#68204 = ADVANCED_FACE ( 'NONE', ( #36198 ), #34338, .F. ) ;
#68205 = CARTESIAN_POINT ( 'NONE',  ( -82.63030655195812813, -288.4508128464818242, -332.1425945407843301 ) ) ;
#68206 = CARTESIAN_POINT ( 'NONE',  ( -113.9915834790967040, -285.4313054464715265, -264.2712388212321457 ) ) ;
#68207 = CARTESIAN_POINT ( 'NONE',  ( -29.47546774090680088, -286.6416090093147204, -193.8258366333480751 ) ) ;
#68208 = CARTESIAN_POINT ( 'NONE',  ( -106.1730206436254349, -284.3934411963727484, -294.8272514909809843 ) ) ;
#68209 = ORIENTED_EDGE ( 'NONE', *, *, #15663, .T. ) ;
#68210 = CARTESIAN_POINT ( 'NONE',  ( 175.2296996224750103, 249.5000000000000568, 25.00000000000000355 ) ) ;
#68211 = CARTESIAN_POINT ( 'NONE',  ( 25.45561829809514620, -294.8438349271464745, -227.8801642848519577 ) ) ;
#68212 = CARTESIAN_POINT ( 'NONE',  ( 6.318747573993888977, -293.1580178845388787, -333.2513205825137561 ) ) ;
#68213 = CARTESIAN_POINT ( 'NONE',  ( 30.49145158158179925, -274.9811050137151938, -298.1016518714695280 ) ) ;
#68214 = CARTESIAN_POINT ( 'NONE',  ( -27.76876061533236495, -294.2823461513569896, -346.7142190754476019 ) ) ;
#68215 = CARTESIAN_POINT ( 'NONE',  ( -108.4155023662685693, -289.2868959687370989, -250.8874848063960599 ) ) ;
#68216 = CARTESIAN_POINT ( 'NONE',  ( -15.31229921200150201, -293.0030087938605448, -341.0739173088455232 ) ) ;
#68217 = CARTESIAN_POINT ( 'NONE',  ( -37.56648963734183866, -293.2543901205146426, -196.9518768416542116 ) ) ;
#68218 = CARTESIAN_POINT ( 'NONE',  ( 201.0876323342543515, 25.81167821795958162, 10.49999999999999822 ) ) ;
#68219 = CARTESIAN_POINT ( 'NONE',  ( 37.77384621546699606, -291.5874995121845359, -273.1329623433663869 ) ) ;
#68220 = CARTESIAN_POINT ( 'NONE',  ( -87.40220017547704856, -297.7500733112210014, -326.2773113011045893 ) ) ;
#68221 = CARTESIAN_POINT ( 'NONE',  ( 28.44436102823925694, -288.9279034904681112, -302.5418980369116753 ) ) ;
#68222 = CARTESIAN_POINT ( 'NONE',  ( -2.211680179745054708, -278.5693669085690658, -337.0266150843143578 ) ) ;
#68223 = CARTESIAN_POINT ( 'NONE',  ( -108.2944544808214857, -276.9784784927340411, -299.2352477078088668 ) ) ;
#68224 = CARTESIAN_POINT ( 'NONE',  ( -44.02561982015154030, -273.3184745797630057, -193.7008442194582472 ) ) ;
#68225 = CARTESIAN_POINT ( 'NONE',  ( 3.514360123374058897, -278.6856735298910053, -208.0730814171312488 ) ) ;
#68226 = CARTESIAN_POINT ( 'NONE',  ( -28.71208679880496462, -275.3444723414158375, -346.1239116492341168 ) ) ;
#68227 = EDGE_CURVE ( 'NONE', #59201, #92631, #20278, .T. ) ;
#68228 = CARTESIAN_POINT ( 'NONE',  ( -84.80930274944560665, -294.4071799903408078, -326.5356153282622245 ) ) ;
#68229 = CARTESIAN_POINT ( 'NONE',  ( 145.2857639756989272, -299.5541904835127980, -195.3611179825600175 ) ) ;
#68230 = CARTESIAN_POINT ( 'NONE',  ( -40.53522992484867160, -298.8138391489502510, -197.2567971679214622 ) ) ;
#68231 = CARTESIAN_POINT ( 'NONE',  ( 196.0143093133015384, 24.42324672360810212, 11.99999999999998934 ) ) ;
#68233 = CARTESIAN_POINT ( 'NONE',  ( -1.720774803308078083, -274.3715100236110516, -206.6275005022664857 ) ) ;
#68232 = CARTESIAN_POINT ( 'NONE',  ( -59.56674070809860666, -287.3586909929717308, -342.3642732730834837 ) ) ;
#68234 = CARTESIAN_POINT ( 'NONE',  ( 23.28745962536372005, -288.1868200511356122, -317.8492315087341353 ) ) ;
#68235 = B_SPLINE_CURVE_WITH_KNOTS ( 'NONE', 3,
 ( #90674, #39092, #40485, #19215, #53797, #47129, #46667, #91150 ),
 .UNSPECIFIED., .F., .F.,
 ( 4, 2, 2, 4 ),
 ( 0.000000000000000000, 0.004220890787215657823, 0.006331336180823474158, 0.008441781574431289625 ),
 .UNSPECIFIED. ) ;
#68236 = CARTESIAN_POINT ( 'NONE',  ( -91.86041495851810623, -275.2768696531442743, -218.5954614916149126 ) ) ;
#68237 = CARTESIAN_POINT ( 'NONE',  ( -100.2889047179441349, -294.0045845158685438, -310.9243262591206758 ) ) ;
#68238 = CARTESIAN_POINT ( 'NONE',  ( -76.68402382037567122, -282.7614468443223359, -336.4253907082803039 ) ) ;
#68239 = CARTESIAN_POINT ( 'NONE',  ( 154.1407330040854333, 128.0000000000000568, -13.42592592592592737 ) ) ;
#68240 = CARTESIAN_POINT ( 'NONE',  ( -106.7874521163989243, -276.9229081003919646, -241.9013258546824261 ) ) ;
#68241 = DIRECTION ( 'NONE',  ( 0.000000000000000000, 0.000000000000000000, 1.000000000000000000 ) ) ;
#68242 = CARTESIAN_POINT ( 'NONE',  ( -69.17601360528942678, -290.4187796333781080, -204.2132330037402994 ) ) ;
#68243 = DIRECTION ( 'NONE',  ( 0.000000000000000000, 1.000000000000000000, 0.000000000000000000 ) ) ;
#68244 = CARTESIAN_POINT ( 'NONE',  ( 219.8344101925596021, 36.73669859915801794, 10.00000000000000000 ) ) ;
#68245 = CARTESIAN_POINT ( 'NONE',  ( -34.76370661218703617, -290.0843910714747267, -195.4054337353889252 ) ) ;
#68246 = CARTESIAN_POINT ( 'NONE',  ( -40.82692550182953539, -275.5277826960543166, -196.7000708261558373 ) ) ;
#68247 = CARTESIAN_POINT ( 'NONE',  ( 36.62601983310198506, -283.2191621828485495, -289.5283477820594840 ) ) ;
#68249 = CARTESIAN_POINT ( 'NONE',  ( -33.49622495927432198, -283.0024352086145427, -343.2723347003428671 ) ) ;
#68248 = CARTESIAN_POINT ( 'NONE',  ( -79.67961082692174557, -295.5035787369413924, -207.9613405089926346 ) ) ;
#68250 = CARTESIAN_POINT ( 'NONE',  ( -32.67162431688959146, -275.5374047398941570, -196.9075937844483235 ) ) ;
#68251 = CARTESIAN_POINT ( 'NONE',  ( -35.39625786534305263, -274.8799912201071152, -197.2129780881582519 ) ) ;
#68252 = EDGE_CURVE ( 'NONE', #46969, #44141, #12179, .T. ) ;
#68253 = CARTESIAN_POINT ( 'NONE',  ( -24.84118108081210607, -284.8929889110902423, -344.3647450824703924 ) ) ;
#68254 = EDGE_LOOP ( 'NONE', ( #6856, #45084, #69244, #47670 ) ) ;
#68255 = CARTESIAN_POINT ( 'NONE',  ( 203.2380858836131097, 291.9636489450776367, -53.99999999997883293 ) ) ;
#68256 = CARTESIAN_POINT ( 'NONE',  ( 8.904463510063092002, -294.2704878251129799, -331.9264682474528740 ) ) ;
#68257 = VECTOR ( 'NONE', #79481, 1000.000000000000000 ) ;
#68258 = EDGE_CURVE ( 'NONE', #44986, #74736, #2156, .T. ) ;
#68259 = DIRECTION ( 'NONE',  ( 0.000000000000000000, 0.000000000000000000, -1.000000000000000000 ) ) ;
#68260 = CARTESIAN_POINT ( 'NONE',  ( 36.57525178469694538, -285.4809262143061801, -305.9938812882205070 ) ) ;
#68261 = CARTESIAN_POINT ( 'NONE',  ( -113.0756011663440006, -277.9120231582376164, -257.3790128287753873 ) ) ;
#68262 = CARTESIAN_POINT ( 'NONE',  ( -71.79216514076699696, -290.0044462979988680, -202.3789893732148073 ) ) ;
#68263 = CARTESIAN_POINT ( 'NONE',  ( -109.8788954254723507, -286.2431167119542579, -257.2876007725129739 ) ) ;
#68264 = CARTESIAN_POINT ( 'NONE',  ( -64.68696564924297832, -279.1741722590903692, -339.1920628701112719 ) ) ;
#68265 = CARTESIAN_POINT ( 'NONE',  ( -30.95136032721581643, -287.5566518426239782, -194.2048369856267129 ) ) ;
#68266 = CARTESIAN_POINT ( 'NONE',  ( 29.95665205232298334, -283.9903010137520027, -303.5839280930067048 ) ) ;
#68267 = CARTESIAN_POINT ( 'NONE',  ( -1.465847451629220144, -276.7564478725773256, -338.4927787524290466 ) ) ;
#68268 = CARTESIAN_POINT ( 'NONE',  ( -108.6572321136195569, -278.0167069861469145, -299.3972145195943426 ) ) ;
#68269 = CARTESIAN_POINT ( 'NONE',  ( -109.5781508691519690, -298.7055692796266158, -252.3308367490608077 ) ) ;
#68270 = DIRECTION ( 'NONE',  ( 0.000000000000000000, 0.000000000000000000, 1.000000000000000000 ) ) ;
#68271 = DIRECTION ( 'NONE',  ( 0.000000000000000000, 1.000000000000000000, 0.000000000000000000 ) ) ;
#68272 = CARTESIAN_POINT ( 'NONE',  ( -30.59740699726062019, -296.2753177241256139, -194.5984209097469204 ) ) ;
#68273 = DIRECTION ( 'NONE',  ( -0.000000000000000000, -0.000000000000000000, 1.000000000000000000 ) ) ;
#68274 = CARTESIAN_POINT ( 'NONE',  ( -103.1891897845255386, -277.6304879278584963, -302.1341105276584358 ) ) ;
#68275 = CARTESIAN_POINT ( 'NONE',  ( -64.77230194073887048, -274.9068642136576841, -198.8237855755641590 ) ) ;
#68276 = CARTESIAN_POINT ( 'NONE',  ( 37.31671867858363356, -280.8355964471062407, -288.2760612169074079 ) ) ;
#68277 = CARTESIAN_POINT ( 'NONE',  ( -27.72680229456249634, -287.9360790159931298, -196.9749629409670035 ) ) ;
#68278 = CARTESIAN_POINT ( 'NONE',  ( -69.22046592836221635, -296.9840475676032270, -339.7039994193829671 ) ) ;
#68279 = CARTESIAN_POINT ( 'NONE',  ( -99.67640017537755170, -297.1633500057298534, -314.9745205380372681 ) ) ;
#68280 = CARTESIAN_POINT ( 'NONE',  ( -4.039535456207898889, -294.4924206869389423, -203.3319647022740924 ) ) ;
#68281 = CARTESIAN_POINT ( 'NONE',  ( -27.28745629830472907, -278.1799192287834330, -196.1537974063413401 ) ) ;
#68282 = CARTESIAN_POINT ( 'NONE',  ( 31.34089874792687880, -283.0946764400395068, -241.6554598822298772 ) ) ;
#68283 = CARTESIAN_POINT ( 'NONE',  ( -110.7425282997226077, -270.7508960706601897, -256.5143776799616262 ) ) ;
#68284 = CARTESIAN_POINT ( 'NONE',  ( -78.70816290299524098, -285.1996186883256996, -334.3553065605329380 ) ) ;
#68285 = CARTESIAN_POINT ( 'NONE',  ( 34.58477660331920589, -286.6594758771205420, -284.5966240585956371 ) ) ;
#68286 = CARTESIAN_POINT ( 'NONE',  ( 30.98277457338434004, -281.3561911198370353, -305.6467941564162629 ) ) ;
#68287 = CARTESIAN_POINT ( 'NONE',  ( -11.11022278200930558, -92.70253263746865002, -359.4537332136167151 ) ) ;
#68288 = ORIENTED_EDGE ( 'NONE', *, *, #26658, .T. ) ;
#68289 = CARTESIAN_POINT ( 'NONE',  ( -27.82959668005257470, -285.8429938832449011, -197.9621720322206500 ) ) ;
#68290 = VERTEX_POINT ( 'NONE', #77904 ) ;
#68291 = CARTESIAN_POINT ( 'NONE',  ( -109.0091602172492742, -285.2831866890015249, -297.8086170479778616 ) ) ;
#68292 = CARTESIAN_POINT ( 'NONE',  ( 35.39887449299214950, -275.7938246196474097, -263.4145137880428820 ) ) ;
#68293 = CARTESIAN_POINT ( 'NONE',  ( 2.547410411992344415, -285.3694003799847110, -204.9633536586277103 ) ) ;
#68294 = CARTESIAN_POINT ( 'NONE',  ( -86.30506999379602462, -290.3115942056789436, -211.2660713682429332 ) ) ;
#68295 = CARTESIAN_POINT ( 'NONE',  ( 31.80429870901055978, -282.0629695675908692, -236.8974348519450075 ) ) ;
#68296 = CARTESIAN_POINT ( 'NONE',  ( 140.6539576904058606, 250.5000000000000568, 12.50000000000000000 ) ) ;
#68297 = CARTESIAN_POINT ( 'NONE',  ( -50.83620284106032017, -281.4028644689976204, -195.2571490623167278 ) ) ;
#68298 = CARTESIAN_POINT ( 'NONE',  ( 37.17240806842435319, -282.1273476364965518, -289.6844709857626867 ) ) ;
#68299 = CARTESIAN_POINT ( 'NONE',  ( -53.35057174420112602, -280.7666405000205145, -340.3538533559490702 ) ) ;
#68300 = CARTESIAN_POINT ( 'NONE',  ( -89.44128332668068992, -230.9695510001336061, -347.9586317399256927 ) ) ;
#68301 = ORIENTED_EDGE ( 'NONE', *, *, #59476, .F. ) ;
#68302 = CARTESIAN_POINT ( 'NONE',  ( 36.52081155437959126, -277.7109644354906663, -282.6897660608909746 ) ) ;
#68303 = CARTESIAN_POINT ( 'NONE',  ( 202.4137727338654145, 295.8836245966012939, -68.61462046017487637 ) ) ;
#68304 = CARTESIAN_POINT ( 'NONE',  ( 35.24378545467292412, -279.7976016100379866, -287.8278912963958760 ) ) ;
#68305 = CARTESIAN_POINT ( 'NONE',  ( -84.13372638231025746, -296.7377939835836855, -214.1309973625218959 ) ) ;
#68306 = CARTESIAN_POINT ( 'NONE',  ( -8.528442555772940636, -291.9269967620080024, -199.0216261750705939 ) ) ;
#68307 = CARTESIAN_POINT ( 'NONE',  ( -113.5000000000000568, -218.8335761803644743, -490.8867980474134356 ) ) ;
#68309 = CARTESIAN_POINT ( 'NONE',  ( 17.49860077288287741, -285.2524054886260387, -220.9561968347129550 ) ) ;
#68308 = CARTESIAN_POINT ( 'NONE',  ( -111.9585833985336905, -271.4497082950938989, -253.4608515288946364 ) ) ;
#68310 = CARTESIAN_POINT ( 'NONE',  ( 31.97340496418030042, -295.0635297477839458, -243.7851573310300068 ) ) ;
#68311 = CARTESIAN_POINT ( 'NONE',  ( -27.78892319592413074, -287.4911834976902583, -197.4914539913472709 ) ) ;
#68312 = VERTEX_POINT ( 'NONE', #7320 ) ;
#68313 = CARTESIAN_POINT ( 'NONE',  ( -7.293385877938820983, -293.3779557772207909, -199.7074822970287471 ) ) ;
#68314 = CARTESIAN_POINT ( 'NONE',  ( -86.96604037179409374, -284.2574985429677668, -324.0532075999353765 ) ) ;
#68315 = CARTESIAN_POINT ( 'NONE',  ( 98.32702654663349051, -298.5100415232777209, -193.7851615946195523 ) ) ;
#68316 = CARTESIAN_POINT ( 'NONE',  ( -103.6538913608810901, -290.8474934253744664, -309.2845285084534339 ) ) ;
#68317 = CARTESIAN_POINT ( 'NONE',  ( -39.21648186493953148, -292.5215923412303596, -193.4324765471042724 ) ) ;
#68318 = CARTESIAN_POINT ( 'NONE',  ( -97.34769812036847725, -290.1393520099832699, -311.9556679138568143 ) ) ;
#68319 = ORIENTED_EDGE ( 'NONE', *, *, #88201, .F. ) ;
#68320 = CARTESIAN_POINT ( 'NONE',  ( 157.1544330182169631, 16.98551211945807893, 7.440913067426849992 ) ) ;
#68321 = CARTESIAN_POINT ( 'NONE',  ( -97.27173917898515754, -299.0416701196417080, -223.9861427894485928 ) ) ;
#68322 = CARTESIAN_POINT ( 'NONE',  ( -31.27612358005698567, -272.9220556158824138, -193.9854961107881763 ) ) ;
#68323 = EDGE_CURVE ( 'NONE', #72504, #20412, #70342, .T. ) ;
#68324 = CARTESIAN_POINT ( 'NONE',  ( 35.26769376072147111, -280.4802999492753202, -260.4293321346249854 ) ) ;
#68325 = VERTEX_POINT ( 'NONE', #41884 ) ;
#68326 = EDGE_LOOP ( 'NONE', ( #85632, #5173, #1936, #82606 ) ) ;
#68327 = CARTESIAN_POINT ( 'NONE',  ( 1.170053370301559426, -274.0596261781940939, -203.7397505483738200 ) ) ;
#68328 = CARTESIAN_POINT ( 'NONE',  ( -50.05467972473267224, -296.3668478065745262, -197.7726347324097844 ) ) ;
#68329 = CARTESIAN_POINT ( 'NONE',  ( -46.02953020763133196, -279.0237719941371779, -344.1376773496667738 ) ) ;
#68330 = CARTESIAN_POINT ( 'NONE',  ( 35.33540859630638664, -273.4946662308361738, -255.1694151051649442 ) ) ;
#68331 = AXIS2_PLACEMENT_3D ( 'NONE', #64299, #6500, #71846 ) ;
#68332 = CARTESIAN_POINT ( 'NONE',  ( -70.66144693004908106, -298.8076802801734857, -204.9489263732471045 ) ) ;
#68333 = CARTESIAN_POINT ( 'NONE',  ( -110.5496402674577752, -297.5812541623145080, -274.2112573753506695 ) ) ;
#68334 = CARTESIAN_POINT ( 'NONE',  ( -113.4336187099429338, -298.0897629919161318, -275.3079574863053267 ) ) ;
#68335 = CARTESIAN_POINT ( 'NONE',  ( -41.08527851115144358, -272.0255016400885211, -195.0478156383719579 ) ) ;
#68336 = CARTESIAN_POINT ( 'NONE',  ( 32.85037379755767262, -294.4738350036436714, -290.8258589516847223 ) ) ;
#68337 = CARTESIAN_POINT ( 'NONE',  ( 31.38511609544448433, -291.7783707396216641, -244.0552317994517750 ) ) ;
#68338 = CARTESIAN_POINT ( 'NONE',  ( 193.9402003287077605, 214.5000000000000568, 16.58062614384823874 ) ) ;
#68339 = CARTESIAN_POINT ( 'NONE',  ( 38.43040694093095055, -275.8765122366463629, -256.9399099676472247 ) ) ;
#68340 = CARTESIAN_POINT ( 'NONE',  ( -63.30870623302911326, -273.8708978526993860, -202.1221554521191592 ) ) ;
#68341 = CARTESIAN_POINT ( 'NONE',  ( -83.59844996041638865, -282.3562785599247036, -331.3670858172334306 ) ) ;
#68342 = DIRECTION ( 'NONE',  ( -0.000000000000000000, -1.000000000000000000, -0.000000000000000000 ) ) ;
#68343 = CARTESIAN_POINT ( 'NONE',  ( -109.0853113604347300, -283.9379855821192109, -256.0273824345195521 ) ) ;
#68344 = CARTESIAN_POINT ( 'NONE',  ( -91.13980850780355070, -281.8143853667122585, -322.8567555219859742 ) ) ;
#68345 = EDGE_CURVE ( 'NONE', #92829, #33827, #70795, .T. ) ;
#68346 = CARTESIAN_POINT ( 'NONE',  ( 19.62630006753686374, -274.7814137089202973, -316.9644618080894247 ) ) ;
#68347 = CARTESIAN_POINT ( 'NONE',  ( -10.45842673334823303, -282.4029203368400545, -200.2900439322175430 ) ) ;
#68348 = CYLINDRICAL_SURFACE ( 'NONE', #50412, 1.500000000000001332 ) ;
#68349 = CARTESIAN_POINT ( 'NONE',  ( -55.12692399563955092, -272.2269772601271711, -196.2657319900211519 ) ) ;
#68350 = CARTESIAN_POINT ( 'NONE',  ( -109.6693238589066510, -280.2895844533979357, -290.8243355635115108 ) ) ;
#68351 = CARTESIAN_POINT ( 'NONE',  ( 123.4306832106270946, -134.2391364535880882, 0.000000000000000000 ) ) ;
#68352 = CARTESIAN_POINT ( 'NONE',  ( -104.1701412615792037, -286.9375009851185041, -234.9889348342551898 ) ) ;
#68353 = CARTESIAN_POINT ( 'NONE',  ( 156.4851178187871312, 15.00000000000000178, -10.00000000000000000 ) ) ;
#68354 = CARTESIAN_POINT ( 'NONE',  ( -73.78304147019487402, -287.5357767546639138, -335.9273842735322546 ) ) ;
#68355 = CARTESIAN_POINT ( 'NONE',  ( -48.18343439339133027, -253.0206516614774728, -472.6442049081569508 ) ) ;
#68356 = CARTESIAN_POINT ( 'NONE',  ( -93.03574360256133957, -296.0241336871748672, -222.5369376958423402 ) ) ;
#68357 = CARTESIAN_POINT ( 'NONE',  ( -31.80243948563547107, -287.1212288633412300, -344.4408493656098926 ) ) ;
#68358 = CARTESIAN_POINT ( 'NONE',  ( -35.93751134800100289, -122.5594593288581251, -363.2174194532766478 ) ) ;
#68359 = CARTESIAN_POINT ( 'NONE',  ( -111.0053523957496537, -294.7338470623768103, -256.1979106822892049 ) ) ;
#68360 = CARTESIAN_POINT ( 'NONE',  ( -106.0463765469124695, -283.4619170499775009, -237.1590820651039735 ) ) ;
#68361 = CARTESIAN_POINT ( 'NONE',  ( -5.228600245311270989, -282.0821595823695134, -203.9142276586865989 ) ) ;
#68362 = CARTESIAN_POINT ( 'NONE',  ( 1.555906525634688453, -280.7795316778975234, -335.6370722843251428 ) ) ;
#68363 = CARTESIAN_POINT ( 'NONE',  ( -92.41172517849986434, -289.8682286249937761, -318.3563034840150863 ) ) ;
#68364 = CARTESIAN_POINT ( 'NONE',  ( 24.63642525851434684, -283.5229760691759111, -310.1295930600817314 ) ) ;
#68365 = CARTESIAN_POINT ( 'NONE',  ( -33.47749448940577821, -283.8051381041314585, -343.4330752799006632 ) ) ;
#68366 = ADVANCED_FACE ( 'NONE', ( #27707 ), #80674, .T. ) ;
#68367 = CARTESIAN_POINT ( 'NONE',  ( 19.03897906200381840, -288.8392426917267812, -220.2878646290233746 ) ) ;
#68368 = CARTESIAN_POINT ( 'NONE',  ( -31.91166361358936143, -298.2850575700418290, -193.3609690682164057 ) ) ;
#68369 = ORIENTED_EDGE ( 'NONE', *, *, #67853, .T. ) ;
#68370 = CARTESIAN_POINT ( 'NONE',  ( -71.40280104847005305, -273.6147269303191933, -201.3043195910106249 ) ) ;
#68371 = CARTESIAN_POINT ( 'NONE',  ( -2.899238311503552712, -294.4896234450193333, -204.1375298169641326 ) ) ;
#68372 = DIRECTION ( 'NONE',  ( -0.000000000000000000, -1.000000000000000000, -0.000000000000000000 ) ) ;
#68373 = CARTESIAN_POINT ( 'NONE',  ( -37.37352853689063892, -288.5519495502701943, -195.3611179825600175 ) ) ;
#68374 = ORIENTED_EDGE ( 'NONE', *, *, #8991, .F. ) ;
#68375 = CARTESIAN_POINT ( 'NONE',  ( 37.31354789722783494, -273.6697087536383606, -279.5496824014452386 ) ) ;
#68376 = CARTESIAN_POINT ( 'NONE',  ( -113.5000000000000568, -296.0521521680024080, -400.5374811273811702 ) ) ;
#68377 = CARTESIAN_POINT ( 'NONE',  ( -113.5090896857543470, -294.9976274434279730, -266.7526290622055853 ) ) ;
#68378 = CARTESIAN_POINT ( 'NONE',  ( -1.665644115893663457, -273.8868551248680205, -206.5415199493936882 ) ) ;
#68379 = CARTESIAN_POINT ( 'NONE',  ( -79.94718285793359769, -292.9845490272139727, -210.1696928222670522 ) ) ;
#68380 = CARTESIAN_POINT ( 'NONE',  ( -61.84940986627871240, -285.1351080055624720, -340.2530856550145018 ) ) ;
#68381 = CARTESIAN_POINT ( 'NONE',  ( -112.5500953213806810, -291.8063263903147799, -283.9369107372662597 ) ) ;
#68382 = CARTESIAN_POINT ( 'NONE',  ( -102.8026306123124840, -292.3886370004836976, -230.6588780488229986 ) ) ;
#68383 = CARTESIAN_POINT ( 'NONE',  ( -34.30331926453491320, -294.8462094232859840, -343.2978593839272889 ) ) ;
#68384 = CARTESIAN_POINT ( 'NONE',  ( 30.61158399337896441, -289.1351492818308770, -238.6223117233984397 ) ) ;
#68385 = CARTESIAN_POINT ( 'NONE',  ( 23.74600930128720222, -281.0933142952720800, -223.4643003413286522 ) ) ;
#68386 = CARTESIAN_POINT ( 'NONE',  ( -100.4395098995483835, -294.0739341297344254, -312.0247741560880286 ) ) ;
#68387 = CARTESIAN_POINT ( 'NONE',  ( -10.70402646358210497, -282.5476109601004850, -342.6634163795613404 ) ) ;
#68388 = CARTESIAN_POINT ( 'NONE',  ( -5.553785854370113739, -278.6118679223745289, -337.9131540086680729 ) ) ;
#68389 = EDGE_CURVE ( 'NONE', #4490, #63422, #11200, .T. ) ;
#68390 = CARTESIAN_POINT ( 'NONE',  ( -35.76141371055521034, -275.1721490433179724, -346.1223526039944431 ) ) ;
#68392 = AXIS2_PLACEMENT_3D ( 'NONE', #86841, #36655, #690 ) ;
#68391 = DIRECTION ( 'NONE',  ( -1.000000000000000000, -0.000000000000000000, -0.000000000000000000 ) ) ;
#68393 = CARTESIAN_POINT ( 'NONE',  ( -3.598530781493743280, -282.1018834281535987, -335.1778115412341776 ) ) ;
#68394 = VECTOR ( 'NONE', #38248, 1000.000000000000000 ) ;
#68395 = CARTESIAN_POINT ( 'NONE',  ( -69.80812268687949995, -280.8391996572095763, -200.9642382458584109 ) ) ;
#68396 = CARTESIAN_POINT ( 'NONE',  ( 34.63777792396833632, -286.2725735048651359, -243.6820072050919066 ) ) ;
#68397 = CARTESIAN_POINT ( 'NONE',  ( 27.10605077755610282, -294.8197083538659058, -233.8633771306119797 ) ) ;
#68398 = CARTESIAN_POINT ( 'NONE',  ( 23.73873534974671173, -277.7646669189965678, -315.9200997434085707 ) ) ;
#68399 = AXIS2_PLACEMENT_3D ( 'NONE', #41797, #84879, #6779 ) ;
#68400 = CARTESIAN_POINT ( 'NONE',  ( 30.11620404028058218, -277.3380741327698615, -306.5663667808615855 ) ) ;
#68401 = CARTESIAN_POINT ( 'NONE',  ( -83.00841149244826056, -277.5303596797073737, -327.3783635016786207 ) ) ;
#68402 = CARTESIAN_POINT ( 'NONE',  ( -85.26803842849682269, -299.3889410165205049, -212.8208872898309778 ) ) ;
#68403 = CARTESIAN_POINT ( 'NONE',  ( 8.058917278216032543, -284.6737996454291419, -210.8077113090986359 ) ) ;
#68404 = CIRCLE ( 'NONE', #59280, 24.00000000000000000 ) ;
#68405 = CARTESIAN_POINT ( 'NONE',  ( 23.15242131724019004, -293.8558825388064975, -317.9869452891306878 ) ) ;
#68406 = CARTESIAN_POINT ( 'NONE',  ( -67.71606923919844689, -291.0442730697384945, -340.2455806194385559 ) ) ;
#68407 = CARTESIAN_POINT ( 'NONE',  ( -9.597799629979137492, -291.3435645212375675, -202.4506187485807800 ) ) ;
#68408 = EDGE_LOOP ( 'NONE', ( #9462, #64510, #82246, #53410 ) ) ;
#68409 = CARTESIAN_POINT ( 'NONE',  ( -70.62453610134701876, -290.1965488427768491, -201.5798768970310277 ) ) ;
#68410 = CARTESIAN_POINT ( 'NONE',  ( 18.49549683846597503, -292.5505262355009677, -223.3048227419540410 ) ) ;
#68411 = ORIENTED_EDGE ( 'NONE', *, *, #24610, .T. ) ;
#68412 = CARTESIAN_POINT ( 'NONE',  ( -74.26637465608381206, -290.6108195064770143, -337.5926324791993238 ) ) ;
#68413 = CARTESIAN_POINT ( 'NONE',  ( -102.2502051271011112, -279.6615629961774516, -236.6238740934600173 ) ) ;
#68414 = CARTESIAN_POINT ( 'NONE',  ( -65.41599023963952675, -296.6140840750867937, -198.9368152003324042 ) ) ;
#68415 = CARTESIAN_POINT ( 'NONE',  ( -3.541653042610806601, -287.1379948536681468, -201.2751283789181684 ) ) ;
#68416 = CARTESIAN_POINT ( 'NONE',  ( 36.66971422386825452, -287.6178714900088949, -249.0045766847676134 ) ) ;
#68417 = CARTESIAN_POINT ( 'NONE',  ( -107.0047570717433416, -284.5953885792574738, -292.2505214474406330 ) ) ;
#68418 = CARTESIAN_POINT ( 'NONE',  ( -56.60324186021520632, -169.1846951020332028, -364.3055494911789083 ) ) ;
#68419 = CARTESIAN_POINT ( 'NONE',  ( -49.43407259941375997, -154.1845681105646690, -363.5609398828140115 ) ) ;
#68420 = CARTESIAN_POINT ( 'NONE',  ( 64.45001422827949966, 46.57074262894973771, -315.3000494332260359 ) ) ;
#68421 = CARTESIAN_POINT ( 'NONE',  ( -95.40740334110685694, -277.1245358482831875, -314.8692727168392480 ) ) ;
#68422 = CARTESIAN_POINT ( 'NONE',  ( 13.93776827101168614, -275.2326265235146252, -322.8211349177072975 ) ) ;
#68423 = CARTESIAN_POINT ( 'NONE',  ( -46.11662604878426919, -297.4513314995372752, -193.9246896369507738 ) ) ;
#68424 = CARTESIAN_POINT ( 'NONE',  ( 26.83260473079646502, -24.62933982865472871, -342.1012798676335933 ) ) ;
#68425 = CARTESIAN_POINT ( 'NONE',  ( -86.78931057167142171, -276.4077431730805756, -328.8105140398925528 ) ) ;
#68426 = CARTESIAN_POINT ( 'NONE',  ( -64.96754881973922124, -275.4464210113846434, -201.6831460444351762 ) ) ;
#68427 = CARTESIAN_POINT ( 'NONE',  ( -84.72017325600741344, -290.2179862707740767, -326.0450523073967588 ) ) ;
#68428 = CARTESIAN_POINT ( 'NONE',  ( 53.34045889417781439, -299.9632562302277847, -193.5105485799727489 ) ) ;
#68429 = CARTESIAN_POINT ( 'NONE',  ( -101.5018370342409355, -297.6037442819738317, -227.8753335946865093 ) ) ;
#68430 = CARTESIAN_POINT ( 'NONE',  ( -4.334760257134855799, -294.7712040644221361, -335.4868812224659109 ) ) ;
#68431 = ORIENTED_EDGE ( 'NONE', *, *, #21626, .F. ) ;
#68432 = CARTESIAN_POINT ( 'NONE',  ( -74.60437101017137707, -279.4641283677482306, -336.0939678938331099 ) ) ;
#68433 = CARTESIAN_POINT ( 'NONE',  ( -35.90663495134732841, -282.5422953164523960, -347.2993016609133292 ) ) ;
#68434 = CARTESIAN_POINT ( 'NONE',  ( -66.88662933562555679, -278.3903727189822348, -337.3723529123301432 ) ) ;
#68435 = CARTESIAN_POINT ( 'NONE',  ( 35.91476065463498912, -277.5690847940529693, -290.5954492241596654 ) ) ;
#68436 = CARTESIAN_POINT ( 'NONE',  ( -36.45646440760401674, -296.6381726008356168, -196.7721045031088067 ) ) ;
#68437 = CYLINDRICAL_SURFACE ( 'NONE', #75952, 4.000000000000003553 ) ;
#68438 = CARTESIAN_POINT ( 'NONE',  ( -74.01144054981590159, -277.7207229415566303, -333.4826685173074452 ) ) ;
#68439 = CARTESIAN_POINT ( 'NONE',  ( -64.85183790945018245, -274.5046859558662504, -198.6019186033956885 ) ) ;
#68440 = CARTESIAN_POINT ( 'NONE',  ( -7.130177354123384603, -287.3488695339653418, -340.6643978980135330 ) ) ;
#68441 = CARTESIAN_POINT ( 'NONE',  ( -35.59653940537977945, -276.0741778120893173, -195.3686308519964143 ) ) ;
#68442 = CARTESIAN_POINT ( 'NONE',  ( 3.173569438467552573, -275.0943706692889918, -335.2085705235602973 ) ) ;
#68443 = CARTESIAN_POINT ( 'NONE',  ( 197.2116943569230898, 214.9331615741067765, -12.42446933126075592 ) ) ;
#68444 = CARTESIAN_POINT ( 'NONE',  ( -13.24431162253579686, -287.9281277036228062, -339.4401856805684474 ) ) ;
#68445 = CARTESIAN_POINT ( 'NONE',  ( -111.7783908071708083, -283.6582752681582633, -289.7133926939125672 ) ) ;
#68446 = CARTESIAN_POINT ( 'NONE',  ( 35.47847237912510820, -279.9651470506128703, -283.6681983543881529 ) ) ;
#68448 = CARTESIAN_POINT ( 'NONE',  ( -111.6643547565761878, -282.6968924718063363, -265.3442634026137625 ) ) ;
#68447 = CARTESIAN_POINT ( 'NONE',  ( 31.62885886734168750, -279.7856446449549708, -244.5548020066396475 ) ) ;
#68449 = CARTESIAN_POINT ( 'NONE',  ( 21.13005604134814419, -290.1987140432833030, -317.3498309153775381 ) ) ;
#68450 = CARTESIAN_POINT ( 'NONE',  ( -105.8906099957172131, -280.1073635266718043, -243.9855501237966848 ) ) ;
#68451 = FACE_BOUND ( 'NONE', #43288, .T. ) ;
#68452 = AXIS2_PLACEMENT_3D ( 'NONE', #7782, #50411, #78832 ) ;
#68453 = CARTESIAN_POINT ( 'NONE',  ( 30.02419410728393601, -279.4860640992655476, -234.6356978869577574 ) ) ;
#68454 = CARTESIAN_POINT ( 'NONE',  ( 18.86257163776771861, -294.8616755083610315, -220.6820767023252188 ) ) ;
#68455 = CARTESIAN_POINT ( 'NONE',  ( -88.23590778428064141, -277.5907254898050951, -213.9363571171152216 ) ) ;
#68456 = AXIS2_PLACEMENT_3D ( 'NONE', #47207, #39628, #54790 ) ;
#68457 = CARTESIAN_POINT ( 'NONE',  ( -1.412905491629123267, -277.2140329782872641, -334.0816913708131324 ) ) ;
#68458 = CARTESIAN_POINT ( 'NONE',  ( -95.73174578151045466, -285.9016969049153545, -317.7166410043448082 ) ) ;
#68459 = DIRECTION ( 'NONE',  ( 0.000000000000000000, 0.000000000000000000, -1.000000000000000000 ) ) ;
#68460 = CARTESIAN_POINT ( 'NONE',  ( -86.43000992025280027, -291.6472956920073898, -327.8724194175006801 ) ) ;
#68461 = AXIS2_PLACEMENT_3D ( 'NONE', #40571, #34443, #90757 ) ;
#68462 = CARTESIAN_POINT ( 'NONE',  ( 0.2138159796696542936, -285.7362339578068031, -203.3107220206265424 ) ) ;
#68463 = CARTESIAN_POINT ( 'NONE',  ( -47.08007906786437502, -290.3262565216114126, -197.2064572312184225 ) ) ;
#68464 = CARTESIAN_POINT ( 'NONE',  ( -48.18343439343948376, -278.5213373408708435, -430.9214249866280397 ) ) ;
#68465 = CARTESIAN_POINT ( 'NONE',  ( 31.71946125282903850, -274.5713978015491534, -295.6445288702159928 ) ) ;
#68466 = CARTESIAN_POINT ( 'NONE',  ( 8.980753267418275954, -292.5487825161296200, -328.4366111618166428 ) ) ;
#68467 = FILL_AREA_STYLE_COLOUR ( '', #4929 ) ;
#68468 = DIRECTION ( 'NONE',  ( 0.000000000000000000, -1.000000000000000000, 0.000000000000000000 ) ) ;
#68469 = CARTESIAN_POINT ( 'NONE',  ( -11.37085642590842305, -290.8642047948958975, -198.5544600203934920 ) ) ;
#68470 = CARTESIAN_POINT ( 'NONE',  ( -111.1176266111509960, -286.1087937281242830, -273.6943695669645535 ) ) ;
#68471 = CARTESIAN_POINT ( 'NONE',  ( -67.67029256810022275, -287.6845465779465485, -340.0328518220001115 ) ) ;
#68472 = CARTESIAN_POINT ( 'NONE',  ( -5.560483446708854416, -287.9037906763186356, -203.9745701137698575 ) ) ;
#68473 = DIRECTION ( 'NONE',  ( 0.9951408606192332362, 0.000000000000000000, -0.09846150276129254919 ) ) ;
#68474 = CARTESIAN_POINT ( 'NONE',  ( 33.86511549150084477, -288.1331623484406919, -253.5084609292994742 ) ) ;
#68475 = CARTESIAN_POINT ( 'NONE',  ( 36.74489105905452391, -295.7088925685389427, -284.1999065763107524 ) ) ;
#68476 = CARTESIAN_POINT ( 'NONE',  ( -112.3401198887111150, -276.5095152970703793, -279.9716269123249504 ) ) ;
#68477 = CARTESIAN_POINT ( 'NONE',  ( -22.93869317498068483, -277.2061377411561693, -346.0347151488948043 ) ) ;
#68478 = CARTESIAN_POINT ( 'NONE',  ( -33.58601733639245168, -290.1789309195158353, -194.8945091649860615 ) ) ;
#68479 = CARTESIAN_POINT ( 'NONE',  ( -114.2108522076812278, -278.6082686985297414, -265.8740857157554274 ) ) ;
#68480 = CARTESIAN_POINT ( 'NONE',  ( -47.52146415016976277, -299.9021612129894834, -196.3613431997065391 ) ) ;
#68481 = CARTESIAN_POINT ( 'NONE',  ( -43.41260863027326877, -261.7933826436608342, -500.4472285273179182 ) ) ;
#68482 = CARTESIAN_POINT ( 'NONE',  ( -112.0911152258861279, -282.4733336966953630, -276.4869313375109527 ) ) ;
#68483 = CARTESIAN_POINT ( 'NONE',  ( -48.18343439339133027, -254.6182378140904916, -482.3412084739035208 ) ) ;
#68484 = CARTESIAN_POINT ( 'NONE',  ( -96.26770673127754208, -276.0671235951129461, -315.5118790952369636 ) ) ;
#68485 = CARTESIAN_POINT ( 'NONE',  ( 35.90659070774783856, -279.7596681712798841, -286.5351921248577014 ) ) ;
#68486 = LINE ( 'NONE', #39107, #29126 ) ;
#68487 = CARTESIAN_POINT ( 'NONE',  ( -25.89326948699024200, -275.3887493745876327, -345.8040844350275052 ) ) ;
#68488 = CARTESIAN_POINT ( 'NONE',  ( -103.1602145007605742, -298.5192524226204682, -237.1018371702075456 ) ) ;
#68489 = CIRCLE ( 'NONE', #21588, 7.500000000000013323 ) ;
#68490 = CARTESIAN_POINT ( 'NONE',  ( 4.366011256174946453, -281.4245215264569424, -334.7819320839103625 ) ) ;
#68491 = CARTESIAN_POINT ( 'NONE',  ( -108.1941796040006949, -297.2489620859068395, -288.9399586035870584 ) ) ;
#68492 = CARTESIAN_POINT ( 'NONE',  ( -103.4322961883367071, -298.3732025329255748, -231.7166789724855960 ) ) ;
#68493 = CARTESIAN_POINT ( 'NONE',  ( -64.57273150917869486, -273.3533365635586279, -202.5939748196624350 ) ) ;
#68494 = CARTESIAN_POINT ( 'NONE',  ( 27.96384264065048697, -295.0596889621393188, -233.3744308843161264 ) ) ;
#68495 = CARTESIAN_POINT ( 'NONE',  ( 38.02306859478124323, -287.5206255436393690, -254.5127466676893562 ) ) ;
#68496 = CARTESIAN_POINT ( 'NONE',  ( 29.44289890549298505, -274.1629952905269079, -306.2506345709406332 ) ) ;
#68497 = CARTESIAN_POINT ( 'NONE',  ( 14.60214286555750007, -288.1784971513300206, -327.2738228997328065 ) ) ;
#68498 = ADVANCED_FACE ( 'NONE', ( #65117 ), #22451, .T. ) ;
#68499 = CARTESIAN_POINT ( 'NONE',  ( 27.87310784581042356, -286.1582819267348441, -236.9260460160904813 ) ) ;
#68500 = CARTESIAN_POINT ( 'NONE',  ( -104.2091343531707395, -289.0023027498201600, -236.2798331643919880 ) ) ;
#68501 = ORIENTED_EDGE ( 'NONE', *, *, #27196, .T. ) ;
#68502 = CARTESIAN_POINT ( 'NONE',  ( 125.5584997210034572, 149.0310057319917405, -265.9501514013184078 ) ) ;
#68503 = CARTESIAN_POINT ( 'NONE',  ( 17.86791605282812156, -287.7418860257988626, -318.2896183447253406 ) ) ;
#68504 = DIRECTION ( 'NONE',  ( 1.000000000000000000, 0.000000000000000000, 1.224646799147353207E-16 ) ) ;
#68505 = CARTESIAN_POINT ( 'NONE',  ( -70.35802020846388416, -284.4179180454589186, -339.6773586285799524 ) ) ;
#68506 = CARTESIAN_POINT ( 'NONE',  ( -36.36927160204471221, -291.1228179276945980, -193.5895777901128554 ) ) ;
#68507 = CARTESIAN_POINT ( 'NONE',  ( 37.64203410756061174, -283.3245629837664410, -283.9939352902941891 ) ) ;
#68508 = CARTESIAN_POINT ( 'NONE',  ( 14.81283117316611353, -282.0835769441939078, -214.3136896195209715 ) ) ;
#68509 = CARTESIAN_POINT ( 'NONE',  ( -101.7722262708617507, -283.9165226295036177, -304.7864499276090555 ) ) ;
#68510 = CARTESIAN_POINT ( 'NONE',  ( -73.79233343604141737, -279.5362303213421455, -335.9224547970185313 ) ) ;
#68511 = CARTESIAN_POINT ( 'NONE',  ( -113.9432200410501963, -296.4543085083787446, -278.1846176485049682 ) ) ;
#68512 = CARTESIAN_POINT ( 'NONE',  ( -98.26130087192044016, -274.4359593214324491, -229.1601332729453873 ) ) ;
#68513 = CARTESIAN_POINT ( 'NONE',  ( 23.95265296160118496, -290.9913533261548650, -227.7375408787310960 ) ) ;
#68514 = CARTESIAN_POINT ( 'NONE',  ( -33.77949833879921471, -297.0181016681536903, -197.0526761339389168 ) ) ;
#68515 = ORIENTED_EDGE ( 'NONE', *, *, #64655, .T. ) ;
#68516 = CARTESIAN_POINT ( 'NONE',  ( 208.6208076322478746, 32.98517505407394168, 14.49999999999999822 ) ) ;
#68517 = CARTESIAN_POINT ( 'NONE',  ( -109.1437777325013911, -286.2172707393778524, -290.0503612655991219 ) ) ;
#68518 = CIRCLE ( 'NONE', #468, 0.5000000000000004441 ) ;
#68519 = CARTESIAN_POINT ( 'NONE',  ( -8.491511416715544769, -295.7630534574070111, -341.4748132229282191 ) ) ;
#68520 = CARTESIAN_POINT ( 'NONE',  ( -110.4203193355407677, -285.1602312421156853, -273.6509839895760479 ) ) ;
#68521 = CARTESIAN_POINT ( 'NONE',  ( 36.65559886206544604, -274.8681280489462324, -290.8360653234958022 ) ) ;
#68522 = CARTESIAN_POINT ( 'NONE',  ( 22.12514995342863600, -293.5479771148287682, -221.6065640571553104 ) ) ;
#68523 = CARTESIAN_POINT ( 'NONE',  ( -10.41050100170151538, -284.5392949572897123, -199.4884431808527268 ) ) ;
#68524 = CARTESIAN_POINT ( 'NONE',  ( 30.87821778903895265, -293.4239062900076647, -234.5842530023379311 ) ) ;
#68526 = CARTESIAN_POINT ( 'NONE',  ( -45.36055653205941951, -289.4898311840251495, -342.9406290633068011 ) ) ;
#68525 = AXIS2_PLACEMENT_3D ( 'NONE', #22457, #74508, #67430 ) ;
#68527 = DIRECTION ( 'NONE',  ( -0.000000000000000000, -0.000000000000000000, 1.000000000000000000 ) ) ;
#68528 = CARTESIAN_POINT ( 'NONE',  ( 154.7659666677360235, 19.56018909072649237, -12.94946946942526189 ) ) ;
#68529 = CARTESIAN_POINT ( 'NONE',  ( 161.0643044244293947, 217.6531385774068781, -202.3978598018051400 ) ) ;
#68530 = CARTESIAN_POINT ( 'NONE',  ( -101.9419003248663387, -286.6089114077928457, -229.7468115569240865 ) ) ;
#68531 = CARTESIAN_POINT ( 'NONE',  ( -85.28047601435909542, -294.9094976428776818, -210.1954327657594206 ) ) ;
#68532 = ORIENTED_EDGE ( 'NONE', *, *, #57514, .T. ) ;
#68533 = CARTESIAN_POINT ( 'NONE',  ( 34.87395367371294697, -280.3067725856217862, -257.7466255189837625 ) ) ;
#68534 = CARTESIAN_POINT ( 'NONE',  ( -110.6478376737737648, -277.9214608828444852, -294.0264843838895104 ) ) ;
#68535 = CARTESIAN_POINT ( 'NONE',  ( -16.43329065755524354, -282.3231646729834097, -198.5080259311049247 ) ) ;
#68536 = CARTESIAN_POINT ( 'NONE',  ( 198.7516057561506955, 282.3040474041899301, -110.9336064257162349 ) ) ;
#68537 = CARTESIAN_POINT ( 'NONE',  ( 22.05370066387754235, -280.7766784376967735, -318.4524602079354167 ) ) ;
#68538 = CARTESIAN_POINT ( 'NONE',  ( -16.69322455083104373, -284.3401677694872660, -198.5750222909682918 ) ) ;
#68539 = CARTESIAN_POINT ( 'NONE',  ( -105.7384823260575359, -274.8371672387395961, -237.7699280267998176 ) ) ;
#68540 = B_SPLINE_SURFACE_WITH_KNOTS ( 'NONE', 3, 3, ( 
 ( #14917, #2100, #23414, #30507, #74055, #67442, #8268, #52280, #30051, #37148, #38052, #66055, #58932, #66961, #30991, #31448, #38539, #88718, #2569, #22469, #22023, #60337, #72673, #36678, #65600, #713, #29598, #87321, #75459, #82081, #10580, #47018, #24806, #68837, #26195, #55089, #69291, #82559, #40374, #4420, #76866, #18165, #25267, #33774, #11046, #39916, #89174, #53692, #90561, #3487, #18630, #47496, #38984, #24326, #76405, #89636, #68359, #60798, #83958, #17707, #61729, #32839, #83474, #39443, #46560, #19107, #53203, #32380, #46101, #11527, #54603, #17239, #3965, #62196, #54144, #75006, #10118, #90115, #61281, #91026, #47962, #67897, #3020, #83013, #11991, #31906, #25719, #33298, #40840, #69759, #4890, #71647, #13418, #6305, #19562, #49839, #93397, #5385, #27614, #27140, #13879, #64095, #91520, #70250, #84414, #35173, #50308, #7233, #41798, #34250, #71176, #63156, #6780, #92935, #79213, #35657, #34712, #42263, #20972, #26676, #56511, #42732, #92451, #20520, #57440, #77810, #28096, #63626, #85370, #56025, #64572, #56983, #55566, #28549, #85821, #49388, #78736, #14356, #84880, #78280, #70709, #20031, #86281, #12959, #48908, #21434, #43216, #72117, #62687, #48428, #77332, #91987, #12466, #41313, #5840, #81499, #65484, #16646, #30395, #37936, #22359, #29009, #51233, #87669, #601, #15730, #66845, #1980, #16190, #29484, #81047, #45042, #23754, #58824, #65949, #74402, #22819, #51688, #36108, #58369, #37483, #44120, #59287, #88133, #79671, #65026, #23291, #36569, #15260, #7684, #30871, #87211, #8607, #73495, #52164, #80121, #73024, #59765, #126, #8152, #86750, #73943, #1509, #57894, #80577, #9058, #1060, #21912, #50786, #37035, #29939, #88606, #66393, #52617, #45500, #44591, #14812, #43667, #72562, #68245, #54489, #39327, #61162, #4308, #24688, #39796, #10461, #75346, #67780, #11411, #75804, #38417, #83357, #46903, #3369, #32729, #54964, #2906, #32257, #82446, #60684, #89999, #53571, #31790, #68718, #90449, #18993, #33186, #82895, #62076, #10002, #9532, #25154, #90909, #83840, #38873, #47846, #3848, #40262, #89524, #2458, #17594, #54028, #46444, #18051, #69179, #26075, #18507, #10928, #47371, #76285, #67326, #61617, #25606, #31334, #60221, #89060, #24210, #53085, #81964, #17120, #45986, #74891, #26559, #76748, #63980, #77216, #55913, #48315, #42619, #12344, #49272, #20402, #71061, #27024, #70131, #6671, #40727, #91870, #33654, #6193, #42143, #69644, #27494, #49731, #41681, #21325, #11876, #77694, #41193, #78628, #71538, #4772, #62563, #48786, #78167, #34136, #12843, #85715, #56392, #13305, #91404, #92820, #13770, #19449, #70599, #5267, #27983, #35060, #55448, #84299, #63039, #56874, #64461, #84765, #19915, #5726, #85254, #34601, #20860, #63511, #35548, #28439, #92339, #93288, #57332, #86174, #86512, #14119, #57211, #29245, #79894, #8385, #87440, #72337, #22586, #93170, #92693, #93623, #51461, #44362, #28322, #73272, #86986, #835, #78968, #85597, #42983, #50551, #86052, #7456, #29717, #58599, #72789, #21201, #43892, #7913, #80350, #21675, #28781, #37264, #79448, #14584, #27863, #50073, #358, #7010, #22139, #51007, #42500, #56755, #15033, #71889, #35882, #64344, #15491, #64799, #65253, #36338, #36803, #57666, #43441, #20744, #49615, #58140, #78510, #65724, #13648, #71413, #6545, #35423, #31111, #10702, #66170, #67094, #30633, #68015, #32026, #87899, #30168, #38179, #38656, #23532, #2227, #75125, #16888, #9781, #23051, #53329, #3144, #8837, #59998, #59533, #17369, #67560, #1286, #73725, #51929, #2689, #53809, #59051, #45276, #37715, #74657, #66621, #10235, #31570, #82677, #39103, #88837, #45745, #24450, #80819, #23987, #46221, #52860, #81738, #60923, #81278, #60460, #89295, #82215, #88382, #89770, #24932, #15968, #17826, #46679, #16424, #75582, #44822, #1745, #52401, #74179, #9297, #39560, #47140, #83133, #25383, #18284, #68482, #61402, #54263, #76050, #90234, #3618, #32505, #93266, #65356, #22236, #44463, #29812, #14686, #58693, #35527, #35041, #35979, #87537, #80445, #64440, #15590, #29352, #36908, #21304, #27963, #50177, #86614, #28420, #43541, #65826, #933, #15130, #57311, #79993, #43993, #22684, #57768, #64899, #73368, #21784, #50660, #63955, #86153, #36441, #43086, #58244, #87087, #78605, #92795, #51107, #79073, #14225, #6647, #51557, #71990, #7556, #72438, #72890, #7108, #93715, #56852, #85693, #28880, #20839, #8014, #463, #49710, #79546, #13750, #42598, #71513, #8480, #9398, #66719, #10333, #68112, #30263, #66266, #74275, #74757, #59636, #38282, #17465, #52959, #45851, #59155, #89393, #39200, #44919, #67195, #1847, #53431, #9876, #37359, #16065, #87999, #38752, #89870, #46773, #81372, #73821, #16986, #8934, #46315, #67656, #25031, #75219, #2331, #81836, #60555, #1381, #31210, #82315, #60095, #88934, #3238, #24083, #2782, #30734, #32128, #61024, #16521, #53902, #31663, #23152, #52036, #24547, #82770, #17922, #80922, #37812, #88483, #23630, #52495, #45372, #83700, #12702, #61494, #76149, #75674, #41542, #41057, #62904, #5123, #69052, #77553, #11282, #76619, #3719, #47237, #25941, #69983, #39661, #40136, #70466, #91740, #63374, #4181, #33055, #54822, #92204, #33515, #61944, #5594, #34468, #19317, #18862, #84169, #32605, #68583, #90326, #20259, #25480, #54359, #10799, #26892, #91262, #11742, #55779, #84632, #83233, #19781, #85109, #55319, #18380, #27360, #90781, #47719, #77080, #48652, #40595, #69509, #4640, #48179, #56249, #12211, #34000, #62421, #26426, #65704, #49595, #78491, #57645, #34926, #50053, #49135, #28302, #64779, #21182, #78949, #29227, #86493, #13629, #21656, #85578, #816, #57192, #72317, #35862, #22121, #35402, #92673, #7895, #50532, #78032, #14099, #43873, #42480, #63841, #13172, #71393, #42963, #58122, #58580, #71868, #79430, #93604, #43422, #29696, #15014, #6990, #28762, #72770, #36784, #79874, #42007, #86033, #87419, #27843, #6526, #70923, #6054, #14566, #36320, #7438, #64322, #50989, #93148, #65234, #56732, #20725, #340, #86967, #80329, #23030, #82192, #9760, #10212, #80800, #51909, #66600, #39080, #74157, #87878, #46197, #75102, #59977, #1722, #31089, #44343, #15472, #73253, #60899, #8365, #37246, #22567, #38635, #38156, #52379, #67538, #31546, #66149, #2667, #32002, #2205, #59031, #67994, #44803, #1266, #23964, #60438, #30148, #51441, #15948, #88816, #89274, #52838, #81714, #16864, #16401, #3122, #73704, #8813, #45723, #37694, #23510, #30609, #59511, #67071, #88360, #81256, #24424, #74633, #45252, #53307, #9273, #17346, #5374, #20510, #77801, #64086, #77323, #40829, #49830, #63617, #24908, #56014, #85812, #91510, #11981, #55078, #26666, #91978, #6295, #6771, #63147, #34704, #12951, #85361, #71639, #56974, #27131, #41789, #20963, #78727, #84871, #70700, #55556, #92925, #35164, #70241, #28087, #5831, #47952, #83947, #92442, #20021, #13870, #27605, #49378, #19099, #56502, #78271, #13410, #41304, #84404, #42722, #76855, #12456, #69749, #42253, #71167, #4880, #35646, #89748, #48899, #33764, #62676, #19553, #34241, #66384, #30384, #86272, #28540, #36559, #37026, #21903, #592, #73485, #15251, #8143, #21424, #51678, #1500, #7224, #29474, #28999, #15721, #65940, #93387, #72107, #50298, #1051, #52155, #9049, #43658, #36098, #73014 ),
 ( #80567, #57431, #79204, #14347, #29930, #44582, #58815, #44111, #87658, #58362, #81037, #65018, #118, #22809, #43206, #65474, #64563, #72553, #80112, #87202, #22350, #8597, #37474, #57885, #59277, #86741, #16181, #7675, #88123, #51222, #23281, #50776, #79662, #45033, #73933, #14802, #2898, #32722, #38408, #52608, #1970, #67317, #38865, #46895, #47362, #9992, #75337, #53563, #32248, #18498, #3840, #67771, #82435, #61607, #90441, #31781, #17585, #59756, #76277, #88596, #30862, #37927, #25144, #46434, #60675, #54020, #75796, #23745, #82887, #66833, #10453, #74392, #83350, #60212, #81490, #39319, #18043, #16637, #45491, #9520, #68237, #10919, #3358, #61155, #89990, #89513, #54481, #2447, #31325, #39787, #89051, #24678, #24200, #17111, #68710, #25598, #53077, #81954, #45975, #74882, #77686, #47838, #27977, #19442, #34595, #91864, #78161, #91397, #54955, #63971, #12837, #40255, #70123, #6187, #11867, #26066, #69171, #40718, #12337, #20395, #20854, #77207, #48780, #27018, #5720, #85709, #71055, #41183, #55907, #35054, #92812, #5260, #84759, #69636, #13299, #49266, #84292, #42137, #19907, #62067, #4298, #41675, #34129, #56867, #70593, #63504, #33178, #92333, #49725, #90901, #48308, #11403, #83832, #4764, #18986, #76740, #27488, #56382, #85248, #33645, #62555, #26552, #63033, #55440, #50190, #28894, #44009, #42613, #79090, #44481, #65842, #66284, #43100, #14242, #57783, #1397, #36455, #72005, #8496, #37374, #22253, #86630, #87103, #6664, #71530, #7124, #79559, #35540, #35994, #21799, #72907, #64455, #64913, #73386, #950, #30282, #16, #50673, #14700, #59171, #65370, #43555, #88017, #23172, #51124, #72451, #80009, #93281, #28433, #57326, #78622, #86168, #21319, #13765, #29828, #480, #7570, #58711, #87553, #29368, #22701, #58260, #15149, #8031, #36928, #51575, #80461, #15609, #39217, #16083, #80938, #66736, #24565, #68133, #53452, #31681, #17483, #45871, #68601, #52513, #81389, #60576, #37831, #52979, #52055, #31227, #67673, #24099, #81853, #32146, #89411, #16537, #82333, #88500, #3737, #60112, #75237, #38769, #25048, #38301, #1863, #10817, #46334, #44936, #17003, #46791, #45391, #30754, #73837, #74291, #74777, #61045, #61511, #9894, #10351, #2799, #3256, #32621, #17940, #89889, #53920, #75693, #39679, #82788, #90343, #9415, #8951, #59656, #88952, #23647, #67216, #2349, #83252, #70001, #19335, #56269, #41076, #77571, #47254, #5142, #85129, #18397, #33532, #20281, #11300, #25958, #25498, #49156, #84650, #12721, #48670, #18881, #27380, #41563, #47736, #78051, #54839, #26445, #76168, #90799, #69527, #19802, #40153, #83720, #13192, #70485, #42027, #76635, #11759, #4659, #70942, #77099, #40611, #6073, #34947, #62923, #62438, #34020, #69070, #4198, #33073, #63860, #61963, #91280, #54376, #5613, #91758, #55336, #34488, #63394, #84187, #92224, #48197, #26910, #12230, #55798, #81200, #73650, #60380, #46144, #22974, #87824, #8760, #31492, #75047, #89219, #38580, #24370, #52779, #75502, #88299, #23456, #67483, #44748, #59922, #58975, #38098, #74570, #31033, #88762, #39028, #2614, #52322, #53248, #1667, #10624, #67008, #82130, #45662, #31949, #45196, #37638, #17747, #17287, #51846, #23908, #53734, #16346, #66546, #80741, #74099, #81658, #67941, #68403, #16806, #10159, #9699, #3064, #39482, #24851, #60841, #89684, #82600, #3532, #15892, #30549, #9218, #2144, #41360, #11565, #63198, #76905, #83055, #90159, #12035, #26241, #92028, #48001, #84454, #54185, #40882, #27183, #25307, #40413, #56070, #18209, #32880, #32422, #84923, #91561, #19604, #55134, #47540, #90601, #62731, #48472, #41838, #20074, #69800, #48954, #61768, #61321, #33339, #77852, #13002, #25762, #70749, #26718, #34290, #18674, #47059, #76444, #83998, #54644, #4935, #75963, #11093, #12509, #83517, #77372, #70294, #39959, #19146, #62236, #68875, #33821, #55605, #4005, #69331, #5425, #4462, #91070, #57937, #49431, #5883, #86792, #6345, #78778, #71218, #65524, #35217, #72153, #43255, #166, #49880, #92977, #29526, #63668, #21013, #56557, #29045, #65067, #92491, #50350, #72602, #64610, #44160, #34753, #6822, #64144, #7724, #642, #27659, #85411, #71693, #7269, #57024, #35696, #14850, #79255, #36146, #20559, #21951, #36606, #42309, #93436, #28135, #50824, #79708, #78319, #13458, #85862, #43703, #87252, #13919, #42776, #28590, #14396, #57480, #58406, #22398, #51270, #80163, #86321, #15301, #21473, #8195, #37973, #24248, #9096, #30911, #67817, #88173, #9569, #73979, #45079, #37519, #74927, #45537, #37076, #53122, #16682, #66881, #2493, #24727, #66429, #2018, #52202, #30431, #38457, #59801, #89558, #73533, #8642, #81534, #58861, #88642, #73065, #81084, #23790, #52654, #74438, #82002, #67363, #1548, #31370, #15772, #53610, #16228, #60259, #89096, #46024, #59322, #22858, #31828, #17158, #65985, #10038, #2942, #23333, #87708, #1096, #38908, #60719, #82481, #17628, #29977, #51724, #80616, #44631, #27058, #12382, #76320, #90946, #41228, #70167, #47410, #26110, #10963, #19483, #55483, #25641, #77252, #55003, #3403, #10496, #83876, #40298, #5302, #62115, #4809, #68281, #19027, #34172, #39365, #54524, #63074, #32294, #46938, #46480, #91904, #11911, #33689, #69678, #39830, #48349, #75840, #11446, #61200, #18084, #90483, #40760, #90036, #68754, #55945, #62599, #84800, #3885, #32762, #83393, #75383, #4342, #61650, #25188, #54061, #47881, #18543, #76785, #82932, #69213, #33219, #91442, #26593, #84332, #58298, #7162, #35580, #49766, #36037, #28936, #12878, #64954, #29407, #93321, #56425, #65413, #42179, #34633, #21360, #55, #77727, #48821, #63544, #86208, #57822, #50229, #28473, #64495, #78661, #86673, #21838, #41716, #50714, #19950, #57366, #85286, #523, #71092, #92373, #79133, #79600, #70632, #5760, #27532, #14281, #14741, #43142, #72046, #43596, #13802, #36496, #20436, #49305, #72492, #78199, #20894, #13338, #92852, #7608, #85747, #42654, #6225, #35095, #64013, #28016, #56907, #71571, #6706, #16577, #73875, #60153, #73426, #36966, #45913, #59696, #22292, #52096, #81895, #87596, #8078, #51163, #22742, #88059, #2388, #2842, #59213, #30797, #8993, #81428, #67712, #53017, #23216, #37871, #17047, #74819, #80980, #66776, #51616, #88992, #31266, #66325, #24139, #1907, #44050, #80050, #88539, #16123, #9934, #23688, #45433, #15190, #52552, #38808, #72951, #1439, #31724, #65879, #80504, #87142, #988, #74333, #9457, #38343, #15652, #29870, #44522, #44974, #58754, #8536, #37415, #67256, #30324, #61092, #26490, #47776, #48246, #25087, #89931, #10859, #77148, #18437, #32186, #84232, #19382, #4237, #39722, #69112, #82375, #24612, #17525, #5196, #46375, #53499, #60615, #76678, #47295, #53961, #12278, #41122, #33117, #68646, #62006, #75275, #10394, #39259, #89453, #68174, #3295, #82828, #11803, #76212, #90384, #40654, #69573, #17981, #4702, #70054, #40195, #46833, #75735, #3780, #32663, #90841, #33579, #61550, #25539, #54420, #26002, #62488, #54887, #83766, #18922, #83291, #11341, #91328, #55380, #19848, #62971, #55848, #34069, #48719, #77622, #12771, #41613, #70535, #91805, #84701, #26957, #65970, #46008, #37505, #52640, #16214, #2479, #15755, #73046, #81986, #2001, #58390, #88156, #24231, #29961, #44142, #87234, #58847, #30417, #38440, #38894 ),
 ( #31356, #23315, #67803, #29509, #59308, #87690, #60244, #89082, #51254, #22382, #1531, #30894, #80598, #52188, #67349, #73965, #66866, #80145, #16667, #53108, #1081, #81069, #22843, #74424, #59787, #15285, #37060, #8176, #88628, #17142, #51710, #45065, #23775, #9079, #81520, #10024, #74913, #37959, #45522, #44615, #73519, #9553, #8628, #66414, #70967, #13217, #77123, #34971, #48691, #54866, #61986, #77597, #91781, #63885, #19825, #56293, #25981, #12746, #92721, #90821, #12252, #27891, #83746, #4681, #4220, #56781, #63419, #85157, #27405, #91306, #6099, #33555, #5169, #18903, #69551, #48221, #92248, #47758, #62465, #85623, #20309, #20769, #26469, #55358, #41098, #49641, #55820, #84210, #78536, #13675, #41588, #70027, #70510, #76656, #11783, #40633, #42525, #19357, #34044, #33095, #49180, #5637, #62947, #78074, #42053, #26932, #84676, #34512, #51034, #14149, #23078, #93650, #86080, #72816, #58625, #35451, #6574, #21231, #43921, #87466, #7942, #79922, #36836, #65281, #87927, #71917, #7038, #15059, #57238, #72366, #71437, #50582, #87014, #43469, #7483, #51488, #65754, #35908, #863, #43013, #51958, #79477, #29744, #58170, #44392, #57694, #50100, #30195, #22613, #64370, #36368, #66197, #64826, #78994, #93196, #28810, #386, #80376, #80849, #29275, #22166, #37290, #1313, #15517, #73300, #86537, #8412, #59085, #14612, #15997, #28348, #21706, #8864, #89324, #38683, #75610, #60487, #3172, #66650, #24479, #10734, #37742, #52887, #39590, #30660, #45303, #44849, #68513, #10264, #32056, #68045, #38209, #46707, #74208, #45775, #1776, #16451, #88865, #39134, #59562, #9326, #3649, #60950, #32539, #67123, #2258, #24014, #61432, #2718, #31141, #90264, #25413, #82244, #81767, #53358, #88411, #23562, #52430, #83163, #81305, #60028, #73752, #89801, #17399, #74686, #24963, #53839, #16917, #82705, #54292, #46248, #9809, #67588, #31598, #75152, #17856, #5531, #76080, #47171, #32989, #84565, #34401, #19712, #91674, #77483, #12145, #34862, #18793, #47651, #26827, #4117, #19255, #18315, #91191, #33934, #84106, #48113, #92139, #55714, #76553, #48583, #54753, #63775, #26359, #41473, #5051, #85039, #4573, #61880, #70858, #12626, #11212, #77017, #13109, #11676, #90711, #40069, #40525, #40990, #27294, #27774, #69912, #70404, #62841, #63308, #92604, #77966, #68987, #56181, #20189, #49069, #41946, #5990, #25871, #56668, #83630, #69443, #55249, #33447, #62350, #85970, #85517, #22513, #50932, #72712, #14957, #78882, #87363, #21120, #86428, #13565, #57128, #35800, #79816, #49534, #49988, #51384, #7834, #73189, #14030, #42891, #64713, #8308, #43362, #71804, #15413, #44281, #29160, #93540, #280, #42415, #78427, #71326, #30092, #6456, #35331, #20663, #36722, #7375, #21585, #65641, #755, #64257, #29639, #1210, #65175, #28241, #37190, #6926, #93086, #86908, #58518, #28699, #57584, #50466, #58057, #80275, #22063, #43812, #66098, #79369, #14505, #72258, #36256, #31621, #8890, #24037, #23104, #2282, #38706, #88889, #52913, #3195, #60512, #23586, #89347, #59586, #39614, #31165, #46271, #9833, #89827, #9350, #66673, #75634, #24503, #51985, #81792, #17879, #52453, #37768, #80875, #81327, #16940, #32079, #32563, #45802, #53384, #67613, #17422, #3677, #82727, #74712, #2741, #46731, #10757, #82269, #75175, #16474, #24988, #60979, #60051, #53861, #10288, #73775, #16022, #68538, #39158, #68070, #61455, #44873, #45330, #1801, #30686, #74231, #88437, #38235, #67148, #26849, #77507, #6013, #85065, #69936, #20216, #90738, #90286, #91218, #49094, #41969, #25896, #70882, #84589, #92163, #76577, #83190, #11700, #48136, #54778, #5078, #27320, #56206, #70429, #83656, #41500, #5555, #77993, #19278, #26385, #34888, #77039, #12170, #25437, #18819, #91697, #4598, #19739, #48607, #40094, #54315, #12654, #47676, #69466, #61903, #13133, #40551, #62864, #33960, #34425, #33471, #62374, #18338, #47193, #55273, #76106, #63332, #55737, #11239, #41013, #69010, #84128, #4141, #33012, #64736, #28264, #65663, #29660, #85539, #27799, #35822, #36278, #21143, #93564, #72734, #14527, #7396, #20687, #50953, #776, #6481, #28721, #57153, #14976, #65198, #92628, #71350, #49557, #301, #51404, #9594, #42916, #35359, #72277, #64280, #7854, #29181, #80296, #36741, #57606, #43382, #22083, #56692, #86449, #43832, #21607, #50489, #58540, #78906, #58078, #79390, #86930, #85993, #87385, #79836, #22532, #14053, #50013, #15435, #44301, #73210, #63799, #78452, #13588, #93109, #42440, #71830, #6949, #83897, #67840, #19048, #32783, #40319, #24752, #31392, #53634, #90057, #2966, #18108, #69234, #4363, #18567, #31851, #83413, #47433, #26133, #61223, #68304, #76806, #25210, #54083, #38481, #60740, #39855, #46503, #61671, #90503, #82025, #67385, #25664, #38931, #17652, #10061, #33241, #89581, #10985, #75862, #54545, #82504, #75406, #62136, #2515, #10522, #89119, #76342, #3906, #60282, #82953, #11468, #3426, #24270, #53145, #39389, #32321, #90967, #55028, #17183, #46046, #46960, #68777, #47904, #74951, #20913, #56447, #49325, #62624, #92874, #42671, #48371, #70650, #70191, #56925, #13358, #40781, #19503, #33712, #78219, #93338, #50245, #84819, #77273, #20457, #12402, #49782, #42199, #28489, #78679, #77748, #85309, #64032, #69699, #5778, #85763, #41737, #63566, #6725, #27079, #71113, #12899, #34652, #5324, #13819, #6243, #4828, #71588, #35112, #92392, #28036, #57382, #34192, #27552, #19968, #63096, #35597, #64512, #86225, #21375, #11932, #91463, #26614, #55505, #84354, #48843, #41250, #91924, #55966, #79151, #16137, #44538, #66340, #8551, #72506, #80995, #14756, #80064, #7177, #50730, #29423, #73441, #43159, #79614, #44989, #1454, #66791, #43610, #7626, #58313, #1921, #36981, #36511, #9007, #37886, #22761, #87157, #87611, #36052, #72060, #64970, #23703, #73, #28951, #14299, #30340, #1005, #15207, #59230, #88076, #57837, #23232, #88555, #58769, #21856, #30815, #65426, #86691, #80518, #52112, #540, #22306, #51177, #51632, #73890, #15671, #37431, #59712, #72965, #44064, #8094, #65893, #29885, #81446, #74350, #52566, #38359, #2403, #67273, #31283, #89007, #60169, #9473, #16594, #45450, #64612, #56072, #71220, #34755, #21015, #34292, #91563, #6824, #20561, #76907, #13004, #42779, #48474, #62733, #12037, #77374, #48956, #57026, #57482, #20077, #85413, #63670, #42311, #28592, #13921, #77854, #92493, #71695, #35698, #41840, #27662, #12512, #49882, #85864, #27185, #78780, #56559, #4938, #40884, #69802, #41362, #93438, #35220, #86323, #70296, #5427, #92030, #48003, #5885, #19606, #33823, #26720, #49433, #84925, #78321, #55607, #84456, #63200, #70751, #13460, #6347, #64146, #92979, #28137, #51271, #8643, #30433, #14398, #37520, #30913, #1097, #57940, #66883, #43705, #36148, #22859, #66430, #79257, #50353, #65069, #87709, #1550, #51725, #29978, #80618, #15302, #37975, #21953, #50826, #58862, #7271, #22399, #21475, #643, #37077, #87253, #80164, #59324, #15773, #79710, #44632, #86794, #2021, #29527, #73534, #8196, #88176, #7726, #168, #73981, #23335, #43257, #44161, #16230, #14852, #29047, #72155, #72604, #73067, #52204, #59803, #65986, #81086, #45081, #9098, #36607, #65526, #58407, #39367, #54526, #18545, #89560, #68283, #53124, #61652, #3887, #67819, #25643 ),
 ( #45539, #75842, #83395, #31372, #24730, #3405, #47413, #76322, #53612, #32297, #82004, #90485, #32764, #2944, #11448, #61202, #74440, #52656, #90038, #82483, #40300, #10498, #46940, #16684, #25190, #69215, #81536, #31830, #4344, #9572, #89098, #88644, #33221, #54063, #10965, #18086, #17161, #23792, #24250, #17630, #38459, #60261, #38910, #82934, #67365, #46026, #2495, #39833, #74929, #10040, #60721, #46482, #75385, #68756, #33691, #85749, #20896, #5762, #41230, #70634, #83878, #26112, #19029, #6709, #47883, #55006, #62117, #49307, #77730, #91906, #78201, #71094, #76787, #13340, #71573, #41718, #62602, #13804, #84334, #11913, #63546, #42181, #40762, #90948, #69680, #34636, #6227, #92375, #27534, #56427, #55947, #78663, #91444, #26595, #85289, #55485, #63076, #19485, #70170, #12880, #34174, #27060, #35097, #20438, #48351, #64015, #77254, #42656, #5304, #92855, #48823, #28018, #12384, #84802, #49768, #56909, #19952, #525, #30326, #36039, #50232, #93323, #64956, #36498, #44524, #44976, #7610, #72953, #51165, #29872, #16125, #1441, #36968, #64497, #43144, #57368, #8080, #23218, #73877, #14743, #72048, #44052, #7164, #73428, #65881, #52098, #8538, #65415, #15192, #87598, #28475, #29410, #80506, #58300, #87144, #59216, #50716, #990, #22294, #80052, #57, #37417, #58756, #86210, #15654, #22744, #51619, #66328, #80982, #28938, #88061, #43598, #86675, #35582, #79602, #57824, #21362, #79135, #14284, #21840, #72494, #3782, #9459, #8995, #9936, #61552, #54422, #38345, #83293, #3298, #10862, #88994, #1909, #24141, #60617, #67258, #82377, #39724, #68648, #82830, #2390, #53963, #17983, #90386, #31726, #38810, #47297, #89455, #24615, #37873, #31268, #10396, #17049, #32188, #61094, #52554, #66779, #89933, #60155, #81897, #74336, #32665, #53019, #75277, #46377, #25089, #45915, #74821, #25541, #30799, #67714, #59698, #46835, #68176, #88541, #53501, #75737, #2844, #23690, #81430, #17527, #39261, #18440, #16579, #45435, #40197, #48248, #48722, #33582, #12280, #85184, #26959, #19850, #33119, #63442, #13240, #18924, #41125, #40656, #27429, #63912, #5198, #70056, #20794, #34071, #91807, #76214, #69575, #77624, #84234, #5659, #34534, #26005, #11343, #92273, #76680, #55382, #47778, #42076, #11805, #12773, #41615, #70536, #26492, #4704, #6124, #69114, #91330, #62008, #56320, #20333, #4239, #55850, #49203, #62973, #90843, #54889, #77150, #62490, #78099, #70992, #83768, #19384, #84703, #34995, #92746, #27917, #56804, #85646, #87039, #6598, #36861, #80399, #86106, #14637, #14177, #886, #51057, #78560, #57263, #71467, #22189, #37314, #87951, #28835, #21255, #58195, #50125, #87489, #79945, #66222, #22639, #21735, #29300, #7968, #13698, #43495, #29769, #79501, #7508, #44416, #64850, #15083, #50611, #72391, #43039, #51511, #43943, #42550, #58647, #72840, #36393, #65777, #1336, #71941, #65306, #57719, #7062, #414, #93677, #35932, #15545, #73324, #59109, #8435, #30218, #49665, #79024, #35476, #64393, #93219, #28372, #86566, #31078, #73696, #81245, #65692, #72306, #806, #37237, #15004, #59023, #16392, #45242, #88351, #72760, #30597, #23502, #51898, #74148, #43863, #14554, #44332, #38142, #59966, #7881, #43411, #8805, #9265, #29686, #7426, #58570, #80791, #36772, #37685, #67059, #2194, #52370, #87410, #36307, #65223, #29213, #8354, #73243, #58112, #66592, #1713, #52825, #17336, #54232, #60884, #76014, #11147, #2657, #81704, #40009, #53294, #31992, #24414, #18728, #82180, #25352, #90203, #47107, #3109, #46187, #76493, #16853, #67983, #9750, #68926, #18254, #45708, #3583, #25812, #17793, #91123, #74621, #53777, #75092, #54692, #47589, #38624, #67527, #24897, #83100, #10201, #82644, #61819, #32473, #4057, #31536, #32927, #83566, #89264, #46646, #39070, #90650, #11616, #60423, #89735, #75547, #40461, #69379, #10672, #39527, #68448, #61370, #4510, #33388, #62287, #44099, #65464, #92080, #5934, #79652, #55188, #84976, #72544, #56123, #77910, #22341, #41413, #56611, #27234, #20127, #84507, #29464, #92544, #84046, #7665, #63719, #49012, #49480, #73005, #19653, #13051, #5472, #77423, #41888, #70346, #48522, #85463, #14793, #37016, #51212, #27712, #34342, #43648, #36548, #69852, #26294, #581, #26769, #63249, #91614, #87193, #55654, #20610, #58353, #80103, #70799, #12562, #15242, #19192, #34805, #76956, #8133, #65930, #48051, #12083, #40932, #4986, #33872, #62781, #1960, #59266, #2887, #60664, #22800, #58805, #66822, #67307, #52147, #30853, #9982, #45482, #38398, #51667, #81942, #31772, #37465, #59746, #88114, #45966, #2436, #29921, #8587, #80557, #31315, #82425, #39308, #73923, #66374, #9509, #1491, #38854, #60201, #17575, #67761, #88587, #74381, #53067, #87649, #23735, #74872, #52598, #81479, #89501, #16171, #89039, #16628, #24189, #23271, #24666, #17099, #15711, #53553, #46424, #75326, #10442, #1042, #81027, #44572, #9040, #45023, #73475, #37918, #30375, #4752, #55427, #77672, #63020, #47826, #91852, #68700, #68225, #69160, #27006, #19895, #3830, #48766, #62542, #70108, #54469, #61145, #83339, #26054, #32712, #76728, #5248, #34118, #48294, #61597, #19431, #77196, #55894, #90891, #4287, #12825, #54941, #83821, #3345, #90430, #84748, #12325, #25586, #41169, #32236, #89980, #18973, #33165, #25134, #11855, #40704, #54010, #18485, #69624, #76265, #91384, #26540, #18031, #82877, #84280, #47348, #11392, #39775, #46885, #40244, #33632, #75787, #10907, #62056, #35044, #65359, #5706, #56855, #92322, #64902, #7111, #34582, #86156, #14689, #6650, #79996, #41664, #42601, #6175, #43544, #7559, #63491, #27477, #13753, #14228, #92798, #71516, #50663, #21307, #79076, #56369, #28883, #72441, #78149, #35530, #63958, #86617, #43089, #70581, #49254, #85233, #71993, #29355, #20384, #20842, #13287, #50180, #42124, #79549, #35982, #58247, #36444, #64443, #3, #57771, #71041, #93269, #21787, #28423, #57314, #466, #85696, #87090, #22239, #51110, #27966, #49713, #78608, #43996, #88937, #52498, #44922, #38285, #60559, #73371, #73824, #88002, #66269, #8937, #30266, #8483, #45375, #2334, #24551, #9879, #88486, #38755, #15593, #15133, #16068, #67659, #89397, #44466, #53435, #9401, #16989, #1384, #8017, #59158, #66722, #37362, #23633, #45854, #23155, #2785, #72893, #52039, #65829, #67198, #74278, #36911, #59639, #81839, #37815, #936, #29815, #1850, #80925, #74760, #31666, #58696, #87540, #30737, #81375, #16524, #31213, #24086, #60098, #52962, #22687, #51560, #80448, #25035, #47241, #46777, #33519, #83704, #17469, #89874, #10337, #54826, #69987, #26895, #61498, #53906, #90785, #82774, #26430, #18866, #5127, #55323, #54363, #61948, #40599, #46319, #76153, #62425, #18384, #40140, #77084, #3723, #47723, #83237, #11286, #75678, #84173, #76623, #75223, #91266, #25945, #69056, #11746, #34004, #10803, #4185, #90330, #39665, #33059, #32609, #68587, #69513, #4644, #91744, #12215, #19321, #41061, #17926, #82319, #48183, #62908, #39204, #25484, #68116, #3242, #32132, #61028, #48656, #42011, #13633, #85113, #35406, #86497, #21660, #35866, #49139, #6994, #64783, #43426, #78495, #85582, #344, #42484, #71397, #55783, #20263, #57196, #63845, #78953, #14103, #5598, #84636, #42967, #56253, #34930, #27364, #50536, #78036, #28306, #93152 ),
 ( #13176, #79434, #14570, #86037, #92677, #64326, #77557, #19785, #12706, #41546, #70470, #34472, #63378, #71872, #6530, #20729, #93608, #28766, #92208, #57649, #65238, #21186, #70927, #7442, #6058, #27847, #50057, #72321, #56736, #49599, #36324, #1727, #16406, #30614, #8819, #88365, #23034, #45728, #29701, #58584, #37699, #15018, #30152, #29231, #8369, #44808, #1270, #59035, #9278, #66605, #87423, #59516, #65708, #74638, #37250, #52384, #15952, #2210, #15476, #72774, #81720, #23515, #58126, #87882, #23969, #22571, #43877, #86971, #51445, #51913, #38161, #38640, #80804, #81261, #73709, #45258, #9765, #88821, #74162, #67076, #52843, #16869, #31094, #59982, #80333, #67543, #22125, #66154, #50993, #79878, #7899, #36788, #820, #44347, #73257, #18268, #54707, #24430, #76035, #33403, #60443, #10686, #62302, #82197, #3127, #2672, #46202, #31551, #83584, #32007, #75564, #67999, #91142, #60905, #68941, #40025, #90667, #46660, #89753, #26309, #89279, #17807, #53312, #25827, #61834, #17351, #47122, #69394, #61385, #40945, #75107, #3601, #24913, #4527, #55204, #10217, #39085, #68466, #4072, #53790, #32488, #11631, #11164, #32942, #82658, #18747, #84059, #39544, #90218, #25367, #47605, #76508, #54247, #83117, #40477, #19207, #48066, #76970, #12099, #77437, #78382, #12581, #13987, #42371, #86389, #42848, #41901, #49493, #28199, #5004, #34819, #21077, #5947, #27728, #64674, #84989, #6410, #70815, #63732, #34358, #71764, #71283, #33887, #49948, #13523, #92557, #93042, #21540, #63263, #56625, #49027, #27250, #85475, #20144, #92094, #35285, #57087, #79328, #93501, #64213, #28656, #70360, #69866, #20622, #57544, #50423, #5485, #14465, #85927, #6887, #56136, #62795, #77923, #78841, #13065, #35761, #91630, #26783, #55670, #84521, #19668, #48536, #41428, #66053, #73140, #81613, #1166, #58930, #43322, #7791, #44703, #51339, #66503, #1622, #30505, #59400, #36676, #45154, #72671, #44231, #65134, #14915, #87319, #8715, #7334, #43770, #9172, #88254, #30989, #65598, #711, #22467, #59876, #30049, #29596, #66959, #2098, #80692, #80233, #51800, #235, #36214, #29115, #72218, #58011, #86867, #22021, #23412, #87780, #8266, #52278, #81157, #50891, #16301, #52730, #22930, #79772, #88716, #58475, #15369, #73604, #74053, #37146, #15846, #37592, #38050, #23864, #18163, #90113, #75919, #10578, #33296, #17237, #46099, #25265, #2567, #17705, #16762, #89634, #32378, #82557, #46558, #90559, #54142, #75004, #83011, #53201, #62194, #24804, #39914, #3485, #83472, #3018, #60335, #69289, #47016, #45616, #75457, #11525, #10116, #31446, #74517, #38982, #39441, #25717, #26193, #68357, #11044, #61279, #68835, #91024, #76403, #3963, #32837, #40372, #4418, #61727, #54601, #67895, #18628, #47494, #53690, #55087, #9652, #67440, #38537, #89172, #24324, #82079, #31904, #60796, #11989, #63624, #20969, #47960, #91985, #49836, #69757, #84412, #83956, #78733, #49386, #64569, #13876, #20029, #34710, #42729, #71644, #84878, #92449, #48426, #56980, #92933, #63154, #6777, #27612, #40838, #76864, #56509, #77808, #35654, #5838, #42260, #4888, #85368, #93394, #33772, #27138, #28546, #62685, #19560, #19105, #91518, #78278, #71174, #13416, #77331, #85818, #12464, #48906, #26674, #55564, #34248, #6303, #41311, #70248, #5383, #35171, #56023, #12958, #41796, #70707, #20518, #64093, #28094, #81044, #16187, #1057, #36566, #65946, #79210, #21431, #14353, #1977, #43213, #50305, #57437, #44588, #73021, #87208, #73492, #66390, #72114, #8603, #66842, #37032, #123, #9055, #79668, #7230, #58821, #37480, #36105, #86278, #65023, #29936, #1506, #87666, #22816, #51685, #51230, #73940, #57891, #86747, #80574, #29006, #58367, #21909, #65481, #8149, #29481, #22356, #30392, #15727, #50783, #59284, #14809, #37933, #598, #88130, #44118, #23288, #43664, #72559, #45038, #52161, #7681, #80118, #15257, #31331, #45497, #88603, #60218, #31787, #41077, #41564, #2904, #69528, #46441, #26446, #30868, #19336, #89057, #9999, #2455, #91759, #24206, #4660, #33533, #55337, #74888, #53083, #55799, #23751, #45983, #81496, #84188, #91281, #52614, #75343, #5143, #89521, #70486, #59762, #60681, #81961, #34021, #26911, #16643, #74399, #24685, #62439, #17118, #53568, #70002, #11760, #48198, #9529, #77100, #62924, #67323, #82443, #38871, #12231, #84651, #38414, #67777, #17591, #19803, #48671, #40612, #77572, #12722, #14121, #13193, #43443, #71891, #22141, #72339, #71414, #78970, #57668, #34489, #64346, #50553, #35424, #57213, #360, #20745, #35884, #6546, #93172, #63861, #7458, #7012, #63395, #79450, #42985, #28324, #28783, #51009, #92694, #86054, #78511, #56756, #21203, #49616, #27864, #64801, #86514, #15034, #29247, #93625, #58142, #6074, #5614, #50075, #86988, #79896, #34948, #43894, #21677, #36340, #85598, #92225, #13649, #14586, #42501, #65255, #27381, #56270, #85130, #20282, #49157, #78052, #42028, #70943, #8839, #17371, #30635, #88384, #72791, #37266, #74181, #80821, #2230, #31113, #22588, #37717, #23989, #66623, #59534, #67562, #87901, #9299, #73727, #44824, #66172, #74659, #45278, #7915, #52862, #16426, #1747, #60000, #24452, #1288, #23534, #51931, #30170, #52403, #23053, #59053, #38181, #88839, #82217, #2691, #81280, #31572, #73274, #36805, #67096, #60462, #53331, #8387, #65726, #81740, #9783, #15970, #837, #16890, #45747, #38658, #89297, #29719, #58601, #87442, #51463, #80352, #15493, #44364, #18286, #25385, #48084, #47142, #76052, #46223, #46681, #61853, #61404, #54725, #83601, #60925, #75127, #47623, #75584, #90236, #17829, #62322, #10704, #90684, #32960, #18765, #32507, #39562, #26327, #39105, #3620, #32028, #76526, #11649, #68017, #68958, #4545, #11182, #10237, #3146, #40042, #54265, #19226, #89772, #68484, #82679, #4089, #40496, #83135, #25844, #84076, #69414, #33420, #91162, #55222, #24934, #53811, #2067, #1593, #82051, #38507, #66026, #44675, #58903, #9620, #24776, #75431, #16273, #73577, #45583, #8686, #74975, #67411, #53659, #10087, #9142, #16730, #89146, #1138, #2540, #30958, #82528, #37565, #66476, #74488, #22901, #38019, #37117, #45124, #52701, #66929, #59846, #17208, #31419, #30475, #60308, #59371, #17676, #74025, #24295, #23835, #38955, #23379, #80662, #89606, #53171, #30020, #88687, #31876, #88223, #51772, #87749, #52248, #81582, #46069, #46529, #67867, #2990, #60765, #15818, #81129, #70216, #40343, #55054, #5350, #34216, #11494, #83923, #68803, #77298, #19529, #83440, #41279, #19075, #61248, #68330, #47929, #4389, #63122, #26162, #62652, #32349, #76832, #91951, #3454, #18595, #27106, #90083, #11012, #10549, #55990, #69724, #91487, #33739, #3932, #12428, #39882, #69260, #25235, #75886, #54570, #4855, #54109, #32806, #84845, #26641, #19993, #61696, #90528, #47461, #48872, #62163, #25688, #39414, #82982, #11959, #76368, #40807, #18132, #46986, #33266, #90992, #55531, #84380, #48395, #64994, #93362, #13845, #97, #86717, #70675, #28976, #87181, #57407, #20484, #29451, #6268, #92416, #79178, #57861, #41764, #12923, #27576, #50269, #21882, #14323, #86247, #49807, #21398, #36076, #5804, #42696, #50754, #71615, #35622, #72531, #92901, #43183, #78703, #6749, #42225, #79638, #72085, #34678, #14780, #7201, #64537, #43633, #58339, #71139, #28513 ),
 ( #7650, #36535, #64059, #56474, #65450, #566, #63592, #22330, #77776, #78245, #85333, #49350, #13382, #35136, #28060, #56950, #85787, #20938, #66813, #45472, #31762, #17085, #81016, #1943, #45954, #74860, #52136, #30841, #15698, #24178, #60191, #30363, #81932, #59735, #8120, #15231, #88577, #45012, #9972, #23725, #9496, #72990, #52588, #38844, #44087, #59252, #67751, #37006, #51655, #51201, #2877, #16618, #38384, #74372, #44560, #53057, #80541, #16160, #65919, #22786, #1478, #67297, #1031, #73463, #60654, #2425, #89491, #8575, #37453, #88098, #80089, #9030, #66362, #29909, #58793, #81469, #23258, #31305, #87637, #73913, #37908, #89029, #18475, #39762, #82868, #54926, #11841, #34107, #19420, #4276, #48282, #25125, #24652, #25576, #77185, #70093, #53999, #5235, #18961, #26528, #10897, #17562, #68688, #76253, #18021, #33154, #55417, #84269, #4740, #46874, #69611, #33620, #12314, #47335, #54458, #63009, #11382, #40233, #53541, #75777, #26042, #32701, #47814, #76715, #68216, #82415, #40692, #3820, #61587, #89971, #41158, #90419, #90879, #62045, #62527, #83329, #69148, #46414, #75315, #83808, #10433, #91369, #39298, #3336, #32225, #61134, #56841, #36428, #91840, #92782, #56355, #93712, #57755, #19884, #55883, #63944, #64428, #49241, #27951, #7096, #42586, #35513, #48755, #79061, #28867, #34569, #85682, #85217, #43073, #93254, #26995, #5694, #77660, #28408, #79535, #84736, #71027, #63478, #6633, #92307, #35967, #57299, #14674, #64887, #20829, #71501, #50164, #12812, #49698, #71977, #78594, #13736, #86601, #13274, #86141, #21291, #14212, #20370, #21770, #50646, #41652, #43530, #72427, #7544, #70569, #27463, #78136, #42111, #6160, #35030, #59622, #22673, #38270, #16509, #16974, #88921, #23140, #44906, #45839, #29337, #52022, #58231, #80908, #87075, #22224, #51093, #43980, #39648, #10787, #3226, #40583, #11271, #67644, #18850, #76137, #68571, #61933, #84158, #32117, #3708, #17910, #89859, #32593, #53891, #61013, #69041, #25928, #48167, #33502, #18367, #62409, #39189, #38739, #61483, #91251, #19306, #68101, #77069, #33043, #69498, #25019, #31652, #82758, #90315, #46762, #47227, #4629, #26415, #47708, #75663, #83689, #76607, #55305, #25468, #54348, #2769, #83222, #40124, #60542, #4170, #90769, #54811, #11731, #89380, #82302, #24535, #53419, #17453, #46303, #10321, #75207, #41530, #78479, #49584, #6513, #56235, #5583, #35851, #69971, #27349, #62892, #35391, #71379, #5111, #56721, #78935, #70909, #50521, #12200, #13160, #70456, #14086, #71857, #33989, #91728, #78020, #13616, #63362, #41996, #21171, #85567, #42469, #26881, #93136, #42951, #48638, #6043, #34454, #57181, #64311, #41043, #19769, #55767, #28291, #93592, #21643, #20714, #77540, #57634, #92193, #84621, #86021, #50040, #12690, #85098, #20248, #6978, #64768, #28751, #86477, #49124, #34915, #63827, #92660, #27832, #76135, #53417, #3706, #67642, #75661, #83220, #39646, #90313, #47706, #11269, #68099, #40122, #10319, #84156, #10785, #25926, #54346, #40581, #53889, #17451, #26413, #69039, #31650, #25466, #62407, #3224, #82300, #60540, #32115, #18365, #76605, #77067, #47225, #4168, #33041, #61931, #48165, #33500, #54809, #83687, #91249, #55303, #18848, #11729, #61011, #69496, #4627, #19304, #12198, #89378, #46301, #75205, #39187, #89857, #25017, #82756, #17908, #62890, #20712, #71855, #5109, #49122, #6976, #26878, #41528, #41041, #35849, #6511, #28289, #64309, #34452, #42949, #70454, #41994, #91726, #12688, #85096, #35389, #33987, #5581, #64766, #57179, #28749, #63360, #92191, #20245, #57632, #92658, #27347, #93590, #86475, #78477, #78018, #49582, #55765, #84619, #19767, #79418, #48636, #77538, #69969, #86019, #56719, #70907, #21169, #50038, #56233, #78933, #13158, #21641, #6041, #13614, #42467, #93134, #34913, #63825, #50519, #27830, #85565, #71377, #14084, #73693, #72304, #59021, #81243, #73241, #52822, #14552, #15458, #72758, #16390, #74146, #36305, #7424, #80319, #80789, #65690, #44330, #23500, #87869, #51896, #65221, #1711, #45240, #50978, #8352, #7879, #59498, #15938, #43409, #22109, #326, #44792, #2192, #29211, #87408, #79863, #23018, #15002, #52368, #8803, #31076, #9263, #37235, #37683, #66590, #58110, #66140, #88349, #1256, #30137, #38140, #29684, #30595, #67057, #59964, #36770, #88803, #23950, #86956, #43861, #804, #58568, #22555, #51430, #46185, #17791, #60882, #39068, #75545, #3107, #75090, #18252, #68924, #91121, #76491, #61368, #11614, #82178, #81702, #82642, #40459, #33386, #17334, #62285, #76012, #83564, #67981, #74619, #31990, #39525, #10199, #90201, #18726, #47587, #61816, #89733, #32925, #90648, #69377, #10670, #46644, #26292, #68446, #3581, #16851, #24895, #83098, #53775, #11145, #40007, #31534, #45706, #4055, #32470, #25350, #4508, #9748, #25810, #54230, #54690, #38622, #67525, #47105, #2655, #60421, #89261, #24412, #53292, #19651, #56609, #63247, #78369, #13508, #4984, #55186, #42356, #55652, #34340, #26767, #21064, #84505, #27710, #92542, #49478, #5470, #48520, #78828, #19190, #70344, #12081, #71270, #20608, #48049, #5932, #28185, #20125, #93489, #84044, #56121, #77421, #57074, #49931, #76954, #40930, #27232, #85461, #12560, #84974, #64198, #34803, #6397, #69850, #35269, #85912, #91612, #49010, #41411, #93029, #13974, #33870, #62779, #92078, #42832, #71749, #77908, #13049, #41886, #63717, #70797, #6875, #35748, #64661, #66491, #699, #8252, #80677, #57531, #87306, #73591, #58462, #80218, #23398, #43757, #58917, #29583, #22453, #86852, #30493, #1153, #86376, #8702, #66041, #51326, #51787, #74040, #22008, #15357, #7778, #79760, #44217, #72656, #50878, #87764, #15833, #38037, #52264, #37133, #81144, #29102, #28642, #73125, #16288, #9157, #57996, #66945, #22917, #59387, #14902, #21527, #36664, #30036, #65584, #44690, #37580, #1607, #50407, #88239, #45141, #79313, #14452, #43309, #72205, #7322, #36200, #65119, #222, #27005, #55893, #40703, #76264, #11854, #23851, #59862, #52717, #41663, #81599, #88703, #2084, #84279, #18972, #33164, #19430, #12324, #18030, #48293, #12824, #76727, #39774, #48765, #25585, #46884, #4751, #77195, #75786, #30974, #10906, #69623, #41168, #33631, #62541, #91383, #90890, #19894, #3829, #32711, #26539, #68699, #4286, #61596, #11391, #47825, #69159, #62055, #70107, #55426, #90429, #5247, #54468, #77671, #40243, #34117, #83820, #63019, #83338, #18484, #84747, #91851, #47347, #26053, #54940, #71040, #85232, #34581, #6174, #71515, #79548, #79995, #42600, #14227, #86155, #64901, #51109, #36443, #6649, #21306, #65358, #465, #35529, #50179, #35043, #43543, #14688, #49712, #7558, #79075, #27476, #63490, #43088, #64442, #29354, #71992, #28882, #92321, #7110, #58246, #56368, #78607, #87089, #20383, #63957, #70580, #22238, #35981, #57770, #2, #92797, #72440, #27965, #93268, #49253, #42123, #78148, #86616, #15132, #13286, #13752, #5705, #56854, #85695, #20841, #28422, #21786, #50662, #57313, #37361, #45853, #73370, #44921, #65828, #15592, #88001, #9400, #8016, #44465, #9878, #31212, #31665, #8482, #66268, #23154, #60557, #1849, #1383, #67658, #2784, #81374, #52038, #52497, #935, #36910, #29814, #82317, #58695, #87539, #43995, #60097, #59638, #73823, #88936, #52961, #22686, #24085 ),
 ( #8936, #89395, #24549, #30265, #53433, #38284, #74759, #59157, #51559, #80924, #30736, #16067, #23632, #38754, #72892, #81838, #37814, #16988, #80447, #66721, #88485, #16523, #45374, #74277, #67197, #2333, #75676, #18864, #25482, #40597, #69511, #61026, #17467, #4642, #17924, #90328, #82772, #77082, #46775, #83702, #54824, #11744, #61496, #10801, #41059, #75221, #32607, #68114, #33517, #76621, #10335, #61946, #84171, #54361, #62423, #4183, #19319, #3721, #89872, #69985, #47721, #46317, #76151, #12213, #39663, #32130, #39202, #68585, #18382, #26428, #26893, #83235, #91264, #33057, #55321, #91742, #5125, #47239, #90783, #34002, #62906, #11284, #25943, #40138, #48181, #55781, #69054, #3240, #25033, #53904, #48654, #35404, #78493, #21658, #6528, #42965, #12704, #64324, #50534, #77555, #92675, #79432, #70468, #85111, #84634, #14568, #50055, #71870, #14101, #78034, #86495, #20261, #85580, #41544, #56251, #34928, #78951, #5596, #49137, #43424, #6992, #72319, #13174, #42009, #63843, #7440, #42482, #70925, #36322, #65236, #28304, #27845, #93150, #34470, #63376, #92206, #29229, #27362, #6056, #19783, #35864, #57194, #20727, #64781, #93606, #56734, #28764, #342, #86035, #49597, #13631, #71395, #21184, #57647, #45255, #22123, #86969, #72772, #30611, #74159, #59513, #37696, #23512, #51911, #74635, #58582, #87421, #66602, #43875, #59033, #58124, #37248, #73706, #30150, #87880, #38158, #1724, #22569, #88362, #818, #9762, #52381, #66152, #81258, #79876, #50991, #15016, #2669, #7897, #36786, #65706, #9275, #8816, #23032, #67073, #2207, #29699, #31091, #67540, #16403, #51443, #38637, #80331, #15474, #59979, #88818, #44345, #73255, #8367, #23966, #52840, #81717, #16866, #45725, #80802, #1268, #15950, #44805, #54244, #82194, #10683, #31548, #46657, #90215, #39541, #68463, #90664, #83114, #3124, #47119, #39082, #69391, #75561, #68938, #25364, #83581, #53787, #75104, #40474, #76032, #89276, #3598, #76505, #67996, #17348, #24427, #32004, #32485, #25824, #62299, #61382, #18265, #11161, #40022, #60440, #4524, #4069, #32939, #33400, #53309, #61831, #54704, #17804, #46199, #10214, #18744, #60902, #47602, #11628, #24910, #89750, #82655, #53150, #38000, #74468, #44187, #2048, #82031, #80187, #30457, #17189, #8222, #22885, #22423, #46051, #81561, #9599, #45564, #15799, #24275, #51754, #23361, #73092, #87733, #66457, #16709, #15326, #80644, #74956, #38486, #10067, #44658, #73559, #1575, #38936, #74006, #8668, #67845, #2971, #30002, #60287, #88668, #31856, #89124, #88203, #30938, #67391, #51295, #81111, #2520, #52228, #9123, #60745, #37546, #52680, #16254, #45104, #59352, #37100, #23817, #66009, #31397, #59827, #66910, #1121, #58887, #54089, #25671, #68783, #46966, #83419, #10992, #82960, #26139, #76813, #5330, #84359, #69240, #19509, #90064, #89586, #90509, #48377, #41258, #25216, #70197, #83903, #91469, #75868, #82509, #39861, #47439, #18114, #4369, #26620, #55511, #69705, #3912, #40787, #4835, #77279, #18574, #54551, #34198, #76348, #11474, #24757, #32789, #90973, #61677, #19054, #47910, #39394, #53639, #11938, #40325, #33247, #61229, #12408, #62143, #55034, #33719, #62630, #17657, #46509, #75411, #10527, #68309, #3432, #32327, #28495, #27085, #13825, #36058, #28042, #7632, #63102, #64038, #27558, #64976, #28957, #84825, #55972, #35118, #35603, #20464, #92880, #72066, #42677, #6730, #19974, #50251, #79, #5784, #56932, #56453, #14305, #64518, #91930, #70656, #48850, #93344, #50736, #77755, #42205, #34658, #71594, #12904, #85769, #41743, #71119, #78685, #20919, #49788, #43165, #57388, #63572, #86230, #92398, #79620, #6249, #21381, #79157, #57843, #49331, #85315, #21862, #7183, #78225, #86697, #14762, #13364, #43616, #72512, #36987, #37436, #45455, #45934, #8556, #73895, #52117, #30820, #17067, #2408, #66345, #80999, #31288, #60174, #1459, #16142, #1011, #9478, #74355, #15677, #67278, #44994, #87163, #546, #9012, #30345, #89012, #37891, #88560, #58319, #66796, #24159, #29429, #44543, #53039, #22312, #65899, #36517, #81915, #1926, #23708, #59717, #29891, #38364, #58775, #59235, #51183, #8100, #80524, #52571, #80070, #87617, #74842, #81451, #65432, #22768, #51638, #73446, #15213, #88081, #23237, #44069, #72971, #16599, #82851, #18458, #31743, #67734, #60636, #48266, #89473, #2860, #9955, #90862, #25560, #39743, #26026, #18943, #24634, #54909, #19403, #83313, #46397, #55400, #32207, #53521, #11364, #83788, #82397, #38827, #17545, #76233, #47797, #40216, #47317, #69132, #3803, #26511, #10416, #39280, #4260, #75297, #33138, #76699, #68198, #3318, #61114, #62028, #11825, #40676, #69594, #4724, #32684, #84252, #89953, #25108, #33602, #53982, #10880, #18003, #46856, #54440, #75759, #68667, #62510, #91350, #61570, #90403, #19868, #93696, #85200, #6615, #63927, #50145, #63459, #26976, #35951, #49682, #12298, #42094, #71960, #77642, #91823, #41142, #12793, #78119, #86124, #86583, #49222, #20812, #92765, #71483, #57738, #43056, #13257, #27932, #7078, #64870, #71009, #56823, #41634, #79043, #21273, #56338, #14195, #85664, #34090, #70075, #78577, #6140, #28852, #13715, #35495, #5217, #42567, #21753, #62992, #20350, #77168, #55867, #70553, #84719, #48738, #64410, #93237, #28390, #5676, #34551, #92289, #35012, #27446, #57282, #904, #16037, #14658, #51076, #16491, #37784, #38253, #15101, #79964, #29786, #67166, #8451, #22206, #74247, #9369, #87970, #58665, #59126, #72411, #43513, #7527, #88905, #36412, #65328, #50629, #66691, #66238, #80418, #1819, #59604, #432, #30705, #60068, #30236, #87057, #2299, #72860, #44890, #87509, #43961, #31182, #29320, #65794, #58212, #73791, #8907, #7985, #1353, #23601, #15563, #79519, #36879, #51529, #22656, #52469, #45345, #44434, #73340, #37330, #23121, #52004, #80890, #88454, #81343, #61472, #74728, #11255, #54795, #60527, #82743, #82287, #69025, #25454, #52929, #31637, #45822, #90302, #11715, #62393, #3211, #89363, #32579, #24521, #61918, #54333, #40568, #90754, #89844, #3694, #76123, #81808, #17896, #4157, #53877, #75650, #18836, #39175, #83207, #25006, #46749, #17438, #25912, #18354, #16957, #33027, #47212, #10773, #40110, #69483, #46288, #39633, #32097, #75192, #68557, #68086, #10305, #83674, #47691, #33487, #76593, #4613, #24055, #53402, #9849, #38722, #67628, #2756, #60999, #44203, #86833, #682, #78814, #84143, #13960, #50391, #26864, #72190, #29567, #58447, #72642, #85899, #43742, #7763, #80203, #21513, #28628, #37116, #79295, #14436, #91236, #55752, #207, #6858, #21991, #50864, #41027, #26401, #79746, #91712, #71731, #62878, #87292, #21051, #65105, #36186, #33974, #73110, #49918, #12184, #29088, #14888, #55289, #19292, #69953, #57981, #36648, #65569, #7307, #22438, #86361, #15342, #42817, #35733, #51311, #77055, #93475, #48151, #64646, #43293, #57517, #8237, #5095, #74486, #66474, #38505, #8685, #82526, #74023, #89144, #52699, #38953, #52246, #15817, #24774, #67409, #1137, #30956, #60763, #1591, #80661, #30019, #30473, #66927, #74973, #75429, #38017, #9618, #81580, #60306, #46527, #31874, #2065, #16728, #89604, #53657, #59844, #45581, #59369, #67865, #10085, #45122, #2988, #2538, #22900, #58902, #31417, #88685, #17674, #24293, #53169, #87748, #82049 ),
 ( #51771, #17206, #10547, #66025, #9140, #73576, #46067, #37564, #44674, #88221, #23377, #81127, #23833, #16271, #26639, #68328, #4387, #84378, #69258, #90990, #34214, #54568, #69722, #40341, #11492, #3930, #33264, #62650, #84843, #32804, #62161, #18593, #90526, #26160, #83438, #61694, #4853, #55529, #48870, #63120, #19073, #91949, #39880, #39412, #55052, #27104, #19991, #68801, #77774, #33737, #41277, #47459, #32347, #76366, #83921, #47927, #76830, #70214, #5348, #19527, #11957, #48393, #77296, #55988, #40805, #12426, #3452, #61246, #90081, #25233, #54107, #82980, #18130, #46984, #75884, #11010, #12921, #95, #13380, #85785, #78243, #72529, #42223, #79176, #50267, #7199, #56948, #6266, #36533, #70673, #28058, #63590, #36074, #72083, #5802, #57405, #79636, #71613, #51199, #41762, #13843, #71137, #14778, #7648, #34676, #92414, #78701, #14321, #64057, #42694, #21880, #86245, #43181, #27574, #28974, #43631, #49348, #6747, #35134, #57859, #64992, #56472, #20482, #85331, #86715, #564, #92899, #20936, #49805, #21396, #35620, #50752, #65448, #29449, #58337, #64535, #87179, #22328, #93360, #28511, #31304, #16159, #37907, #74859, #1477, #16617, #81015, #52135, #44559, #81931, #52587, #15229, #60190, #23724, #1942, #80087, #73462, #81468, #88097, #9495, #38383, #29907, #44085, #67296, #80540, #59251, #51654, #45953, #15697, #45471, #74371, #2424, #30362, #8574, #9971, #72988, #23257, #37004, #89028, #24177, #8118, #30840, #53056, #45011, #24651, #65917, #73912, #37452, #17084, #38843, #1029, #58791, #9029, #67750, #66361, #66812, #2876, #59734, #31761, #87636, #60653, #89490, #22785, #88576, #18020, #4739, #54925, #82414, #61133, #75314, #26041, #41157, #91839, #32700, #89970, #62044, #25124, #91368, #83806, #70092, #26527, #25575, #33153, #11840, #17561, #18474, #33619, #83328, #11381, #48281, #68687, #18960, #54457, #47334, #46873, #55416, #47813, #46413, #62526, #90878, #76252, #76714, #5234, #75776, #40232, #61586, #10896, #69147, #3819, #39761, #40691, #69610, #63008, #77184, #84268, #12313, #53998, #53540, #4275, #34106, #10432, #82867, #39297, #19418, #68215, #90418, #3335, #32224, #78593, #56354, #6632, #57754, #86600, #7095, #20369, #71976, #35966, #14673, #49697, #56840, #65344, #13735, #21290, #71026, #49240, #50645, #84735, #42110, #77659, #50163, #86140, #19883, #71500, #93711, #85681, #26994, #55882, #27950, #85216, #28866, #21769, #48754, #12811, #92781, #93253, #78135, #20828, #64886, #35512, #64427, #41651, #14211, #79534, #63477, #42585, #13273, #43529, #28407, #70568, #34568, #5693, #57298, #72426, #92306, #6159, #27462, #79060, #35029, #7543, #43072, #36427, #63943, #66253, #73807, #52483, #29335, #59142, #45359, #30251, #52020, #88919, #15579, #30721, #1369, #87986, #58681, #2315, #66705, #58230, #74262, #37799, #23138, #23616, #45837, #87526, #80906, #73355, #51545, #16052, #44449, #22672, #59620, #81357, #9863, #24069, #8921, #52945, #921, #451, #44904, #81822, #74742, #29800, #38737, #88469, #31197, #80434, #87074, #8467, #1834, #37347, #16507, #60082, #16972, #9385, #38268, #67181, #22223, #51092, #79981, #15118, #43979, #72878, #8002, #36894, #65810, #93346, #6251, #21383, #79159, #5786, #91932, #43167, #49333, #71121, #63574, #57845, #78227, #64520, #35605, #84827, #13827, #86699, #13366, #12906, #19976, #42207, #92882, #7185, #7634, #64040, #28497, #71596, #72068, #72514, #50738, #36060, #28959, #79622, #14764, #48852, #77758, #34660, #38366, #74357, #44545, #2410, #16144, #22314, #29431, #44996, #59237, #31290, #81001, #23710, #87165, #73897, #60176, #58321, #73448, #89014, #51185, #65901, #65434, #24161, #30822, #52573, #88562, #58777, #67280, #1013, #66347, #80072, #36989, #15679, #59719, #15215, #29893, #53041, #81453, #81917, #87619, #22770, #8558, #17069, #23239, #51640, #45936, #74844, #9014, #37437, #37893, #44071, #72973, #8102, #9957, #80526, #1461, #548, #16601, #66798, #30347, #45457, #9480, #88083, #52119, #1928, #18460, #75299, #84254, #61116, #53523, #40218, #26028, #2862, #67736, #82399, #11366, #54911, #69134, #47319, #4262, #32686, #55402, #39282, #68200, #76235, #24636, #39745, #38829, #18005, #54442, #10882, #68669, #18945, #33140, #3320, #62030, #10418, #19405, #46858, #90864, #25562, #11827, #25110, #17547, #91352, #83790, #32209, #3805, #60638, #89955, #82853, #47799, #31745, #53984, #4726, #76701, #26513, #75761, #61572, #90405, #48268, #83315, #40678, #62512, #77170, #69596, #33604, #89475, #46399, #70077, #34092, #50631, #62994, #5219, #12300, #93239, #27934, #42096, #28392, #21275, #91825, #57284, #21755, #85666, #48740, #57740, #34553, #26978, #13717, #86126, #55869, #41144, #84721, #78579, #50147, #42569, #20814, #71485, #6142, #28854, #12795, #41636, #49684, #19870, #13259, #77644, #85202, #56825, #78121, #71011, #79045, #6617, #70555, #35497, #5678, #86585, #20352, #64412, #92767, #14197, #92291, #63461, #64872, #43058, #27448, #35014, #7080, #56340, #49224, #63929, #71962, #35953, #93698, #88907, #51531, #23123, #1355, #73793, #60070, #45347, #15565, #30238, #74249, #9371, #80420, #59128, #43963, #52471, #88456, #58667, #16493, #87972, #36414, #43515, #52006, #73342, #38255, #80892, #37786, #7529, #16039, #67168, #72413, #87511, #2301, #65330, #79966, #79521, #31184, #44892, #66693, #8909, #72862, #81345, #1821, #29788, #7987, #24057, #434, #906, #29322, #30707, #59606, #58214, #23603, #14660, #44436, #87059, #22208, #8453, #36881, #51078, #15103, #65796, #22658, #37332, #66240, #10307, #82745, #61920, #3696, #90304, #9851, #40112, #83676, #89365, #17898, #17440, #4159, #54335, #81810, #60529, #74730, #25456, #40570, #91238, #32099, #24523, #61474, #53404, #90756, #83209, #69485, #25914, #25008, #32581, #11257, #16959, #46751, #33029, #75652, #10775, #47693, #68088, #18356, #53879, #39635, #46290, #54797, #47214, #45824, #18838, #76125, #68559, #69027, #4615, #75194, #76595, #61001, #39177, #11717, #3213, #89846, #33489, #62395, #52931, #38724, #67630, #2758, #82289, #31639, #27336, #78921, #71844, #55754, #6964, #20702, #28279, #12676, #19294, #41518, #78008, #84607, #6029, #57169, #86009, #6497, #19756, #71367, #35378, #14070, #49111, #56223, #64754, #13148, #41984, #26403, #48623, #27818, #34442, #49572, #78467, #69955, #55291, #13604, #26866, #5571, #91714, #21159, #77524, #92646, #63814, #85083, #42455, #64297, #48153, #93123, #35837, #34903, #62880, #84145, #70444, #41029, #56708, #50028, #77057, #12186, #5097, #85554, #42935, #33976, #63348, #92181, #20234, #70897, #314, #29197, #8340, #79405, #790, #93579, #72746, #15447, #65678, #29672, #73680, #37221, #58094, #66128, #36293, #16378, #7867, #23005, #80308, #66579, #79850, #43396, #52355, #1243, #28738, #58553, #88336, #86944, #14541, #57621, #22096, #87397, #8791, #9251, #22544, #30125, #44316, #87856, #74133, #59483, #51418, #73228, #23488, #81231, #59009, #51883, #50966, #1699, #37670, #36756, #30582, #80776, #50507, #86464, #15926, #44780, #45228, #38129, #21625, #72291, #7412, #65210, #14989, #43848, #4047, #52812, #67516, #67042, #32917, #32458, #54220, #90192, #60412, #68916, #2646, #67970, #88792, #38613, #17323, #61358, #31065 ),
 ( #23940, #83089, #61807, #9736, #31980, #31524, #18244, #68436, #2179, #74607, #81692, #39515, #54682, #11606, #46174, #89252, #75535, #24403, #11133, #3568, #83556, #39997, #39058, #46634, #25340, #59953, #60873, #47096, #3097, #24884, #90639, #82166, #76003, #89720, #53765, #53282, #25802, #18715, #16840, #47578, #10659, #82631, #76483, #45696, #75078, #17780, #10189, #91603, #34333, #55644, #4975, #70789, #27700, #49923, #35260, #20116, #64186, #40921, #40451, #41400, #93019, #85904, #69841, #21056, #34794, #42348, #26759, #33377, #84497, #92070, #33861, #48998, #71261, #6389, #20600, #62771, #85452, #49470, #28176, #63239, #70335, #78820, #27224, #56112, #69369, #19643, #41878, #48511, #63709, #92534, #84036, #4499, #56598, #77412, #12550, #12073, #57066, #5463, #13041, #77897, #78360, #84965, #5924, #62276, #91111, #13500, #26280, #55176, #19181, #48041, #76946, #80668, #72648, #52254, #13965, #14894, #72196, #15824, #73583, #35739, #71738, #79752, #80209, #65111, #43748, #22908, #58454, #51317, #64652, #1145, #44681, #50397, #7770, #7313, #58909, #15349, #42823, #21519, #93481, #44209, #1599, #6865, #86840, #79302, #22444, #14443, #51779, #73116, #30482, #8692, #36654, #87298, #66032, #28634, #65575, #87755, #689, #29573, #37572, #29094, #8243, #37124, #30026, #36192, #66482, #59377, #57523, #88229, #23385, #86368, #43299, #214, #57987, #21999, #50870, #38513, #74981, #2546, #45591, #17683, #68337, #90535, #75895, #60772, #11019, #81588, #81135, #82057, #39889, #32813, #16736, #61703, #75437, #82989, #67417, #74031, #31425, #38961, #74494, #89612, #18139, #46993, #61254, #9626, #32355, #90090, #68810, #10093, #17214, #25695, #67873, #2996, #16279, #60314, #82534, #89152, #10555, #39420, #30964, #45130, #3460, #24301, #53178, #52707, #3939, #46075, #53665, #24783, #25242, #31882, #46535, #9148, #38026, #54116, #66935, #2073, #59852, #88693, #23841, #27586, #19536, #92907, #54577, #55538, #19082, #56483, #20492, #76375, #18603, #26648, #27114, #11966, #84387, #63600, #5358, #91959, #33747, #63130, #11501, #47468, #40350, #83448, #69267, #4396, #33273, #41772, #70223, #48402, #70682, #92424, #62170, #5812, #64067, #34224, #91001, #6275, #76839, #26170, #55998, #34686, #55061, #83930, #47936, #84853, #85341, #20003, #48881, #77784, #77305, #71146, #40814, #69731, #12932, #4864, #12437, #62659, #91493, #49358, #41288, #78252, #13390, #42233, #35144, #1835, #64543, #45838, #37348, #52484, #16053, #2317, #14329, #71622, #81823, #30722, #56956, #87987, #24070, #28519, #42704, #85793, #57414, #30252, #38269, #38738, #1370, #66706, #44905, #23617, #9864, #88920, #59143, #73808, #52946, #16973, #23139, #8922, #86253, #31198, #67182, #8468, #60083, #37800, #78709, #20944, #59621, #52021, #74743, #88470, #81358, #49812, #16508, #67643, #13851, #66254, #28067, #6755, #21404, #35628, #93369, #45360, #74263, #9386, #50277, #79185, #43189, #80907, #73356, #68100, #46761, #61932, #60541, #3225, #62408, #83688, #84157, #61012, #32116, #75662, #19305, #54347, #89858, #26414, #55304, #40123, #90768, #10786, #25018, #48166, #89379, #17909, #53418, #25927, #54810, #24534, #47226, #69497, #61482, #41042, #2768, #3707, #53890, #4628, #91250, #82301, #17452, #68570, #69040, #82757, #32592, #11730, #76136, #4169, #46302, #18849, #33501, #39188, #90314, #39647, #47707, #33042, #31651, #10320, #75206, #76606, #77068, #25467, #83221, #18366, #11270, #40582, #12199, #42468, #86476, #14085, #41995, #49583, #28290, #5110, #34914, #21170, #6042, #27831, #64767, #85097, #6512, #70908, #63826, #34453, #71856, #71378, #33988, #50039, #13615, #92659, #93135, #21642, #63361, #56720, #49123, #27348, #85566, #20247, #92192, #35390, #57180, #79419, #93591, #78478, #28750, #70455, #69970, #20713, #57633, #50520, #5582, #14553, #64310, #6977, #56234, #62891, #78019, #86020, #13159, #78934, #35850, #91727, #42950, #26880, #55766, #84620, #19768, #48637, #77539, #12689, #41529, #59022, #43410, #7880, #44793, #51431, #66591, #1712, #86957, #72305, #30596, #43862, #22556, #15003, #9264, #72759, #15939, #80790, #87409, #8804, #7425, #36771, #38141, #59499, #31077, #65691, #805, #80320, #59965, #1257, #29685, #67058, #2193, #73695, #15459, #51897, #65222, #36306, #327, #81703, #29212, #58111, #22110, #88350, #87870, #73242, #23501, #52369, #50979, #81244, #52824, #23019, #79864, #88804, #58569, #44331, #37684, #16391, #8353, #37236, #66141, #45241, #74147, #23951, #30138, #76013, #10671, #33387, #17335, #46186, #25351, #2656, #17792, #16852, #89734, #32472, #82643, #46645, #90649, #54231, #75091, #83099, #53293, #62286, #24896, #40008, #3582, #83565, #3108, #60422, #69378, #18253, #45707, #75546, #11615, #10200, #31535, #74620, #39069, #39526, #25811, #26293, #68447, #47106, #61369, #11146, #91122, #76492, #90202, #68925, #40460, #4509, #4056, #32926, #67982, #18727, #54691, #53776, #47588, #61818, #67526, #9749, #55187, #38623, #89263, #24413, #82179, #31991, #60883, #21065, #48050, #92079, #49932, #69851, #84506, #84045, #78829, #49479, #71271, #13509, #77422, #85913, #19652, #84975, #12082, #55653, #42357, #12561, #13975, #48521, #20126, #40931, #41412, #34341, #78370, #76955, #70345, #42833, #6398, #71750, #5471, #63248, #27233, #6876, #41887, #56122, #35749, #64662, #27711, #49011, #92543, #4985, #33871, #62780, #28643, #91613, #26768, #19191, #35270, #5933, #77909, #64199, #93030, #13050, #28186, #93490, #63718, #70798, #34804, #56610, #85462, #20609, #57075, #21528, #86377, #72206, #30037, #44691, #58918, #37134, #22918, #51327, #74041, #57997, #86853, #66042, #43310, #58463, #57532, #36665, #73126, #29584, #87307, #37581, #1154, #22009, #87765, #223, #9158, #65585, #80678, #44218, #30494, #43758, #7323, #16289, #51788, #50408, #22454, #52265, #50879, #36201, #79314, #79761, #80219, #66492, #66946, #15358, #15834, #8253, #73592, #38038, #23399, #8703, #1608, #81145, #45142, #59388, #88240, #14903, #2085, #14453, #700, #65120, #29103, #72657, #7779, #75446, #24790, #61713, #46543, #82998, #52718, #10564, #90547, #88704, #38971, #25705, #16748, #31434, #30975, #54588, #90100, #18150, #82067, #60784, #39900, #39429, #68346, #81600, #47003, #83459, #67427, #89622, #89161, #75907, #32364, #59863, #38523, #45603, #3473, #18615, #69276, #10103, #2555, #61265, #60324, #68821, #25251, #47479, #3951, #3006, #54127, #11032, #23852, #53675, #32823, #82542, #17693, #76388, #46085, #11512, #31891, #40359, #24311, #74505, #9636, #53189, #17223, #74992, #67882, #27597, #49824, #62669, #34234, #77315, #55548, #91969, #19546, #91503, #34696, #85353, #13862, #92917, #77793, #28079, #4874, #4405, #5367, #56967, #78721, #33758, #42716, #92433, #6286, #84397, #91012, #48412, #56007, #26659, #12943, #35157, #64078, #78263, #12449, #49370, #13401, #85805, #27124, #63140, #33284, #84863, #20014, #62179, #41297, #5822, #70233, #56494, #20501, #47946, #26180, #42245, #48892, #41781, #69742, #20955, #70692, #63609, #71158, #55071, #83940, #19093, #76848, #11975, #40823, #28533, #1045, #37020, #35640, #22344, #44576, #36551, #16174, #71633, #72547, #36091, #73479, #37468, #93381, #64557, #43651, #44103, #6765, #58808 ),
 ( #81030, #66377, #51215, #1494, #72101, #57425, #7669, #30378, #23275, #7218, #52149, #65934, #8591, #57880, #86266, #86735, #29468, #65012, #80106, #59269, #88117, #51670, #112, #22803, #80561, #21417, #585, #65468, #50292, #58356, #87196, #79198, #28992, #73008, #79655, #29924, #87652, #14341, #43200, #15714, #21897, #50770, #14796, #15245, #8137, #2890, #67763, #24669, #67309, #45484, #61147, #73925, #38400, #66824, #53555, #89503, #9042, #9984, #39310, #53069, #46887, #45026, #81944, #2439, #89982, #25136, #30855, #1963, #17102, #82427, #31317, #45968, #3348, #31775, #60667, #59749, #75329, #54012, #16630, #74874, #60204, #10444, #17577, #88589, #81482, #23738, #46426, #18034, #37920, #38857, #89042, #68228, #24192, #52601, #32239, #74383, #9512, #82879, #15549, #87954, #64854, #87043, #29772, #51061, #418, #66225, #23107, #45333, #30690, #44421, #59590, #36397, #35936, #36865, #88440, #81330, #65311, #16477, #30222, #37771, #22192, #28839, #79948, #87493, #29305, #73327, #66677, #1804, #16025, #58199, #80878, #44876, #23589, #58651, #65780, #74234, #22642, #51514, #93681, #15086, #37317, #43946, #59113, #51990, #79505, #57723, #73778, #72843, #7971, #7512, #52456, #889, #8438, #1339, #8893, #80402, #86570, #21739, #50615, #14642, #43499, #72395, #68543, #67152, #53865, #76111, #68074, #47680, #9354, #10292, #67616, #11244, #69014, #31168, #2285, #75179, #75638, #60515, #39162, #18342, #82731, #46735, #60054, #90290, #40098, #45807, #3199, #2744, #54319, #10761, #38238, #16943, #88892, #39619, #90742, #24041, #82274, #74716, #17883, #9836, #47197, #3682, #25900, #4145, #32083, #32567, #61459, #52916, #60984, #83194, #89832, #24993, #33016, #24507, #25442, #61907, #54782, #31624, #83661, #18825, #81795, #38709, #89351, #53389, #17426, #46275, #41017, #12660, #55741, #63803, #6017, #69940, #78456, #12174, #77511, #4602, #48141, #26853, #41973, #40556, #77043, #42444, #92632, #64285, #5083, #33964, #84593, #93113, #34430, #62868, #6485, #35364, #20221, #19743, #85069, #33475, #69470, #62378, #21147, #91223, #26390, #76581, #27804, #92167, #41505, #56697, #85543, #55278, #20691, #85998, #56210, #19282, #28268, #91701, #84132, #77997, #49561, #48611, #11704, #70433, #49099, #13592, #13137, #70887, #34892, #5559, #57157, #63336, #27324, #71354, #35826, #50956, #50017, #29184, #65666, #22086, #79839, #30116, #58543, #50493, #22535, #86452, #66569, #58081, #73216, #36744, #22997, #36281, #93567, #8783, #51407, #78910, #14979, #44772, #79394, #64740, #14057, #14530, #43835, #58999, #59470, #72737, #87388, #780, #44305, #30573, #15917, #7857, #29663, #73672, #37661, #80299, #15439, #43385, #51872, #87848, #86934, #80765, #8332, #6953, #42921, #37213, #66120, #1691, #1234, #88325, #71835, #28724, #57609, #21610, #72280, #7400, #65201, #304, #52346, #84361, #19056, #52803, #12410, #63104, #55036, #2637, #11940, #81681, #16830, #45687, #74595, #9724, #38603, #67507, #40789, #69242, #53272, #91471, #26622, #31516, #60404, #89242, #24395, #82156, #17312, #47441, #76350, #11476, #11648, #80941, #52059, #37833, #89413, #40495, #24567, #2801, #82336, #17005, #40962, #23649, #52515, #31684, #8953, #24101, #23176, #2352, #38771, #88954, #52982, #4544, #60578, #81391, #53455, #59659, #69884, #31229, #47622, #9897, #91161, #9418, #66739, #76988, #18764, #16086, #81855, #19225, #16539, #1865, #44938, #45394, #45874, #33419, #33904, #74780, #76525, #67675, #69413, #5023, #84075, #62321, #26326, #48083, #12117, #55221, #62811, #74294, #73839, #30757, #60115, #88502, #38305, #67220, #55686, #42387, #85491, #28673, #13539, #49964, #19684, #71299, #57558, #84537, #5962, #86403, #77454, #92112, #91646, #21557, #57103, #78855, #21094, #85008, #93515, #27266, #92575, #48553, #63279, #41917, #85943, #12598, #56153, #50441, #14005, #79344, #20162, #49042, #70830, #14479, #49508, #56641, #77937, #42865, #93059, #26800, #5501, #41444, #64229, #43337, #36230, #34836, #34374, #6427, #13081, #35776, #28215, #72234, #64689, #63747, #35303, #71779, #70376, #20638, #6901, #27745, #78398, #7348, #36692, #8281, #29612, #58490, #43786, #22945, #73158, #65148, #87796, #37161, #87335, #1182, #8732, #72686, #22483, #726, #65614, #51357, #80247, #7805, #66070, #30063, #37608, #15861, #44248, #44720, #15384, #249, #58948, #73620, #29132, #51818, #58028, #80711, #86882, #22036, #79789, #50905, #14931, #89873, #40139, #91265, #26429, #40598, #53905, #11745, #69512, #48182, #83236, #90329, #5126, #18383, #76152, #60558, #25034, #61947, #68586, #83703, #18865, #10336, #89396, #47722, #61027, #39664, #32131, #55322, #82773, #33058, #4184, #54825, #10802, #17925, #84172, #24550, #75677, #17468, #76622, #25944, #53434, #11285, #33518, #25483, #82318, #46318, #61497, #46776, #62424, #19320, #75222, #39203, #32608, #90784, #3722, #54362, #4643, #69055, #77083, #68115, #12214, #41060, #3241, #69986, #47240, #79433, #28305, #35865, #20262, #26894, #49138, #85581, #63377, #13632, #64782, #93607, #14102, #27363, #78952, #42966, #21659, #56735, #63844, #72320, #20728, #49598, #34003, #92207, #35405, #42010, #57195, #86036, #77556, #62907, #21185, #34471, #13175, #5597, #28765, #56252, #6529, #71396, #50056, #78035, #85112, #57648, #91743, #70926, #84635, #71871, #93151, #55782, #78494, #6993, #92676, #19784, #48655, #34929, #6057, #86496, #50535, #12705, #41545, #27846, #64325, #42483, #14569, #43425, #70469, #44807, #58125, #88364, #38160, #43876, #66153, #65707, #52383, #8818, #36323, #15017, #29230, #73708, #88820, #45727, #80332, #72773, #15951, #7898, #45257, #37698, #23968, #74161, #73256, #80803, #59515, #65237, #1269, #81260, #37249, #59034, #2209, #22570, #66604, #8368, #30151, #819, #9277, #1726, #343, #16405, #30613, #87881, #23514, #52842, #29700, #23033, #15475, #58583, #51912, #51444, #87422, #67075, #31093, #16868, #59981, #81719, #7441, #36787, #86970, #22124, #50992, #79877, #44346, #75106, #53789, #46201, #40476, #10216, #47121, #18267, #68940, #24912, #67998, #4526, #38639, #89752, #31550, #4071, #40024, #67542, #25366, #47604, #39543, #19206, #74637, #75563, #39084, #76507, #69393, #2671, #60442, #46659, #76034, #32006, #10685, #83583, #54246, #11163, #89278, #61833, #11630, #17350, #68465, #3126, #25826, #32941, #9764, #82196, #24429, #90666, #62301, #53311, #82657, #60904, #83116, #17806, #18746, #54706, #91141, #33402, #3600, #26308, #55203, #32487, #61384, #84058, #90217, #5946, #42847, #63262, #78381, #49026, #20143, #12580, #49947, #20621, #76969, #28198, #85474, #77922, #71282, #93500, #41427, #13064, #27249, #5484, #41900, #92093, #70359, #13522, #35284, #86388, #71763, #27727, #6886, #48535, #48065, #70814, #35760, #28655, #77436, #12098, #42370, #78840, #34357, #40944, #56135, #34818, #84988, #56624, #13986, #64673, #57086, #63731, #93041, #85926, #69865, #92556, #49492, #5003, #6409, #64212, #33886, #21076, #62794, #91629, #26782, #55669, #84520, #19667, #29595, #44702, #73603, #65133, #21539, #8714, #22020, #710, #86866, #81156, #50890, #87779, #58929, #15845, #65597, #14914, #45153, #79327, #36675, #72217, #37591, #80691, #14464, #66052, #88253, #80232, #59875, #50422 ),
 ( #58474, #38049, #73139, #79771, #74052, #9171, #22929, #87318, #30048, #43321, #7333, #36213, #234, #29114, #58010, #43769, #66502, #37145, #51338, #1621, #30504, #72670, #59399, #30988, #1165, #7790, #66958, #22466, #15368, #51799, #23411, #44230, #8265, #52277, #16300, #2097, #90112, #68356, #54141, #82556, #11524, #89171, #24323, #3484, #74516, #89633, #88715, #67894, #10577, #60795, #24803, #68834, #32377, #53200, #61278, #31445, #40371, #3017, #18162, #75456, #61726, #75003, #38536, #47493, #25264, #23863, #53689, #83471, #82078, #9651, #52729, #17236, #17704, #3962, #4417, #18627, #76402, #83010, #31903, #47015, #16761, #81612, #45615, #33295, #67439, #2566, #60334, #75918, #39440, #46557, #11043, #32836, #46098, #39913, #10115, #90558, #38981, #69288, #25716, #54600, #63623, #49385, #26192, #91023, #76863, #34709, #78277, #92448, #41795, #27611, #56022, #78732, #62684, #91517, #70706, #47959, #63153, #62193, #41310, #77807, #34247, #91984, #42259, #5837, #26673, #56508, #4887, #13875, #70247, #85367, #48905, #35170, #48425, #11988, #20968, #20517, #55086, #27137, #56979, #55563, #40837, #83955, #84411, #84877, #71173, #71643, #20028, #13415, #12957, #6302, #42728, #28093, #64092, #92932, #85817, #49835, #6776, #19104, #19559, #69756, #33771, #5382, #77330, #12463, #86277, #93393, #80117, #29480, #66389, #51229, #87665, #57436, #15256, #1505, #28545, #43663, #30391, #21430, #36104, #35653, #59283, #1056, #22815, #58820, #29005, #37479, #65022, #36565, #50304, #7229, #79667, #29935, #79209, #122, #88129, #51684, #23287, #57890, #86746, #14808, #52160, #87207, #21908, #81043, #73020, #72558, #44117, #14352, #43212, #72113, #73939, #50782, #7680, #64568, #80573, #8148, #65480, #15726, #44587, #597, #73491, #45037, #37031, #58366, #16186, #22355, #65945, #8602, #89996, #66841, #37932, #23750, #75342, #25151, #10458, #82442, #68242, #2903, #25603, #9528, #38413, #17590, #88602, #9998, #9054, #81960, #24684, #74887, #38870, #82891, #46439, #67322, #39324, #45496, #54486, #17117, #32254, #89520, #75801, #89056, #52613, #61614, #3365, #1976, #67776, #3845, #2454, #81495, #30867, #31330, #31786, #18048, #18505, #60680, #61160, #53567, #54025, #83355, #68715, #46900, #10925, #32727, #90446, #39793, #47368, #60217, #59761, #16642, #45982, #74398, #24205, #53082, #40260, #27022, #70129, #13303, #91868, #34599, #4305, #55911, #42141, #69176, #84297, #71059, #62072, #76745, #76282, #6191, #41679, #63509, #5724, #69641, #78165, #11873, #77214, #33183, #47843, #26557, #70597, #90906, #40725, #35058, #92337, #63978, #4769, #33652, #55445, #92818, #34134, #62561, #27981, #26073, #54961, #48313, #48784, #91402, #12342, #85252, #84763, #19913, #83837, #27492, #56871, #18991, #41190, #19447, #56390, #77691, #11408, #5265, #63037, #12841, #85713, #20858, #20399, #49270, #58264, #57330, #87559, #22257, #66288, #22705, #21804, #29373, #8037, #78626, #14706, #954, #79563, #7574, #44486, #64917, #80013, #50677, #43559, #14246, #51579, #51130, #13768, #29832, #87107, #72455, #72911, #1401, #43104, #36459, #28898, #7128, #65374, #20, #72011, #15153, #36932, #59175, #73390, #44013, #8500, #50193, #49729, #486, #37378, #30288, #79097, #88020, #65846, #80465, #35998, #42617, #57786, #58715, #86636, #15614, #71536, #6669, #35546, #64459, #93285, #28437, #86172, #21323, #87811, #2600, #15880, #73638, #58045, #22500, #59437, #66085, #81188, #16335, #7819, #86896, #45184, #58506, #37178, #29627, #23896, #87351, #30535, #1656, #52311, #8296, #51372, #81646, #22051, #73177, #14945, #74087, #23443, #50920, #8748, #31021, #22960, #79804, #43800, #58964, #80263, #59908, #52766, #88750, #72700, #1198, #16794, #36709, #15399, #65630, #45648, #9206, #38084, #66995, #44266, #74558, #30079, #51834, #743, #80727, #44736, #2132, #37626, #66536, #9687, #38569, #67471, #88288, #62098, #76769, #49291, #84317, #3052, #56413, #85273, #70151, #11897, #41214, #53234, #89207, #82117, #71081, #17275, #24358, #31480, #19936, #48335, #62583, #48806, #41702, #46132, #77713, #42166, #12366, #67928, #78186, #54985, #75035, #34157, #12863, #10148, #60368, #39014, #5287, #70619, #63060, #91889, #27043, #26579, #13324, #31937, #90931, #55931, #26096, #33674, #83861, #40746, #77236, #4795, #91425, #5746, #84786, #19014, #34621, #47866, #69663, #55468, #63531, #19468, #92358, #27520, #20422, #58739, #72479, #35082, #64940, #974, #6693, #20880, #64001, #35568, #7148, #15176, #15637, #72033, #43581, #21824, #511, #80489, #65866, #36023, #50699, #29855, #87582, #41, #79587, #64482, #72936, #44034, #79121, #36953, #14728, #56895, #92839, #7595, #28921, #22727, #36481, #58285, #28002, #65398, #87128, #44506, #51601, #29393, #6213, #93309, #85734, #57809, #49752, #78649, #28459, #13789, #22279, #8062, #86194, #42641, #21346, #86660, #57353, #51151, #71558, #50217, #80035, #14268, #43128, #24594, #61073, #2374, #9444, #17963, #31252, #88978, #73412, #37858, #74805, #81414, #2826, #31709, #23202, #8522, #60601, #73861, #52539, #44961, #39243, #8979, #45900, #17034, #67698, #23673, #66762, #3279, #37401, #88525, #30310, #89436, #38794, #66311, #24126, #46360, #38331, #1426, #59199, #74319, #1893, #75261, #68159, #88046, #52082, #45419, #9921, #30784, #67244, #82359, #53005, #53483, #80965, #17508, #10376, #16110, #60139, #59682, #32172, #89915, #16564, #81879, #25071, #53944, #82812, #85159, #25983, #54402, #55360, #83275, #84678, #19359, #63421, #19827, #18905, #26471, #5172, #75718, #11785, #91783, #76658, #4683, #41590, #61988, #77125, #47760, #40635, #11325, #48694, #48223, #10841, #26934, #84212, #69554, #70029, #92250, #40176, #33557, #54868, #4222, #62467, #90823, #69095, #12255, #70512, #47279, #46816, #91309, #5639, #27407, #76196, #56295, #41100, #77599, #33098, #39705, #83749, #34046, #62949, #55822, #12749, #34514, #68629, #3762, #32647, #61535, #90367, #25523, #18419, #58626, #71919, #35910, #20312, #78538, #21709, #28350, #43471, #72368, #63887, #49182, #7485, #20771, #93198, #85625, #79923, #49643, #86539, #57696, #14614, #64372, #13677, #43922, #78076, #35454, #70969, #36370, #79479, #13219, #64828, #87016, #78997, #42055, #6102, #21233, #42528, #22168, #15060, #34973, #92723, #86082, #50585, #71439, #50102, #29277, #93652, #65283, #27894, #388, #51036, #56783, #14151, #6576, #58174, #72817, #57240, #43016, #7040, #7943, #36838, #28812, #65756, #866, #29745, #1314, #31599, #60029, #10265, #60488, #59563, #67124, #45776, #22614, #52431, #38684, #23563, #45304, #82245, #8865, #24015, #88413, #81306, #51959, #89325, #88866, #51489, #67589, #31142, #16452, #16918, #39135, #80851, #74209, #66651, #44850, #9327, #37743, #15998, #52888, #74687, #3173, #17401, #2260, #46249, #81768, #75153, #87928, #87467, #38210, #68046, #32057, #23079, #80377, #9811, #24480, #73753, #15518, #1777, #2719, #30661, #53359, #44393, #73302, #8413, #37292, #66198, #30196, #59086, #83631, #90712, #5532, #18794, #76554, #60951, #25415, #62351, #68988, #84107, #19256, #10735, #89802, #48114, #61433, #40071, #32541, #26828, #90265, #33449, #4575, #55251, #11213, #54293, #84566, #24965, #76081, #17857, #77018, #26360 ),
 ( #12146, #91192, #53840, #68514, #82706, #40991, #48584, #46708, #4118, #3650, #69444, #83165, #5052, #69914, #77484, #33935, #32990, #40527, #62843, #75611, #25872, #91676, #54754, #47653, #55715, #61881, #19713, #11677, #12628, #18316, #41474, #70406, #39592, #47172, #71807, #64259, #57586, #79818, #92605, #93089, #13566, #85519, #28243, #49535, #27775, #64715, #21589, #43814, #34402, #50468, #34863, #42416, #5991, #283, #63776, #6929, #35802, #28701, #78429, #56669, #58059, #92140, #71328, #85041, #86430, #93542, #27295, #78885, #7377, #57130, #72714, #63309, #35333, #20664, #36258, #29163, #56182, #20190, #6458, #79371, #85972, #21122, #43364, #14032, #14508, #49070, #72260, #65178, #70859, #49990, #42893, #86911, #22066, #77968, #41947, #13110, #50934, #14959, #46146, #80743, #15416, #16348, #44284, #45665, #74101, #24372, #74573, #73652, #81202, #59925, #36724, #66548, #52782, #37640, #59450, #2616, #22977, #38101, #8762, #1669, #66100, #9701, #9220, #65643, #81660, #45198, #30552, #31035, #53251, #1212, #88301, #15894, #58977, #23458, #51850, #30094, #67011, #88764, #17289, #31494, #2146, #60382, #8310, #7837, #52325, #89221, #82133, #37193, #757, #23910, #38582, #87826, #29642, #44751, #16808, #67485, #58521, #87365, #22515, #51386, #80277, #73191, #26245, #62735, #4008, #11097, #19608, #32883, #90604, #75050, #39486, #76447, #83058, #4465, #33342, #24853, #67943, #91074, #84458, #54647, #17750, #26722, #3536, #89687, #11568, #62239, #39030, #10161, #53737, #47543, #55138, #40416, #83521, #69334, #68878, #91566, #75505, #10627, #18679, #60844, #75968, #3066, #54188, #25765, #47062, #39962, #84001, #19149, #68407, #48005, #46603, #55609, #18212, #76909, #61771, #12039, #61324, #82603, #33826, #40886, #31951, #69804, #4940, #32425, #90162, #25310, #48959, #49435, #57484, #57942, #20563, #85866, #64148, #42781, #29050, #14400, #78323, #92981, #43259, #72157, #13463, #28139, #13006, #21477, #86326, #27664, #79260, #57028, #5429, #12514, #21017, #42313, #7273, #49885, #6826, #70298, #78782, #36150, #41364, #56562, #65071, #34295, #77856, #48477, #170, #13923, #35700, #71698, #41842, #50355, #70754, #71222, #63202, #20079, #92495, #64614, #92032, #5887, #86797, #93440, #77376, #34757, #63672, #85415, #27187, #6349, #35222, #56074, #84927, #28594, #1099, #30435, #43707, #79712, #72606, #60263, #7728, #14854, #21955, #9100, #37522, #51727, #37977, #30916, #22862, #87711, #80166, #23794, #88178, #50828, #2024, #59327, #80620, #45082, #67367, #15304, #15776, #29980, #73069, #44634, #37079, #44163, #52206, #66885, #31374, #16686, #1552, #45541, #22401, #36609, #73536, #74442, #2496, #51273, #65529, #16232, #52658, #8200, #646, #65988, #8645, #58864, #23338, #81538, #9574, #59805, #66432, #88646, #38463, #29529, #81088, #73983, #58409, #87255, #10967, #89100, #53615, #90487, #3407, #18547, #47415, #38912, #24252, #76325, #89562, #68285, #60723, #55008, #24732, #61654, #32766, #83397, #39369, #82485, #19031, #53126, #10500, #46028, #11450, #54528, #82006, #39835, #62119, #54066, #33693, #17163, #90040, #17633, #90950, #83881, #74932, #10042, #61205, #25645, #46484, #25192, #4346, #68759, #40302, #67821, #69217, #26114, #31832, #82936, #75387, #33223, #47885, #2946, #32299, #18088, #76789, #11915, #46942, #75844, #3889, #40764, #69682, #4812, #35099, #79137, #6711, #34638, #42183, #20898, #91447, #27536, #13806, #92377, #20441, #57370, #77732, #92857, #91908, #71096, #93325, #28477, #42658, #55949, #71575, #35585, #50234, #85291, #56429, #7166, #49309, #78203, #62604, #27062, #64017, #70636, #85751, #49770, #12386, #26597, #78665, #63078, #41720, #34176, #86212, #84804, #28021, #6229, #56911, #12883, #19954, #21364, #55487, #5764, #19487, #64499, #14286, #84336, #13342, #43147, #72050, #48353, #77256, #63548, #48825, #41232, #70172, #5307, #59, #9345, #9828, #88432, #67143, #46266, #81786, #74707, #87946, #24498, #68065, #73771, #2277, #1796, #82264, #38701, #64958, #44868, #57826, #67608, #24983, #75629, #16469, #8884, #45797, #37763, #75170, #2736, #53856, #10283, #38231, #16935, #89342, #28940, #31160, #17417, #60046, #88884, #32074, #52448, #31616, #24032, #52908, #30681, #39153, #60507, #23098, #3190, #53379, #60973, #89822, #82722, #59581, #17874, #45324, #23581, #46726, #81322, #74226, #36041, #51980, #80869, #16016, #66668, #5550, #11234, #10752, #11695, #63327, #56201, #40089, #85060, #5073, #12649, #90732, #3671, #25891, #62369, #32558, #77034, #92158, #49089, #83650, #18332, #19273, #47188, #48602, #12165, #27315, #77502, #76572, #84123, #62859, #39609, #69461, #55732, #40546, #91212, #34420, #54773, #41008, #4593, #33466, #69005, #41494, #69931, #68533, #84584, #48131, #26380, #33955, #20211, #4136, #55268, #18814, #61898, #91692, #47671, #33007, #26844, #19734, #61450, #90281, #70424, #25432, #54310, #83185, #76101, #36737, #29656, #13583, #58536, #72273, #79832, #64276, #70877, #93105, #35818, #42435, #57602, #14972, #43828, #58073, #71345, #29177, #86926, #65658, #6945, #14049, #22528, #64732, #93559, #77987, #6476, #79386, #85989, #7392, #36273, #27794, #13128, #65194, #78447, #57148, #49552, #72729, #35354, #50484, #21603, #297, #28260, #21139, #7850, #41964, #50009, #34883, #22079, #43378, #6008, #28717, #50949, #42912, #63794, #92623, #78902, #71826, #772, #87381, #56687, #85534, #86445, #14523, #20681, #81216, #60397, #2160, #88778, #8324, #38596, #82149, #87840, #16362, #15909, #2630, #52796, #80291, #58991, #67499, #74588, #44765, #53266, #80757, #52338, #73205, #22990, #1684, #16824, #15430, #51864, #17304, #31509, #39045, #73665, #8776, #30565, #67956, #9235, #37654, #75064, #10175, #23926, #59463, #59939, #37206, #44297, #66114, #89702, #1227, #30109, #51400, #89235, #67024, #45213, #24388, #46161, #66562, #3081, #60859, #31049, #88315, #31966, #23472, #74115, #81675, #38114, #45681, #9716, #39501, #91089, #12054, #26260, #4480, #84016, #18695, #41379, #25325, #54205, #33357, #10641, #25781, #24869, #4026, #40432, #90619, #54663, #4955, #62255, #83073, #55154, #61342, #70313, #32899, #48021, #11585, #91582, #11112, #68422, #77392, #19164, #53751, #83536, #19624, #18227, #3552, #82617, #47078, #47558, #33841, #34311, #76463, #76926, #69350, #40901, #5444, #84474, #69821, #62750, #48492, #12529, #26739, #55625, #75984, #63217, #17764, #61787, #46618, #75519, #32441, #90177, #39979, #68894, #50372, #28154, #6841, #84944, #85881, #79276, #27203, #78338, #14417, #48976, #5903, #92049, #43274, #71714, #72172, #13021, #63688, #56090, #7288, #35715, #57499, #28610, #20578, #36166, #56577, #64164, #41857, #27679, #42327, #64629, #77872, #85430, #65087, #86343, #187, #49450, #13480, #71238, #20094, #93455, #6367, #70770, #34773, #92513, #21494, #35238, #21033, #57043, #49901, #92996, #78796, #13941, #42798, #70139, #4780, #19001, #5276, #91879, #75813, #34145, #92347, #62571, #25615, #34610, #11419, #3856, #84306, #63049, #46912, #18059, #32736, #55455, #27033, #19458, #91413, #48323, #76757, #5735, #83367, #18517, #26567, #68726, #83849, #82905, #62085, #33661, #54973, #47854, #55922, #77225, #47381, #12353, #54497, #63520, #90918, #41202 ),
 ( #76294, #48794, #40271, #84774, #19923, #77703, #33194, #69187, #12852, #10937, #4317, #39804, #41690, #70608, #61625, #27502, #90458, #11884, #26084, #40734, #69651, #36011, #14717, #85262, #21335, #7584, #86184, #14257, #51141, #71546, #86647, #57343, #28448, #20869, #58275, #28910, #20411, #36470, #30, #50204, #79574, #8049, #49741, #79108, #35557, #13778, #43115, #6680, #78638, #21813, #43570, #65855, #80025, #64929, #15165, #56883, #56401, #72021, #44023, #36942, #85723, #963, #50688, #87116, #42627, #49280, #64470, #7138, #93298, #57797, #22266, #72921, #65385, #72468, #498, #29381, #78176, #13314, #42153, #71070, #6202, #35068, #63988, #92828, #27991, #37843, #52992, #81866, #73399, #29842, #17015, #30298, #8965, #1411, #89423, #59185, #2361, #67231, #24112, #73848, #23187, #53466, #87570, #44948, #80474, #45884, #88965, #22714, #74304, #2813, #88512, #68147, #58725, #30769, #88029, #31695, #24577, #51589, #15624, #1875, #31239, #80952, #59669, #38781, #9428, #60126, #8509, #74791, #60588, #52069, #23660, #66749, #9908, #67685, #37388, #52526, #81401, #82346, #17494, #16550, #45405, #38316, #46347, #75248, #10363, #39230, #19813, #41087, #69080, #61522, #5156, #62935, #25059, #61059, #4208, #69537, #54388, #33083, #12240, #47746, #40621, #53931, #84198, #34032, #39689, #61974, #90353, #48207, #4670, #32157, #10829, #82800, #33543, #84661, #41576, #76181, #68615, #11769, #3750, #70012, #62449, #48680, #91769, #90809, #76644, #55346, #89901, #25968, #77110, #54850, #83733, #26921, #18407, #91294, #18891, #26457, #25510, #55808, #19345, #17951, #77582, #12733, #3267, #46803, #75706, #83262, #32632, #11312, #47265, #40163, #85612, #34960, #7027, #57683, #79910, #65269, #50088, #374, #70955, #70498, #71426, #29261, #22154, #6087, #51022, #64815, #72354, #56770, #63407, #20758, #28337, #63872, #78983, #7471, #36355, #50569, #92707, #21691, #79465, #58157, #93185, #6559, #15047, #57227, #86069, #5625, #27879, #71906, #78525, #93639, #28798, #20297, #34500, #86526, #49630, #13663, #42040, #87002, #42515, #43002, #14136, #14599, #35439, #64360, #92236, #27391, #21219, #56281, #43457, #35897, #85142, #49169, #78062, #13205, #82230, #43908, #44837, #38196, #45763, #30183, #36820, #59071, #1764, #73288, #23549, #74673, #9797, #24002, #37278, #88853, #52875, #31586, #66637, #73740, #72804, #30648, #59548, #7929, #8400, #45291, #51944, #67109, #2244, #87454, #65742, #31128, #44378, #23066, #15505, #38671, #66184, #16439, #81293, #60014, #87915, #1301, #67576, #851, #80836, #29732, #81754, #9313, #58613, #88399, #16905, #8852, #22601, #51476, #37730, #15985, #2704, #60475, #80364, #52418, #74195, #89311, #24466, #53346, #26344, #61866, #54739, #68032, #4560, #48100, #53826, #76066, #75596, #62338, #18778, #46236, #24949, #39120, #83617, #5039, #55701, #90250, #82692, #25857, #17842, #55237, #47637, #33919, #84093, #83148, #90697, #69430, #75140, #11196, #91178, #47157, #68973, #12133, #32524, #76540, #18299, #40056, #10719, #19242, #11663, #10251, #77004, #40511, #4103, #33434, #62828, #39576, #32974, #25398, #68499, #40978, #61418, #3633, #69900, #91662, #26816, #17387, #3159, #32043, #46694, #60937, #89785, #54278, #36244, #20177, #65162, #41934, #78415, #5979, #49057, #21109, #71793, #265, #79358, #64245, #14493, #85026, #84553, #85506, #43351, #29148, #77953, #19700, #78870, #86416, #70845, #77471, #34851, #42404, #13096, #93075, #21573, #50455, #64702, #63763, #35789, #93528, #72247, #13554, #20653, #48569, #71314, #6445, #12614, #92593, #85957, #27762, #14019, #42880, #34389, #41459, #6915, #56657, #49523, #56169, #7362, #35320, #57117, #28229, #28687, #49977, #57573, #70391, #5519, #63295, #92127, #27282, #28277, #26863, #13602, #35835, #27816, #7410, #62877, #63812, #27334, #64751, #28736, #84605, #55751, #34901, #35376, #20232, #92644, #71842, #42453, #6495, #19754, #50026, #93577, #5569, #56706, #56221, #14068, #64295, #91711, #70442, #48621, #93121, #50505, #77522, #41982, #34440, #71365, #63346, #6962, #57167, #79403, #57619, #20700, #86007, #21157, #12674, #49570, #42933, #78465, #78919, #86462, #78006, #21623, #14539, #43394, #85081, #72288, #41516, #92179, #49109, #13146, #70895, #6027, #82975, #789, #67406, #16724, #24771, #46524, #29196, #53653, #46982, #17203, #72745, #18128, #58552, #50965, #38950, #82523, #313, #65209, #79848, #10082, #17671, #67861, #46064, #2985, #31413, #54103, #36755, #65677, #74969, #22095, #38501, #36291, #45578, #53165, #9614, #2534, #75425, #31871, #29671, #60759, #7866, #75882, #74483, #89601, #24289, #10543, #22543, #14988, #90078, #39408, #58093, #60301, #32343, #87396, #43847, #86943, #51417, #89139, #68324, #81575, #82046, #3447, #61243, #25230, #85329, #70670, #40802, #55525, #5799, #34672, #11953, #84375, #69255, #77771, #19989, #83918, #41759, #19523, #61691, #68797, #48390, #4850, #63588, #26636, #63118, #32802, #77293, #92412, #3926, #19069, #27572, #90522, #11490, #11008, #56470, #70212, #91945, #34212, #4383, #12919, #40339, #69719, #25684, #76363, #55049, #5346, #54565, #33261, #20479, #27100, #49346, #62158, #90987, #47925, #39876, #62647, #26157, #83434, #18589, #12423, #76827, #41275, #47456, #33735, #91484, #55986, #84840, #48867, #22783, #65446, #93, #14319, #1027, #22326, #50264, #57857, #36531, #13378, #43179, #29446, #72081, #36072, #72986, #93358, #14776, #79174, #7197, #42692, #80084, #50750, #42220, #58335, #21878, #64989, #7646, #29905, #71611, #28972, #57402, #35618, #86712, #28509, #6745, #43629, #562, #87633, #8116, #79634, #37002, #78699, #78241, #72526, #65914, #58789, #13840, #71134, #87177, #15227, #64533, #6264, #86243, #51197, #21394, #44083, #35132, #64055, #92897, #28056, #56946, #85783, #20934, #49802, #81465, #89968, #9493, #67293, #51652, #16157, #53054, #59732, #74857, #9969, #1474, #80538, #38841, #52133, #30837, #23255, #17559, #81013, #24173, #89026, #45951, #1940, #45008, #75311, #15695, #66810, #8571, #67748, #17082, #44557, #2422, #24649, #16614, #73460, #37450, #52585, #73910, #53538, #46411, #66359, #30360, #23722, #81929, #9026, #45469, #60650, #31302, #2874, #59249, #31758, #82412, #88095, #74369, #37905, #89488, #10430, #88574, #38381, #60188, #39294, #68213, #3332, #32222, #61131, #33616, #32698, #63006, #91366, #53996, #61584, #46870, #26525, #12808, #63474, #4273, #90416, #62524, #25573, #91836, #55413, #41649, #26991, #90875, #4737, #77181, #82865, #83804, #70089, #54923, #76712, #19881, #40230, #84266, #26039, #18957, #83326, #55880, #19416, #18017, #5232, #48279, #47811, #12311, #70566, #18472, #11838, #33151, #76249, #40689, #69145, #47332, #41155, #34104, #34565, #48752, #84732, #77657, #54453, #25122, #69607, #5691, #75774, #11379, #10894, #39758, #68685, #62041, #3817, #78591, #50160, #27948, #71974, #29333, #58228, #72424, #85678, #43527, #7540, #79979, #21287, #28404, #36892, #79058, #14209, #92303, #56838, #93709, #6630, #21767, #50643, #42108, #27460, #79532, #92779, #71498, #63941, #87072, #20826, #64883, #35964, #86597, #42583, #49695, #22220, #56352, #13731, #49237, #14671, #57752, #85214, #43070, #65342, #57296, #20367, #78133, #93251, #35510 ),
 ( #449, #51090, #13271, #71023, #64425, #28864, #86138, #7093, #36425, #15116, #43975, #6155, #72876, #8000, #35027, #30718, #30249, #16969, #67178, #919, #73353, #87524, #38266, #53414, #10317, #44902, #8465, #74259, #37345, #9860, #2311, #82298, #38734, #37796, #45357, #24067, #29798, #59616, #45835, #1832, #23614, #60538, #80904, #31195, #66703, #88467, #59140, #67640, #60080, #58678, #74740, #9383, #52481, #88917, #17449, #87983, #81355, #73805, #23135, #16505, #16050, #52018, #52943, #81820, #75202, #89376, #2766, #24532, #66251, #65808, #31648, #46298, #22670, #1366, #51542, #80431, #15577, #8919, #44447, #25463, #90765, #68568, #18846, #69966, #5107, #19302, #32589, #84154, #48162, #26876, #61928, #69036, #77535, #25924, #54807, #39185, #3704, #40579, #47223, #62405, #91247, #82753, #68097, #26411, #39644, #18363, #10783, #33985, #61480, #11726, #76603, #33497, #83218, #90311, #62888, #3222, #54343, #89854, #55301, #4624, #32112, #83685, #12196, #41038, #4166, #61009, #25015, #40120, #76133, #91724, #55763, #53887, #17905, #11267, #69494, #33039, #47704, #77065, #84616, #19765, #46759, #48634, #75659, #49119, #71375, #70905, #57630, #14082, #41526, #20242, #34450, #78931, #324, #50976, #85562, #78016, #21167, #13156, #50517, #42946, #29209, #79415, #78475, #86017, #64763, #70452, #6508, #86473, #42465, #64307, #7421, #27828, #71853, #13612, #35387, #6039, #14550, #6974, #5579, #21639, #50036, #93131, #35846, #58108, #34911, #28286, #20710, #63822, #57177, #56716, #92656, #93588, #28747, #22106, #36303, #43407, #65219, #41992, #12685, #72301, #86954, #63358, #49580, #92189, #27344, #56231, #85094, #72756, #66138, #37680, #15456, #59495, #16848, #45704, #59962, #73239, #31074, #88801, #67523, #8801, #15936, #24410, #66588, #1709, #79861, #44328, #81241, #87866, #9261, #38138, #29682, #14999, #67054, #80316, #59019, #51427, #74617, #8350, #52366, #23498, #74143, #30135, #37233, #9745, #43858, #1253, #36768, #2189, #45238, #7877, #30592, #65688, #802, #58565, #87406, #22553, #23015, #51894, #23948, #88347, #44790, #52820, #81700, #80787, #38619, #89259, #16388, #73691, #31532, #2653, #60419, #54688, #40457, #17332, #82176, #67979, #25808, #69375, #83562, #32923, #18723, #47103, #69849, #53773, #82639, #61813, #39066, #54228, #53289, #32467, #68921, #25347, #83096, #33384, #90646, #17789, #47585, #89730, #4983, #61366, #76489, #40005, #26289, #39523, #3105, #12080, #11612, #46182, #18250, #48048, #46642, #31988, #75087, #75543, #76010, #62283, #62778, #11142, #4505, #4053, #91119, #33868, #19189, #55184, #84043, #76953, #40928, #91611, #10197, #10668, #60880, #24893, #90199, #68444, #3578, #77419, #84504, #71268, #20607, #57530, #42355, #78827, #48519, #6396, #86375, #19650, #34801, #21526, #12559, #27231, #26766, #50405, #85911, #13972, #49930, #20123, #28641, #56120, #27709, #41409, #92077, #70796, #21063, #70343, #84973, #79311, #42831, #14451, #49008, #77905, #5931, #43308, #78368, #13048, #72203, #7321, #64196, #63716, #35268, #41885, #36199, #92541, #93027, #28184, #71747, #56606, #85460, #65118, #5469, #49477, #34339, #6874, #35746, #63246, #57073, #93488, #13507, #55651, #64660, #1152, #58461, #2082, #59860, #22007, #57995, #66039, #66490, #51324, #30035, #9155, #44689, #37579, #50877, #81142, #30971, #36663, #58916, #87305, #45137, #1605, #29101, #7777, #79759, #30490, #81596, #38520, #73124, #65583, #8699, #697, #38035, #59385, #16746, #66942, #87762, #73590, #52262, #86849, #22916, #74038, #51786, #80676, #88701, #15356, #88237, #15831, #23395, #22452, #23849, #16286, #14900, #52715, #45601, #74503, #9633, #221, #80217, #43756, #8250, #44216, #72655, #37132, #29581, #3949, #54585, #76846, #62177, #47001, #91009, #67880, #67425, #68343, #26178, #19090, #3003, #47944, #61711, #69274, #53672, #60321, #82540, #25249, #31889, #75904, #4403, #33282, #47476, #60780, #18612, #76383, #55068, #90098, #3470, #11973, #54125, #82996, #2553, #89620, #68818, #75443, #90545, #25703, #17221, #31432, #83457, #24788, #46541, #83937, #32362, #18147, #89159, #24308, #61262, #11029, #17691, #40357, #11510, #10562, #53187, #39897, #82065, #46082, #32821, #74990, #10101, #38968, #39426, #62667, #21783, #72889, #4872, #50176, #8013, #26656, #42597, #40821, #36907, #7555, #29351, #65355, #35526, #43992, #71512, #43085, #91500, #13749, #86152, #36440, #33755, #6646, #65825, #58243, #29811, #64439, #93265, #21303, #58692, #3862, #28419, #932, #87536, #79545, #79072, #50659, #55545, #84395, #19544, #80444, #48410, #77313, #69740, #87086, #57767, #71989, #22235, #51106, #57310, #79992, #51556, #14685, #14224, #22683, #7107, #35978, #43540, #15129, #64898, #28879, #86613, #72437, #462, #2330, #9397, #31209, #52494, #24546, #23151, #52035, #38281, #66265, #59635, #15589, #1846, #74274, #88482, #23629, #45850, #67194, #80921, #60094, #16064, #53430, #30733, #24082, #45371, #38751, #8933, #59154, #89392, #88933, #73367, #81371, #31662, #44918, #1380, #8479, #73820, #16520, #74756, #17464, #52958, #81835, #16985, #9875, #44462, #67655, #2781, #30262, #87998, #37811, #37358, #60554, #82314, #66718, #87380, #22078, #36272, #22527, #15429, #93103, #51399, #15908, #79831, #42910, #51863, #28715, #21137, #7849, #80290, #64274, #35352, #50007, #72728, #44296, #36736, #14971, #65657, #296, #22989, #6943, #35816, #43827, #85987, #7391, #6474, #79385, #50948, #72272, #65193, #73204, #771, #64730, #29655, #71824, #80756, #14522, #58535, #86925, #8323, #86443, #78900, #58990, #37205, #28258, #29176, #1226, #93557, #14047, #57146, #57600, #58072, #66113, #44764, #30108, #87839, #21602, #50483, #43377, #39500, #9715, #24387, #68421, #3551, #74587, #53265, #38113, #46617, #82616, #52795, #10640, #82148, #30564, #37653, #17303, #67498, #32440, #89234, #31965, #1683, #46160, #61341, #66561, #81674, #90176, #59462, #74114, #73664, #25324, #39044, #60858, #3080, #67023, #75518, #9234, #38595, #88314, #45212, #23925, #67955, #23471, #2159, #54204, #89701, #83072, #31048, #59938, #16823, #18226, #31508, #88777, #8775, #52337, #75063, #45680, #10174, #24868, #81215, #16361, #53750, #2629, #60396, #17763, #48020, #5902, #92512, #76462, #27678, #41378, #48975, #33356, #39978, #62254, #4954, #11584, #26738, #77871, #13020, #27202, #40431, #92048, #56089, #34772, #69820, #76925, #85429, #33840, #62749, #47077, #69349, #48491, #55153, #70312, #5443, #90618, #75983, #34310, #47557, #26259, #18694, #41856, #4479, #19623, #84473, #63216, #91088, #84015, #70769, #11111, #19163, #4025, #84943, #12528, #68893, #91581, #20093, #12053, #32898, #61786, #40900, #55624, #63687, #56576, #25780, #54662, #77391, #83535, #71713, #50371, #29547, #65086, #57960, #71237, #7744, #51291, #57042, #79275, #78795, #65549, #21972, #49449, #28153, #42326, #86814, #8218, #58883, #93454, #85880, #29068, #21032, #58427, #50845, #37096, #87273, #86342, #186, #72622, #78337, #14416, #663, #43273, #72171, #15321, #35714, #79728, #21493, #7287, #13940, #22419, #14870, #13479, #80183, #43724, #36165, #36627, #66005, #42797, #44182, #28609, #6840, #73088, #64628, #1117, #49900, #29998, #6366, #57498, #20577, #35237 ),
 ( #64163, #92995, #9119, #24271, #88664, #59823, #52224, #89582, #60283, #22881, #67841, #31393, #23813, #17184, #39390, #81107, #52676, #66905, #45100, #81557, #37996, #16250, #53146, #74952, #3427, #82505, #67386, #17653, #88198, #87729, #16705, #46504, #68305, #23357, #32323, #82026, #24753, #74002, #80640, #2044, #45560, #30933, #2516, #53635, #75407, #2967, #74462, #38932, #31852, #10523, #9595, #38482, #51748, #89120, #46047, #15795, #10062, #60741, #44654, #73555, #8664, #37542, #66453, #1570, #30453, #59347, #32785, #27081, #90505, #33714, #4830, #55507, #11470, #54547, #84821, #25212, #76344, #18110, #84356, #26616, #54085, #11934, #34194, #26135, #5780, #61225, #62138, #25666, #63098, #55968, #82955, #46962, #33243, #62626, #18569, #90969, #70652, #40783, #3908, #12901, #83415, #75864, #91465, #48373, #10987, #90059, #39857, #19505, #77275, #12404, #69701, #41252, #55030, #77750, #61673, #47435, #70193, #68779, #83899, #40321, #69236, #76809, #19050, #47906, #5326, #91926, #4365, #19970, #48845, #41739, #42673, #57839, #21377, #7628, #20915, #78221, #87159, #7179, #63568, #93340, #29425, #35114, #49327, #92394, #64034, #35599, #43612, #44066, #6727, #72062, #50247, #28953, #15209, #542, #64514, #79153, #58315, #22308, #28491, #14301, #92876, #36513, #72508, #13821, #65428, #43161, #85311, #27554, #36054, #57384, #51179, #64972, #86693, #56449, #75, #80066, #20459, #71590, #72967, #13360, #28038, #34654, #42201, #21858, #50732, #79616, #56927, #71115, #85765, #86227, #6245, #49784, #78681, #14758, #65895, #8553, #67731, #89009, #89470, #66342, #37433, #52114, #24631, #59714, #73443, #31740, #60633, #45452, #80997, #16596, #29887, #1007, #58771, #46394, #87613, #22763, #8096, #24156, #23705, #37888, #53036, #17064, #51634, #81912, #80520, #15673, #52568, #1923, #38824, #81448, #60171, #44540, #74352, #2858, #1456, #16139, #53518, #30342, #59232, #36983, #82394, #67275, #45931, #31285, #88078, #9952, #23234, #9009, #44991, #73892, #66793, #2405, #30817, #88557, #17542, #74839, #9475, #38361, #10877, #25557, #91821, #33135, #46853, #5215, #34087, #18939, #54437, #83785, #3315, #39277, #32204, #19866, #61111, #68195, #75294, #62507, #90859, #11360, #91347, #84249, #89950, #26507, #84717, #54906, #18000, #26974, #3800, #25105, #76696, #55397, #53979, #10413, #82848, #47794, #19400, #11822, #40673, #69591, #69129, #55865, #75756, #39740, #4721, #68664, #76230, #32681, #83310, #26023, #47314, #40213, #48263, #33599, #61567, #77165, #90400, #18455, #4257, #12295, #62025, #41140, #70073, #62990, #7525, #21271, #77640, #13713, #43511, #49220, #63457, #12791, #78117, #49680, #57736, #58211, #20810, #86122, #64408, #43054, #29318, #14655, #78575, #93235, #72409, #36410, #42565, #28388, #13255, #21751, #86581, #27930, #79517, #57280, #50143, #41632, #71481, #65325, #42092, #92287, #70551, #71007, #6613, #50627, #87056, #35493, #79041, #14193, #71958, #48736, #430, #7076, #35949, #5674, #34549, #64868, #93694, #6138, #27444, #56336, #56820, #85198, #28850, #20348, #35010, #63925, #92763, #85662, #37783, #74246, #43960, #1818, #52928, #79963, #30235, #81807, #7984, #22655, #22205, #16956, #81342, #9368, #38252, #15562, #24054, #51528, #23120, #72859, #87508, #66237, #16490, #15100, #80417, #45821, #67165, #9848, #44433, #73339, #1352, #38721, #73790, #8450, #74727, #67627, #59603, #59125, #30704, #36878, #65793, #903, #60526, #29785, #58664, #51075, #2298, #66690, #52003, #31181, #60066, #37329, #88904, #31636, #88453, #87969, #2755, #80889, #44888, #23600, #8906, #52468, #24520, #10304, #61917, #76592, #90753, #69024, #54794, #83206, #12183, #89843, #25005, #4156, #75191, #90301, #89362, #68556, #11254, #61471, #25453, #69482, #33026, #53876, #25911, #32096, #41026, #3693, #18835, #76122, #62392, #75649, #39174, #48150, #26400, #4612, #82742, #40567, #33486, #77054, #18353, #54332, #33973, #47211, #40109, #53401, #17895, #83673, #32578, #47690, #11714, #68085, #82286, #91235, #46748, #55288, #60998, #84142, #10772, #19291, #69952, #5094, #39632, #17437, #46287, #3210, #53022, #88545, #61097, #3301, #1912, #82380, #10864, #2848, #76217, #37876, #38813, #2394, #39727, #3785, #59701, #30802, #9940, #10399, #88997, #67717, #46838, #17530, #75280, #23693, #25092, #68650, #74339, #31729, #31271, #82833, #39264, #66782, #45438, #52557, #68180, #25544, #81434, #17053, #9463, #46380, #38348, #75741, #32192, #54425, #32669, #60620, #89936, #53966, #16582, #89458, #17986, #24619, #53504, #61555, #81900, #90388, #83296, #18444, #60158, #47302, #67261, #24144, #45918, #74826, #41128, #34538, #56808, #69580, #70061, #84238, #62495, #5202, #26496, #4708, #41619, #92277, #20798, #6128, #84707, #34999, #11809, #11347, #12284, #63915, #85650, #40660, #49668, #5662, #13244, #91334, #4243, #55387, #62978, #33586, #19854, #42080, #33123, #69117, #62012, #40201, #90847, #26009, #54895, #27433, #26963, #34076, #56325, #20337, #83772, #85189, #18928, #48725, #47783, #76684, #19388, #48251, #12777, #49207, #77153, #91811, #55854, #77627, #78103, #70540, #63446, #70996, #92752, #27920, #86111, #21260, #72397, #35481, #28841, #78564, #64856, #14644, #57725, #86572, #15089, #7515, #50130, #65314, #57267, #87496, #93683, #87046, #43501, #7974, #71947, #93223, #29775, #36400, #42554, #21741, #892, #79029, #64397, #71471, #14183, #50617, #43949, #51517, #79507, #421, #29308, #58202, #13702, #58654, #22195, #51064, #22645, #6603, #79951, #72846, #36868, #28376, #43044, #65783, #7067, #35938, #26333, #33423, #20165, #63283, #6432, #85013, #27749, #91166, #49046, #35307, #62326, #77459, #64233, #55226, #69888, #69418, #93063, #34840, #56645, #92580, #62817, #71303, #5027, #70380, #84080, #40966, #19688, #63751, #19230, #33908, #28219, #85495, #57107, #91650, #26804, #48557, #85947, #27270, #55690, #21099, #49967, #13085, #12602, #77941, #4549, #5507, #78858, #14008, #84541, #48088, #20642, #76992, #41448, #12121, #34378, #56157, #92116, #41923, #70834, #5966, #49512, #78404, #13543, #42391, #30523, #65617, #72689, #81176, #729, #58493, #42868, #7351, #44252, #50908, #66073, #1185, #86406, #71782, #30066, #43340, #22039, #14482, #8736, #72237, #15387, #80251, #37164, #86885, #36233, #66524, #6904, #58031, #93518, #58951, #8284, #35779, #87338, #15868, #7808, #64692, #28677, #43789, #65151, #44724, #37613, #57563, #21560, #14934, #73164, #254, #36697, #51822, #22487, #87799, #50444, #22948, #73624, #79347, #29615, #29136, #80714, #1643, #79792, #51360, #59423, #88275, #23431, #52299, #89193, #23884, #24826, #52752, #54162, #82577, #32857, #83031, #82102, #89657, #68378, #45172, #75023, #61299, #46120, #67916, #11066, #31468, #46579, #17261, #10136, #74543, #18185, #17724, #74074, #90134, #53710, #39002, #39461, #61746, #9674, #3040, #24346, #67459, #31923, #60356, #38557, #75477, #3508, #25738, #39936, #10602, #68853, #16781, #81634, #90578, #53221, #32400, #60815, #47037, #2588, #59896, #3982, #25285, #9193, #75938, #54620, #45635, #31009, #38071, #16320, #66981, #2119, #88738, #55584, #27158, #5403, #77827, #64116, #49407, #19580, #34268, #78297, #13436, #84432, #63175, #47979, #56531 ),
 ( #92467, #92005, #56046, #40391, #70726, #20537, #26215, #48449, #76883, #34729, #84900, #18649, #91043, #11544, #20049, #71195, #28113, #62708, #55110, #48929, #83976, #27633, #12977, #6322, #85388, #77350, #41815, #5858, #47516, #12484, #63645, #41334, #70269, #42283, #4908, #35190, #92953, #83492, #12010, #76422, #69309, #4437, #33317, #62213, #19124, #40860, #69778, #33793, #91538, #26695, #15629, #52074, #73404, #22718, #88517, #45410, #67690, #52997, #37848, #81871, #58729, #57001, #59190, #17022, #9913, #87574, #38786, #52531, #60131, #44498, #1882, #81406, #8514, #51593, #45891, #20989, #37393, #13896, #16555, #23665, #49856, #8970, #31244, #23193, #2818, #85838, #88036, #80479, #88970, #24117, #78755, #42750, #30303, #30775, #66302, #80957, #67236, #66754, #59674, #71666, #74309, #74796, #93414, #16101, #1416, #9435, #38322, #6800, #64589, #35674, #2366, #29846, #44953, #73853, #39234, #40167, #68151, #69542, #4212, #48211, #4673, #3754, #11316, #83738, #60593, #90357, #76648, #61526, #83266, #26461, #46807, #61977, #32636, #25514, #89905, #33547, #33087, #89428, #11773, #69084, #54392, #54856, #77114, #25063, #18410, #10833, #82804, #47270, #75710, #53935, #90813, #18895, #41090, #55350, #25972, #84202, #32163, #31700, #76186, #19349, #12244, #61064, #70018, #47750, #62455, #17955, #24584, #39695, #40626, #68620, #91298, #53472, #82351, #17499, #46352, #75253, #10368, #3271, #27884, #34964, #43461, #56774, #20762, #5161, #63411, #6565, #13209, #28341, #57231, #48683, #34036, #86073, #5629, #78066, #70502, #64819, #34504, #71430, #49634, #92714, #35901, #78529, #21223, #26925, #13667, #93643, #62939, #42044, #28802, #84665, #92239, #91773, #57687, #64363, #50093, #78987, #27395, #7031, #56285, #6091, #55812, #85148, #49173, #93189, #19817, #20301, #86530, #14142, #21697, #70959, #63876, #85616, #50574, #42519, #35444, #79469, #14603, #43006, #71910, #77587, #12738, #41580, #378, #16909, #29267, #65273, #72358, #59553, #87919, #8404, #88403, #81297, #58162, #23553, #81758, #51949, #15051, #24006, #855, #87006, #73744, #52422, #36360, #7475, #22158, #44841, #16443, #8856, #80840, #37734, #66188, #88857, #72808, #7933, #15989, #51026, #73292, #79914, #51480, #23070, #44382, #37282, #45295, #66641, #36827, #1768, #43912, #52879, #80368, #30652, #59075, #74199, #58617, #65746, #31132, #9317, #29736, #1305, #67114, #87458, #22605, #15509, #30187, #38200, #2248, #60018, #17847, #83152, #61422, #40060, #26349, #11667, #75600, #90254, #40516, #69434, #46698, #25403, #10256, #18783, #54743, #24953, #76544, #54282, #2708, #9801, #45767, #10723, #4564, #91182, #75144, #55241, #68977, #47641, #32047, #38675, #60941, #3638, #39124, #18303, #33438, #62341, #25861, #68036, #90701, #83621, #84097, #68503, #39580, #74677, #32528, #47161, #67580, #3162, #76070, #53830, #4107, #32979, #89315, #31590, #61870, #46240, #82696, #17391, #60479, #89790, #11201, #24470, #53350, #82235, #12617, #42883, #77008, #34392, #69903, #42407, #78419, #12136, #63766, #85961, #77956, #57576, #19246, #20180, #77474, #21112, #78873, #40981, #5042, #85029, #85509, #70394, #49060, #28232, #92596, #56660, #33923, #6448, #49980, #55705, #13099, #41463, #64248, #20656, #48104, #26819, #62831, #49526, #6918, #91665, #92130, #84556, #27765, #19703, #57120, #13557, #35792, #14022, #41937, #71317, #35323, #48573, #70849, #93078, #5982, #34854, #71796, #63299, #64705, #93532, #28690, #5522, #27285, #56172, #21576, #66540, #30084, #22505, #15884, #38089, #50924, #51376, #747, #43804, #80267, #7823, #79808, #22965, #73642, #2136, #81192, #66089, #16338, #86900, #51838, #8752, #31025, #45188, #1202, #74091, #22055, #86420, #87355, #9210, #66999, #72704, #50458, #80731, #88292, #36713, #79361, #29631, #44271, #58510, #58968, #23447, #52315, #1660, #15404, #37631, #30540, #14496, #73181, #8300, #43354, #37182, #87815, #72250, #44740, #59441, #7367, #36248, #65166, #271, #29152, #58049, #60372, #39018, #31484, #25753, #89211, #32414, #3523, #54177, #10151, #53239, #83507, #23900, #75039, #16798, #83047, #25299, #52771, #10616, #32872, #24843, #4451, #59912, #60831, #24362, #61760, #54634, #81650, #45653, #31941, #61313, #17279, #89675, #68867, #39474, #90151, #74561, #47051, #90593, #2604, #53726, #82121, #11084, #18199, #88754, #67475, #9691, #75953, #47532, #38572, #67933, #46136, #68393, #3056, #3997, #39951, #76436, #18665, #82592, #11557, #40405, #17739, #46593, #69323, #75492, #84913, #28126, #48463, #63658, #34281, #5416, #91552, #35206, #5873, #62227, #13449, #70739, #63189, #56546, #78769, #26709, #92019, #12498, #84445, #27172, #77363, #55597, #57015, #56060, #77842, #19594, #6336, #42299, #41350, #64134, #12990, #83990, #91057, #41828, #20062, #92968, #48943, #85402, #55125, #34742, #85851, #26231, #70283, #21004, #19137, #33809, #33330, #49870, #92481, #20550, #49420, #27647, #13910, #62722, #78310, #47992, #4923, #71209, #42764, #76896, #71683, #12025, #40873, #69791, #65056, #36138, #50816, #23324, #58398, #72145, #30424, #59315, #44150, #79700, #15293, #28580, #64602, #57471, #45072, #86313, #93428, #6814, #87699, #22390, #36598, #22851, #15764, #21465, #51717, #16221, #80154, #43247, #52195, #29037, #50340, #8186, #80606, #79246, #35688, #14388, #73056, #44624, #37068, #65977, #1088, #633, #81077, #7261, #158, #29969, #57927, #7714, #86784, #14842, #51262, #72593, #65514, #73526, #58854, #21943, #8635, #43695, #29518, #87244, #37512, #66422, #1540, #88165, #23783, #32756, #46472, #9088, #38901, #68748, #74431, #88635, #37966, #9561, #74920, #82925, #83387, #46016, #17621, #89551, #68274, #54517, #39824, #10031, #24718, #3878, #53603, #73972, #38449, #75376, #81995, #3396, #32286, #52647, #66874, #61192, #67356, #53115, #45530, #61644, #2486, #10489, #39357, #90029, #24240, #31363, #90477, #2010, #89089, #30903, #25181, #54055, #59794, #82474, #46931, #67810, #18537, #81527, #2935, #60252, #75834, #25634, #16674, #17150, #31820, #18078, #60712, #10957, #56421, #91898, #84794, #4336, #34629, #78195, #83869, #12375, #11905, #92366, #48816, #76314, #54996, #69207, #19945, #35090, #85743, #26587, #19021, #55939, #47875, #85281, #77721, #64009, #20431, #19476, #27052, #5755, #11440, #41222, #27528, #77245, #5296, #42175, #62591, #12872, #48343, #70160, #40754, #49300, #41711, #40291, #13334, #70628, #34166, #63540, #92847, #69671, #63068, #55477, #4803, #71088, #91435, #33683, #6221, #28011, #56903, #47403, #33213, #62108, #76778, #90940, #26104, #84326, #66319, #50225, #1434, #15185, #22736, #7157, #13797, #36032, #72487, #79129, #518, #51609, #80498, #982, #14276, #65873, #29863, #8530, #43591, #50707, #59208, #7603, #14736, #64949, #43136, #51158, #8071, #30318, #15646, #29401, #44515, #21354, #20890, #21832, #73420, #49762, #72041, #78657, #44044, #37409, #50, #42649, #28930, #36490, #57817, #58293, #71566, #6701, #58748, #86668, #87590, #35575, #64491, #65407, #79595, #93317, #87136, #22287, #28469, #80045, #72946, #36960, #57362, #86204, #37866, #88054, #75271, #88534, #67251, #59691, #53955, #23682, #60609, #31718, #82369, #38338, #81423, #17975, #52091, #9452, #44969, #17519 ),
 ( #80974, #52547, #82822, #10388, #75729, #16572, #45427, #2382, #10852, #45908, #74327, #46827, #39716, #89446, #31261, #2836, #16118, #73870, #8987, #32657, #66770, #1902, #23211, #39253, #9929, #24134, #68168, #3289, #30792, #32181, #3772, #67707, #60148, #68640, #88987, #53012, #24605, #61084, #81888, #17042, #74814, #53493, #89925, #38803, #46369, #25081, #85975, #21125, #12632, #61545, #49993, #63313, #41950, #34406, #28703, #92144, #35336, #6462, #57133, #13114, #56186, #86432, #25534, #77972, #19717, #78888, #28246, #54414, #13570, #35804, #27779, #7379, #90378, #63780, #27299, #64717, #57588, #84570, #48588, #34867, #64262, #20194, #92609, #71809, #42420, #93092, #77488, #14035, #93544, #5535, #56673, #85045, #42896, #6931, #41478, #70410, #49073, #21591, #50470, #70863, #5994, #85522, #71332, #20667, #79373, #14510, #43366, #72262, #49539, #78433, #88303, #65180, #1213, #81204, #66101, #87827, #31037, #51387, #66550, #37194, #8311, #758, #38103, #8763, #284, #16350, #73653, #30095, #59452, #81662, #29643, #58979, #15417, #87366, #22978, #80278, #58522, #1672, #23460, #45667, #59927, #15895, #88766, #36725, #36260, #51851, #23912, #16810, #65644, #74575, #30554, #67013, #22516, #29164, #44285, #80744, #73192, #44752, #2148, #52784, #45200, #37642, #74103, #9222, #58060, #52327, #86912, #22067, #50935, #79819, #14960, #43815, #72715, #7838, #38584, #17292, #31496, #75971, #91077, #48008, #82605, #46148, #18215, #75052, #47546, #11100, #26248, #76450, #75507, #83061, #61774, #67487, #68410, #54650, #39487, #61327, #4468, #24855, #39965, #10629, #3539, #67945, #11571, #68881, #2618, #83524, #47065, #32428, #32887, #55141, #3068, #90165, #17752, #60846, #25313, #53739, #31953, #4011, #90607, #19152, #33345, #25768, #62242, #10163, #9703, #54192, #84004, #60384, #39032, #89223, #18682, #40419, #89689, #24374, #46605, #69337, #53253, #82135, #13926, #42784, #57031, #70301, #28142, #85869, #64617, #5890, #13009, #21480, #34760, #92498, #76912, #41367, #78326, #84930, #6352, #35225, #26726, #12042, #64151, #77379, #56077, #48480, #71701, #12517, #49438, #20566, #71225, #27190, #5432, #6829, #40889, #92035, #33829, #92984, #42316, #69807, #27667, #49888, #41845, #4943, #62738, #77859, #34298, #78785, #35703, #91569, #55612, #48963, #13466, #63205, #70757, #21020, #56565, #93443, #84461, #28597, #57487, #19611, #63675, #86329, #85418, #20082, #14858, #23342, #59331, #29533, #81092, #1103, #7276, #14403, #29984, #44167, #16236, #65992, #8649, #72160, #58868, #45086, #43262, #58413, #73987, #36153, #50832, #50358, #9104, #15780, #37526, #73540, #43711, #52210, #79716, #51277, #65075, #21959, #650, #44638, #174, #72610, #37981, #66436, #66889, #7732, #36613, #87259, #2028, #8204, #65533, #30919, #59809, #87715, #22405, #22866, #29054, #57946, #86801, #88650, #80170, #15308, #79263, #1556, #51731, #73073, #30439, #88182, #37083, #80624, #33226, #3410, #60267, #69220, #46032, #38467, #25195, #10970, #81542, #52662, #67371, #90043, #39838, #54069, #32303, #82939, #17637, #40305, #24256, #53130, #61208, #9578, #24736, #23798, #2951, #39373, #89566, #53619, #3892, #18091, #82010, #46945, #89104, #4349, #31837, #75847, #10504, #90489, #10047, #2500, #76328, #68762, #16690, #82489, #18550, #17167, #31378, #45545, #74937, #46488, #32769, #62122, #75391, #61657, #68289, #25648, #74446, #83400, #54531, #47418, #11453, #38917, #67826, #60727, #84339, #92860, #26600, #91911, #19034, #62607, #41235, #56431, #55011, #91450, #56913, #78206, #78668, #55490, #19490, #70175, #13809, #48828, #48356, #20901, #49773, #34641, #5310, #5767, #47888, #83884, #76792, #35588, #11918, #40767, #90953, #13345, #12886, #27065, #42186, #6232, #69685, #71099, #6714, #70639, #33696, #42661, #77259, #4815, #92380, #35102, #12389, #26117, #34179, #63551, #64020, #27539, #85294, #20444, #84807, #71578, #63081, #55952, #49312, #19957, #77735, #41723, #28024, #85754, #36501, #65417, #44527, #72955, #64960, #36971, #7168, #80986, #72497, #87601, #51168, #37420, #50720, #14288, #23221, #65885, #93328, #29413, #59219, #61, #79139, #28479, #28942, #528, #73431, #73880, #58304, #8083, #80055, #58759, #44979, #30329, #87147, #15195, #88064, #52101, #22297, #44055, #57828, #66331, #8541, #43601, #1444, #994, #21366, #57372, #29875, #22747, #16128, #51622, #80509, #86214, #15657, #8998, #50236, #7614, #64502, #43149, #86678, #72052, #36043, #21843, #79605, #14746, #7581, #16545, #87113, #79570, #66294, #52065, #28905, #26, #14713, #37384, #80947, #1406, #44491, #30293, #58721, #81397, #65381, #493, #73395, #50684, #65851, #64923, #44019, #80470, #36937, #959, #44944, #8505, #29377, #59181, #36466, #45401, #72916, #88025, #51584, #37839, #51137, #43566, #23655, #23182, #57793, #29838, #59665, #58271, #72462, #86643, #22263, #87565, #73844, #74300, #22710, #16092, #15619, #8960, #9424, #30763, #66745, #1871, #88508, #52521, #21810, #80020, #15160, #8043, #47262, #17490, #69077, #82795, #88960, #2357, #17947, #32153, #4205, #53927, #90349, #60121, #46798, #33080, #31235, #46342, #61969, #24107, #38777, #38311, #90806, #3746, #25505, #61518, #31689, #40160, #67681, #39224, #52988, #9903, #82342, #32628, #81862, #2807, #25965, #54383, #54846, #60584, #89419, #75244, #83728, #89897, #24573, #18888, #47743, #75700, #10359, #10825, #17011, #45880, #74786, #76641, #53461, #68142, #67226, #83259, #39685, #3263, #18403, #76176, #61054, #25055, #68609, #11308, #26454, #69534, #12237, #12729, #20754, #21213, #77578, #49166, #27388, #6083, #86063, #71422, #41572, #56278, #6554, #35433, #70494, #85137, #70008, #78521, #49625, #84657, #42510, #20292, #62445, #4667, #78059, #5622, #64355, #13201, #63869, #33540, #42037, #93181, #91288, #19809, #28333, #55343, #41084, #11766, #57223, #70951, #92703, #34957, #5151, #13658, #34028, #34497, #84194, #77106, #55805, #27873, #19342, #62932, #50083, #56766, #40618, #91766, #26918, #48677, #48204, #63403, #92232, #85607, #8847, #22595, #58151, #87449, #7021, #42995, #35892, #23543, #64810, #71901, #78978, #66179, #846, #15042, #1296, #87910, #93634, #30178, #88392, #58608, #21686, #30643, #7466, #28791, #80359, #59062, #57678, #14130, #86521, #51470, #23061, #15500, #44371, #73282, #72799, #1756, #79460, #14594, #8395, #50563, #79904, #43451, #86997, #29727, #51017, #43902, #51939, #37273, #72348, #80829, #36349, #59542, #22149, #15980, #65735, #44832, #65263, #369, #37725, #73735, #29255, #7923, #36814, #66631, #24942, #9791, #82225, #61412, #3154, #89779, #9308, #39571, #83143, #88848, #17379, #16899, #3628, #53819, #81288, #60008, #74189, #82687, #40050, #90692, #31581, #23997, #60932, #52870, #90244, #17837, #68967, #25393, #24461, #32037, #10714, #16434, #46231, #32516, #75135, #10245, #47152, #67570, #46689, #53340, #39114, #45757, #54273, #75591, #45286, #18294, #68493, #68027, #76061, #4097, #74667, #11190, #60470, #38666, #32968, #2699, #89305, #61861, #52413, #38190, #67104, #2238, #31122, #81749, #25852, #26809, #78409, #71308, #55231, #6438, #20171, #27755, #12126, #18773, #40972, #77465, #84086, #5513, #56651, #85500, #5972, #19236, #70839, #34845 ),
 ( #20647, #70385, #76535, #83612, #34383, #19693, #49517, #41453, #77946, #47631, #63288, #13548, #11657, #33913, #42397, #40504, #26338, #49051, #35313, #69894, #69423, #5033, #12608, #48093, #92121, #64238, #54734, #63756, #76997, #92586, #4554, #33428, #48562, #55695, #62332, #27275, #56162, #91172, #62822, #85019, #91656, #13090, #41928, #84546, #93069, #80257, #93522, #72241, #64696, #58957, #28681, #65624, #36703, #87344, #43344, #86410, #22954, #57111, #14486, #49971, #22493, #58499, #85951, #43794, #66079, #58038, #37619, #28223, #259, #57567, #1191, #87805, #21103, #78863, #65156, #736, #50449, #29142, #8290, #72694, #29621, #14013, #15393, #30072, #35783, #86890, #21566, #44260, #51366, #42873, #6908, #71786, #73171, #80721, #79351, #7356, #36238, #7813, #22044, #37171, #51828, #15874, #44730, #50913, #73631, #8742, #79797, #14939, #17730, #2594, #24352, #61304, #81640, #3046, #67465, #38563, #31015, #68383, #39008, #1649, #46585, #10142, #31474, #89664, #18190, #59902, #60362, #45641, #23890, #89200, #16787, #88744, #31930, #53716, #75943, #90140, #46126, #25290, #66988, #66530, #53227, #54168, #47042, #2126, #11073, #52759, #82109, #75483, #17268, #67922, #23437, #82583, #3514, #9199, #75029, #74550, #10608, #60821, #30529, #74080, #88282, #24833, #83037, #59431, #9681, #38077, #39466, #32406, #52305, #81182, #16328, #45178, #13320, #20876, #93305, #68858, #6209, #86190, #71077, #92835, #36018, #56408, #71552, #42160, #35077, #5742, #43124, #13785, #3987, #21342, #78645, #63996, #64477, #86655, #34617, #27998, #20418, #92354, #56890, #85269, #63527, #6689, #28455, #50695, #64936, #49748, #37, #41697, #39942, #85730, #28917, #21820, #70615, #79582, #35564, #72028, #27514, #32862, #49286, #42636, #78182, #57350, #7144, #57805, #50212, #79116, #14264, #61751, #90583, #25744, #54625, #83497, #18655, #47522, #76427, #12859, #16105, #22722, #37855, #66759, #58281, #14724, #1888, #15172, #87578, #80031, #74316, #44030, #80961, #52078, #8975, #58735, #8057, #38327, #72475, #29851, #65393, #30780, #73857, #7591, #59194, #81411, #73408, #53002, #43577, #15633, #72931, #16561, #9440, #36477, #506, #80484, #44957, #29389, #51597, #45416, #87123, #36949, #22275, #67241, #59679, #88522, #23670, #65862, #2371, #970, #44502, #51147, #8518, #37397, #52536, #66307, #1422, #31249, #60136, #88975, #30306, #88041, #23197, #24123, #39701, #53479, #11781, #40631, #25520, #61069, #90363, #9918, #45896, #38791, #26467, #67695, #74801, #81876, #69092, #3759, #17960, #4218, #90819, #2823, #33093, #91304, #61532, #24590, #33553, #10373, #31705, #83272, #61984, #60598, #17030, #89433, #54399, #25978, #18416, #47276, #76192, #75715, #4679, #82356, #17504, #11322, #46357, #82809, #75258, #89912, #32644, #53940, #46813, #54863, #40173, #39240, #83744, #68156, #62462, #25068, #18901, #68625, #47756, #3276, #32168, #69549, #76654, #10838, #20307, #50098, #55818, #70024, #19355, #84674, #56291, #64368, #64824, #27403, #92719, #70965, #49639, #35906, #21229, #85154, #6097, #78992, #14147, #49178, #34969, #19823, #28346, #93194, #34510, #86078, #63883, #12250, #48219, #27889, #78072, #43011, #56779, #13673, #77121, #85621, #71915, #63417, #12744, #13215, #70508, #48689, #20767, #42523, #93648, #7036, #78534, #55356, #77594, #84208, #42051, #41096, #5167, #41586, #34042, #71435, #57236, #5635, #62945, #92246, #6571, #35449, #91779, #26930, #59559, #8862, #22164, #73750, #37740, #16449, #51486, #58623, #67120, #80374, #44389, #28808, #87012, #30193, #36833, #51955, #80847, #72364, #57692, #15995, #29272, #7940, #384, #88409, #58168, #1311, #66195, #23076, #72814, #51032, #52428, #86535, #43919, #79475, #44847, #87925, #21703, #73298, #1774, #87464, #50580, #14609, #29742, #79920, #30658, #23560, #43467, #7481, #861, #59083, #15057, #22611, #66648, #8410, #81303, #36366, #45301, #74206, #65279, #15515, #65752, #9323, #38206, #37288, #9806, #24011, #68509, #83627, #40522, #75149, #38680, #10730, #67585, #40065, #3644, #18789, #68983, #68042, #75607, #54288, #31138, #60947, #47167, #32053, #53836, #90707, #17396, #32535, #3169, #89797, #60484, #4113, #61428, #60025, #76076, #39586, #24960, #25409, #47648, #89321, #82702, #90260, #17853, #83159, #76550, #24476, #46704, #10261, #53355, #18311, #46245, #82240, #11207, #32985, #11673, #25868, #61876, #54750, #2715, #2255, #88862, #52884, #81764, #31595, #16914, #45772, #74682, #39131, #62347, #55711, #27291, #5048, #49066, #6453, #35328, #49531, #62838, #20660, #78424, #57125, #92136, #5528, #14027, #56178, #85036, #69440, #33930, #70855, #77480, #92601, #27771, #19252, #4570, #56665, #69909, #48580, #40988, #64254, #91671, #41943, #13106, #63772, #19709, #26824, #93083, #33444, #84562, #26355, #85514, #34859, #91188, #20186, #42412, #34398, #55246, #84103, #70401, #12623, #71323, #28238, #48110, #77014, #41469, #5987, #63305, #77963, #13562, #85967, #21117, #12142, #49985, #78879, #79366, #7830, #7372, #87821, #44277, #71801, #50463, #64710, #15410, #30547, #81198, #22060, #14502, #51381, #43359, #80737, #73186, #59446, #15889, #14954, #22510, #1207, #6923, #36719, #22971, #72709, #752, #37636, #58054, #8305, #43809, #65639, #36253, #44745, #37187, #35797, #51843, #30089, #88297, #65172, #72255, #86905, #23453, #29636, #277, #66544, #1665, #80272, #50929, #66095, #93537, #28696, #57581, #42888, #86426, #21581, #29157, #58973, #58515, #87360, #73647, #8757, #79813, #52320, #25759, #89682, #52777, #61766, #38578, #31031, #17745, #3530, #74097, #45194, #59919, #82598, #32420, #46599, #24849, #75499, #10157, #32878, #16804, #45660, #53732, #2142, #17285, #16344, #89217, #31947, #82128, #46142, #90157, #10622, #74568, #39480, #81656, #90599, #24368, #68401, #3062, #83053, #2611, #88760, #68873, #61319, #9216, #75045, #11091, #9697, #23906, #38096, #67481, #39025, #25305, #54641, #67939, #54183, #60839, #18206, #67006, #75961, #47057, #39957, #4003, #31490, #60378, #53246, #55132, #20072, #84921, #40880, #77850, #19602, #76442, #18672, #48470, #91559, #12999, #84452, #63196, #11563, #77370, #41836, #47538, #69798, #70747, #40411, #91067, #83515, #63666, #56068, #48952, #5881, #4932, #92489, #12033, #12507, #62234, #76903, #26716, #34751, #4460, #33818, #27657, #69329, #62729, #55603, #92026, #83996, #41358, #33337, #70291, #27181, #5423, #34288, #26239, #19144, #47999, #46892, #17107, #90897, #82432, #3837, #61152, #47357, #60672, #24197, #33173, #75793, #9517, #39316, #69167, #74879, #89048, #38405, #9989, #75334, #83346, #83828, #46431, #18040, #89987, #68707, #54950, #40251, #10450, #25141, #4294, #62063, #68233, #54017, #38862, #76273, #18493, #53560, #11399, #82884, #31322, #67314, #10915, #3354, #26061, #39783, #32719, #2444, #61604, #18982, #60209, #17582, #74389, #53074, #67768, #81950, #45973, #90437, #25594, #54477, #2895, #31778, #89509, #32244, #24674, #19438, #91860, #13295, #11863, #48303, #13761, #35050, #35537, #12333, #77203, #27014, #64451, #5716, #41178, #71525, #6659, #85243, #55902, #56377, #69632, #40713, #4760, #86163, #33641, #62550, #47834, #63966, #63499, #77681, #92807, #56863, #91393, #27973, #57322, #27485 ),
 ( #84755, #71050, #6183, #26548, #76736, #85705, #70118, #19903, #5256, #42609, #34125, #20391, #49262, #42133, #48775, #63029, #93277, #55436, #12833, #84288, #20850, #49721, #41671, #92329, #78617, #70589, #34591, #78157, #28429, #79556, #23167, #80934, #43096, #79085, #87099, #87549, #72448, #51119, #30277, #65838, #58706, #72001, #8492, #52050, #57779, #80005, #14697, #66280, #22696, #50187, #28890, #7120, #51571, #8947, #59651, #476, #86625, #29824, #21795, #59167, #80457, #37826, #88013, #22249, #946, #73382, #14237, #15144, #1393, #44005, #72903, #16079, #36452, #15604, #8027, #36923, #43552, #44932, #44476, #35989, #73833, #37370, #66732, #1859, #30749, #7567, #21315, #29364, #65367, #64909, #58256, #11, #50670, #75689, #4195, #83248, #68128, #18394, #88948, #88496, #89407, #47251, #40150, #24095, #69066, #82784, #90340, #74772, #81385, #9890, #46330, #52974, #3252, #25495, #54373, #68598, #81849, #39676, #16999, #61040, #32142, #17936, #38765, #45866, #76164, #52509, #67669, #45386, #46787, #53916, #16533, #39213, #61508, #53447, #33070, #23643, #24561, #2795, #11297, #74287, #9411, #38297, #60571, #89884, #31677, #82329, #3734, #25044, #10814, #67211, #32618, #2344, #31223, #17479, #75233, #60108, #10347, #90796, #69524, #83716, #34485, #49612, #6542, #41073, #4655, #70482, #33529, #6070, #63391, #78507, #34943, #34017, #41559, #20277, #25955, #26907, #13189, #91755, #19798, #56751, #77096, #92221, #62920, #55795, #26442, #63857, #27376, #54836, #42024, #5610, #84647, #85126, #13645, #55333, #48667, #69998, #19332, #77568, #12226, #84184, #56266, #49152, #71410, #85594, #78048, #20741, #62435, #61960, #12717, #42496, #18877, #91276, #47733, #70939, #92690, #48194, #76632, #5138, #27860, #11756, #40608, #67446, #2574, #16767, #28778, #81618, #45621, #24330, #59406, #66508, #75010, #88259, #52283, #35419, #93620, #38056, #44709, #59882, #88722, #78965, #64340, #23870, #35879, #15851, #7007, #31452, #52736, #66965, #16307, #2103, #30510, #53207, #64796, #57662, #45159, #21198, #37598, #93167, #73610, #81163, #8720, #1628, #74523, #74058, #86509, #9178, #71885, #82085, #23418, #9657, #30995, #38543, #21672, #14116, #89178, #60341, #28319, #17243, #46105, #51806, #50069, #57208, #80698, #86049, #42979, #19567, #75924, #47500, #25723, #4424, #84419, #69764, #39920, #54607, #4895, #33779, #11050, #83478, #68363, #76870, #19111, #83017, #40845, #18634, #60802, #67901, #76409, #3969, #62692, #11531, #62200, #31910, #40378, #91525, #3024, #18169, #26681, #89640, #10584, #10122, #55571, #69295, #91030, #33302, #3491, #11996, #39447, #68841, #24810, #75463, #54148, #26199, #53696, #32384, #48433, #55093, #38988, #61285, #90119, #47022, #82563, #61733, #25271, #17711, #46564, #83962, #32843, #47966, #90565, #41318, #5390, #21916, #34255, #70255, #77337, #64577, #92940, #13423, #93402, #86286, #63161, #28554, #86754, #56988, #20036, #29013, #5845, #91992, #78740, #57445, #27145, #12471, #56030, #49844, #35662, #84885, #42268, #21439, #71181, #35178, #72121, #92456, #13884, #78285, #49393, #41803, #79218, #42737, #48913, #50313, #20977, #6310, #6785, #57898, #70714, #64100, #56516, #34717, #28101, #27619, #63631, #71652, #14360, #77815, #7237, #85826, #36112, #12964, #85375, #43220, #65030, #20525, #130, #2462, #45046, #52621, #37039, #43671, #65953, #8611, #80125, #30399, #81503, #16650, #30875, #44124, #1984, #59769, #38421, #73499, #80581, #89064, #37487, #66397, #50790, #15264, #52168, #58828, #73947, #9062, #605, #14816, #37940, #51237, #29943, #22363, #45504, #73028, #23295, #88137, #66849, #1064, #8156, #74406, #72566, #87673, #7688, #88610, #16194, #36573, #1513, #9536, #15734, #65488, #29488, #51692, #22823, #67330, #31338, #58373, #87215, #44595, #81051, #59291, #60225, #33190, #68722, #61621, #74895, #11415, #54968, #60688, #82899, #82450, #69183, #25610, #53089, #31794, #45990, #90453, #11880, #62567, #3373, #89528, #54493, #24692, #62080, #83361, #40731, #90913, #90003, #3852, #47850, #81968, #39331, #10006, #47375, #18511, #17124, #76289, #26079, #18055, #24214, #38877, #25158, #17598, #83844, #18997, #67784, #2910, #54032, #40266, #75350, #46907, #76752, #4312, #69648, #53575, #4776, #33658, #46448, #75808, #10465, #68249, #32261, #61167, #10932, #39800, #63984, #79103, #36005, #70603, #5271, #6197, #34140, #35552, #92824, #14252, #64465, #63515, #71065, #49735, #26563, #56396, #42623, #27498, #49276, #86178, #12847, #27987, #92343, #85258, #55917, #93292, #56878, #55452, #71542, #35064, #20406, #20864, #43110, #84769, #78171, #5730, #48790, #13309, #41685, #19918, #85719, #78632, #7134, #21329, #13774, #50199, #91874, #91408, #42147, #72017, #84303, #27028, #19453, #6675, #28443, #77698, #48319, #34605, #57336, #77220, #12348, #41197, #70135, #63043, #67379, #26495, #55386, #62977, #4242, #11346, #19853, #33122, #90846, #9113, #38475, #76683, #82019, #4707, #33585, #23807, #37989, #62494, #74454, #53139, #45554, #41127, #9587, #47782, #18927, #69579, #24264, #2509, #54894, #91333, #66897, #40200, #84237, #69116, #62011, #70060, #89113, #11808, #76216, #47301, #31386, #77152, #40659, #2037, #19387, #48250, #26008, #12283, #26962, #60276, #83771, #18443, #5201, #34075, #91810, #55853, #84706, #30927, #59817, #88658, #52670, #81551, #16699, #48724, #49667, #7514, #420, #78102, #29307, #43043, #50616, #34998, #41618, #63914, #6602, #13243, #28375, #79506, #14643, #28840, #42079, #93682, #57724, #36399, #71470, #78563, #87045, #35480, #64396, #77626, #70995, #50129, #56807, #71946, #7066, #92276, #12776, #35937, #49206, #27919, #20336, #43500, #6127, #21259, #86110, #64855, #92751, #85649, #72396, #70539, #20797, #5661, #86571, #14182, #34537, #93222, #21740, #13701, #63445, #27432, #42553, #57266, #65313, #58201, #56324, #85188, #79028, #88442, #73329, #51992, #31170, #66679, #59592, #72845, #9356, #52918, #58653, #80880, #80404, #67154, #23591, #51063, #29774, #43948, #52458, #9838, #60517, #1341, #87495, #30692, #22644, #60056, #81332, #38711, #88894, #87956, #1806, #81797, #16945, #2287, #15551, #24043, #45809, #67618, #44878, #16027, #22194, #73780, #37773, #79950, #44423, #16479, #30224, #45335, #74236, #65782, #15088, #38240, #51516, #59115, #8440, #74718, #37319, #2746, #31626, #7973, #66227, #23109, #36867, #891, #8895, #46277, #18827, #54784, #53391, #40100, #62380, #54321, #33966, #89353, #90292, #53867, #91225, #55280, #17428, #82276, #61461, #61909, #46737, #25444, #4604, #69016, #33018, #75181, #76583, #26392, #32085, #83196, #82733, #40558, #90744, #24509, #3201, #10294, #25902, #77045, #39164, #68545, #60986, #4147, #89834, #33477, #83663, #12176, #84134, #18344, #47682, #11706, #68076, #47199, #69472, #76113, #11246, #19284, #10763, #48143, #41019, #69942, #17885, #5085, #24995, #75640, #39621, #3684, #32569, #86000, #14532, #27326, #92634, #41975, #20223, #56699, #77999, #56212, #93115, #50019, #72282, #57611, #42446, #86454, #63338, #62870, #63805, #21612, #43387, #92169, #7402, #57159, #64742, #49101, #55743, #13139, #20693, #85071, #13594, #28726, #50495, #27806, #71356, #70889, #35828, #71837, #6019, #93569, #6487, #19745 ),
 ( #79396, #5561, #85545, #34894, #14059, #64287, #91703, #70435, #84595, #35366, #26855, #48613, #49563, #34432, #28270, #78458, #6955, #21149, #77513, #12662, #78912, #42923, #41507, #65203, #1236, #81224, #66122, #87850, #31058, #51409, #66571, #37215, #8334, #782, #38122, #8785, #306, #16370, #73674, #30118, #59472, #81683, #29665, #59001, #15441, #87390, #22999, #80301, #58545, #1693, #23481, #45689, #59945, #15919, #88785, #36746, #36283, #51874, #23933, #16832, #65668, #74597, #30575, #67033, #22537, #29186, #44307, #80767, #73218, #44774, #2169, #52805, #45221, #37663, #74123, #9244, #58083, #88327, #52348, #86936, #22088, #50958, #79841, #14981, #43837, #72739, #7859, #61797, #53274, #9726, #90629, #10183, #40442, #83546, #3089, #54673, #18704, #91101, #32449, #39509, #48031, #61352, #25334, #38605, #67964, #11122, #17773, #32909, #25791, #82158, #67509, #47568, #39052, #82625, #75071, #69359, #31974, #75993, #47089, #4037, #53759, #60867, #33366, #2639, #24877, #60406, #76474, #68905, #31518, #54213, #11594, #68430, #89244, #24397, #10651, #89710, #4489, #62267, #17314, #46168, #75528, #39988, #46628, #3560, #26270, #83082, #55164, #90186, #84028, #19173, #18237, #41868, #41390, #28167, #78349, #12064, #84485, #4967, #49461, #64641, #21507, #56101, #19634, #85441, #48503, #21045, #13491, #93469, #49913, #48987, #56588, #35251, #40911, #70781, #57057, #13033, #34784, #71726, #92060, #42338, #77886, #5914, #70323, #78808, #71250, #69831, #85893, #20591, #63699, #6379, #28622, #5454, #92525, #84956, #34322, #27691, #27214, #63228, #64176, #93008, #86356, #6853, #13954, #35728, #77403, #76936, #42811, #57511, #33851, #12540, #62760, #91594, #26749, #20106, #55635, #36641, #8231, #79740, #30012, #81120, #22894, #79288, #30466, #87742, #80197, #73568, #2058, #14882, #15336, #29559, #7756, #44197, #65562, #43736, #80654, #37555, #59836, #45113, #58896, #74015, #50858, #50385, #51304, #9132, #30948, #72636, #88678, #44667, #52238, #675, #43287, #58440, #37109, #87286, #51764, #16263, #38009, #59362, #22432, #1584, #88214, #66920, #73103, #66018, #14430, #1130, #15809, #72184, #8677, #66467, #23370, #7300, #36180, #199, #65099, #29082, #57973, #86826, #21984, #83429, #53159, #90073, #61238, #18123, #67855, #17198, #47450, #81570, #38945, #74478, #46976, #82970, #16718, #68318, #90517, #82518, #62153, #23826, #24766, #82041, #25681, #18584, #45573, #9609, #89595, #25225, #74965, #53648, #32797, #3442, #54098, #38496, #11002, #54560, #60296, #17666, #46059, #68791, #75877, #52689, #31407, #67401, #39871, #11484, #2529, #2980, #89133, #32337, #24284, #61686, #3921, #40334, #76358, #46519, #69250, #4378, #10077, #75420, #33256, #10537, #39403, #31865, #60754, #27567, #91940, #63112, #55520, #92892, #47919, #20474, #56464, #55044, #41753, #64049, #55981, #35613, #90982, #27094, #84369, #28051, #56941, #19064, #83912, #84835, #63582, #48385, #19984, #6259, #70665, #34668, #76822, #78235, #85778, #33729, #48861, #19518, #42215, #92407, #26150, #4845, #11948, #85325, #78694, #40797, #70207, #62641, #5794, #91479, #35127, #49341, #13835, #20928, #77766, #13374, #71129, #69714, #12914, #49797, #42686, #71605, #6740, #12418, #26630, #77288, #41269, #5340, #34207, #36997, #93353, #44552, #8110, #556, #87628, #16151, #28967, #29439, #43624, #21871, #58329, #79630, #57852, #1022, #51647, #73905, #59244, #44078, #88090, #64984, #64528, #65441, #23248, #45003, #87, #9021, #58784, #66354, #50746, #57396, #14771, #22321, #86706, #72980, #1469, #30355, #73455, #72521, #15687, #8566, #52127, #87172, #51192, #28504, #80079, #15222, #86238, #7641, #65908, #36525, #22778, #80533, #14314, #21390, #37445, #29900, #81008, #36067, #50259, #79167, #43174, #72076, #7192, #81924, #31297, #61579, #1935, #53049, #53991, #47326, #17554, #74364, #83321, #60183, #52580, #39289, #25117, #30830, #66805, #81460, #10425, #82860, #68208, #46406, #3327, #31753, #54448, #38374, #67288, #75306, #23717, #38836, #37900, #17076, #53531, #9964, #67743, #18012, #32217, #2417, #61124, #9487, #18467, #45944, #89963, #24643, #10889, #24168, #16609, #90411, #46865, #59727, #2869, #32693, #89021, #45464, #88569, #74852, #60645, #75769, #76242, #89483, #39752, #82407, #68678, #3813, #25568, #41150, #55875, #71017, #35021, #12306, #84727, #69602, #78127, #20359, #84261, #42102, #19876, #62036, #69140, #48746, #5226, #6149, #26986, #63468, #33146, #77650, #63935, #4268, #19411, #92773, #90870, #11833, #11374, #27941, #70561, #92297, #34559, #4732, #13265, #40684, #70083, #26034, #76707, #55408, #5685, #54917, #33610, #56832, #27454, #85672, #62518, #91359, #48274, #20820, #63001, #26520, #49690, #40224, #12801, #77176, #41643, #83797, #18952, #47806, #34099, #91831, #56346, #85208, #49231, #1702, #15929, #67045, #88794, #71492, #37673, #50154, #9738, #38614, #23491, #59012, #88339, #6623, #42577, #35503, #24405, #64419, #93245, #78585, #2182, #30585, #44783, #31068, #23942, #28398, #59956, #89254, #59486, #21281, #31526, #8343, #57290, #81234, #52814, #86132, #13724, #79052, #52358, #81694, #16381, #45231, #74136, #73684, #2648, #14203, #44319, #9254, #73231, #80779, #37226, #87859, #38131, #51886, #8794, #16842, #45698, #66131, #74609, #1246, #60414, #23008, #67518, #66582, #30128, #39517, #3099, #12076, #25804, #82168, #18246, #48044, #53767, #67972, #17325, #82633, #54223, #62279, #62774, #25342, #90642, #68917, #47580, #33863, #19184, #83091, #4049, #76949, #40924, #47098, #32919, #17783, #26283, #91114, #32460, #84039, #61809, #10191, #46176, #54684, #76005, #69845, #83558, #11608, #75081, #18717, #4978, #39060, #61360, #91606, #31982, #46636, #53284, #60875, #76485, #40453, #69371, #75537, #55179, #10661, #11135, #89722, #24886, #3570, #4501, #68438, #90194, #39999, #33380, #14446, #84967, #56115, #70792, #43302, #35742, #36195, #92537, #64189, #42351, #21059, #7317, #86371, #56601, #71264, #21522, #50400, #27703, #6392, #20118, #93484, #64656, #5927, #57526, #35263, #77415, #84500, #93022, #20603, #79305, #28180, #78823, #48514, #57069, #72199, #19646, #34797, #65114, #12554, #27227, #26762, #55647, #85907, #13968, #49926, #49002, #28637, #77900, #85456, #41403, #92073, #63712, #42826, #70338, #13044, #5465, #71741, #34336, #41881, #49473, #78363, #63242, #13503, #6868, #23844, #52710, #37575, #73119, #8695, #22002, #57990, #50873, #38516, #79755, #86843, #217, #81138, #15827, #30029, #16282, #9151, #14896, #45133, #9629, #73586, #36657, #45595, #22447, #43752, #1602, #74034, #72651, #29097, #7773, #66486, #38029, #30485, #59381, #88232, #87758, #16739, #692, #29576, #23388, #65578, #1148, #58457, #8246, #44684, #66035, #58912, #66938, #52257, #87301, #2077, #51320, #74497, #37127, #30967, #80671, #59855, #80213, #15352, #81591, #88696, #44212, #22912, #51782, #67876, #82060, #31428, #2999, #68340, #62173, #31885, #67420, #3463, #26173, #19085, #60775, #47939, #61706, #69270, #53668, #60317, #82537, #25245, #89615, #46996, #4399, #33277, #47471, #24786, #18606, #76378, #55064, #90093, #32358, #11969, #54120, #82992, #2549, #17687, #68813, #75440, #90538, #25698, #17217, #89155, #54580, #46538 ),
 ( #10558, #24304, #91004, #32816, #83451, #11504, #39423, #83933, #61258, #18142, #53181, #38964, #75898, #40353, #46078, #11022, #76842, #74985, #10096, #39892, #3943, #84856, #57418, #92427, #12441, #64548, #93373, #78255, #20007, #49361, #62662, #4867, #91496, #79189, #26651, #33750, #40817, #28071, #56486, #70685, #56959, #49815, #55541, #85796, #50282, #20494, #77308, #86257, #63133, #84390, #42236, #20947, #19539, #69735, #48405, #13393, #78712, #71149, #6278, #35148, #34689, #21408, #41291, #70226, #64070, #5361, #34227, #91962, #92910, #28523, #27117, #48885, #56001, #13854, #77787, #42708, #71625, #12935, #6758, #41775, #35631, #5815, #63603, #27590, #85345, #87188, #15238, #59260, #7658, #58800, #58347, #22337, #14788, #66369, #1038, #43193, #44567, #65926, #51208, #22794, #52143, #79646, #80098, #65459, #72539, #44094, #36543, #43642, #87645, #80550, #16167, #88108, #8128, #30370, #50762, #14333, #72999, #81023, #45019, #575, #72093, #15706, #23265, #29459, #65003, #37012, #29916, #51662, #73470, #7210, #36084, #105, #8582, #28984, #57871, #86726, #37460, #1487, #21890, #56795, #20784, #5186, #63434, #6588, #13232, #28362, #57254, #48708, #34060, #86097, #5651, #78089, #70525, #64841, #34526, #71452, #42540, #93210, #49194, #92262, #28826, #62962, #20324, #55836, #21246, #64385, #91796, #49656, #71932, #63900, #43485, #26947, #6114, #27419, #7054, #93667, #84691, #19839, #70982, #35466, #56308, #34985, #14165, #78551, #50115, #77611, #79011, #35923, #41603, #92735, #85173, #43029, #57709, #86553, #21723, #12762, #42067, #27907, #50599, #79492, #14627, #13688, #85637, #66209, #88876, #72830, #7956, #80862, #58186, #73313, #72381, #51500, #87939, #44405, #8424, #52441, #16009, #36850, #44861, #15072, #24025, #80388, #1789, #59098, #45315, #87478, #22179, #31153, #73764, #7498, #37303, #67136, #65767, #51047, #36383, #877, #1325, #81316, #81778, #23091, #8876, #51972, #66662, #52900, #38222, #37755, #30673, #2270, #60039, #59575, #88425, #29756, #74219, #16462, #15531, #9338, #23574, #29290, #65296, #16928, #401, #79935, #43933, #22627, #67601, #25425, #76565, #9821, #53850, #11688, #31609, #46259, #45788, #40539, #11226, #33000, #68998, #39146, #47664, #75163, #46719, #2729, #17411, #89814, #40081, #38694, #10276, #69454, #61891, #33459, #68057, #3183, #24976, #62362, #3662, #32067, #4585, #91204, #83177, #82716, #54303, #60499, #89335, #24490, #84116, #53371, #82256, #74699, #90724, #61444, #75622, #25884, #54765, #60963, #83642, #55261, #18326, #17867, #26372, #10745, #39603, #68526, #32551, #90274, #47182, #76093, #4129, #18806, #28253, #28710, #85053, #56681, #34875, #13577, #93552, #78895, #49081, #63787, #14042, #42904, #20203, #92617, #77495, #85982, #57141, #92151, #50001, #27787, #69924, #77028, #85528, #13121, #71818, #20675, #71339, #41001, #49546, #6938, #12157, #27307, #35811, #5065, #19726, #19266, #64725, #78441, #6469, #42428, #12641, #21132, #48595, #77980, #33947, #84577, #63320, #35346, #62852, #41487, #57595, #64270, #48124, #70417, #5543, #56194, #91686, #70870, #34413, #26837, #55725, #93098, #41957, #6001, #14518, #50478, #43373, #31044, #72268, #79381, #86439, #73660, #8319, #22523, #8771, #1678, #7387, #37649, #2154, #66109, #29172, #38109, #14967, #36268, #87834, #66557, #65188, #21598, #292, #58986, #30560, #22985, #1222, #51859, #80285, #9229, #86921, #22074, #30104, #58067, #87376, #50944, #65652, #37201, #58531, #51395, #59458, #80751, #79827, #15903, #43823, #67019, #766, #44760, #73199, #88309, #72723, #7845, #45208, #23467, #36732, #29651, #52333, #15425, #44292, #81211, #16357, #74110, #88773, #39974, #3547, #89697, #83068, #11579, #24382, #24863, #39040, #17299, #53746, #75059, #53261, #90172, #47072, #69345, #54657, #39495, #83531, #60392, #59934, #60854, #18690, #40427, #89230, #4475, #54200, #61782, #46155, #52791, #10170, #17759, #82143, #68417, #90614, #25775, #68889, #67951, #11107, #4019, #47553, #82612, #46613, #23921, #75514, #10636, #81670, #3076, #61335, #31960, #18222, #75979, #9710, #16818, #32894, #32436, #25320, #31504, #76458, #45676, #74583, #38591, #67494, #2625, #26733, #57038, #91084, #48487, #84011, #56572, #92506, #26255, #77866, #6360, #92044, #71709, #33352, #34306, #91577, #35233, #92991, #55149, #19159, #5439, #5898, #84469, #63212, #42322, #13016, #70765, #48016, #20573, #64158, #69814, #27198, #55620, #78333, #34768, #62249, #40896, #76921, #63683, #21028, #12049, #12524, #4950, #41852, #33836, #71233, #27674, #49896, #28149, #56085, #85425, #49445, #62745, #84937, #13475, #20089, #48970, #85876, #78791, #13934, #19619, #42793, #77386, #41374, #70308, #1564, #21968, #37091, #7740, #72618, #65082, #8657, #73082, #35710, #80632, #44175, #36621, #29993, #52218, #182, #65543, #79724, #57955, #658, #50841, #29063, #66000, #87723, #16244, #30447, #80178, #59339, #7283, #6836, #29542, #88191, #81101, #36161, #45094, #1112, #37535, #86810, #93450, #14866, #58422, #43720, #15316, #66446, #23351, #15788, #87268, #51739, #44647, #64624, #22414, #51286, #28605, #8213, #58877, #57494, #22874, #73548, #86337, #21487, #50367, #79271, #14411, #43269, #72167, #12045, #4471, #92501, #62245, #5435, #70304, #27193, #76915, #26251, #56568, #90610, #48011, #83527, #56080, #92038, #25771, #77382, #5893, #91572, #71228, #32890, #33832, #91080, #34763, #27670, #54653, #18685, #4946, #34301, #84007, #62741, #41848, #12520, #63208, #47549, #20085, #63678, #69340, #26729, #55144, #77862, #84933, #61777, #40422, #76453, #48966, #20569, #11574, #40892, #33348, #41370, #69810, #70760, #13012, #49441, #85421, #55615, #84464, #78329, #19614, #48483, #13469, #42319, #36616, #7279, #72163, #64620, #8207, #72613, #35228, #80173, #43714, #36156, #29536, #51734, #93446, #65078, #79266, #57490, #177, #21483, #28600, #65537, #87262, #15783, #1106, #79719, #29987, #6832, #6355, #29057, #58871, #80627, #35706, #44641, #653, #37086, #86332, #92987, #50362, #57950, #14406, #14861, #65995, #87718, #15311, #43265, #51280, #44170, #22869, #86804, #21962, #64154, #50835, #7735, #28145, #58416, #22408, #73077, #57034, #85872, #49891, #21023, #78788, #13929, #42788, #71704, #39376, #9107, #46035, #17171, #67829, #23801, #66892, #3413, #37529, #88653, #30442, #2954, #38920, #66439, #24259, #46491, #38470, #18094, #73543, #74449, #37984, #75394, #68292, #1559, #59334, #45548, #74940, #30922, #9582, #82492, #53133, #10050, #88186, #60730, #10507, #16239, #67374, #2032, #24740, #31840, #8652, #81095, #23345, #89569, #61211, #52213, #52665, #45089, #82013, #73990, #17640, #53622, #90046, #32307, #2503, #25198, #54072, #59812, #82942, #81545, #31381, #16693, #60270, #89107, #75850, #54534, #68765, #19493, #35934, #86568, #26121, #83403, #55494, #18553, #86108, #48359, #64852, #21257, #19037, #26603, #5313, #10973, #11921, #91914, #76795, #4818, #43041, #62125, #77262, #47892, #40770, #11456, #50127, #12392, #39842, #27068, #84342, #69688, #70179, #93679, #40308, #33700, #55015, #4352, #62611, #90956, #69223, #41238, #34182, #57721, #71943, #63085, #7064, #47421, #46948, #91453, #28837, #3895, #76331, #32772, #55955, #79026, #33229 ),
 ( #14180, #83887, #61660, #90492, #25651, #51059, #87953, #59111, #16024, #65779, #15085, #45332, #79503, #36864, #72393, #44875, #80877, #14639, #66224, #88439, #80401, #60053, #21737, #22641, #79947, #23588, #81329, #43497, #7510, #87491, #23106, #72842, #51513, #30689, #1338, #51988, #36395, #8892, #16476, #888, #73777, #15548, #44419, #43945, #52455, #37770, #50613, #1803, #66675, #73326, #59589, #67151, #7970, #8437, #29771, #58650, #37316, #30220, #74233, #9352, #38237, #31167, #2284, #65308, #416, #22191, #29303, #58197, #87041, #40554, #24505, #69468, #83192, #90740, #75177, #81794, #10290, #46733, #53387, #68541, #25898, #54780, #69012, #82271, #40096, #4143, #76579, #17881, #24990, #33473, #75636, #10759, #88891, #17424, #90288, #3197, #18340, #47195, #38708, #24039, #76109, #89349, #68072, #60514, #83659, #46273, #61457, #32565, #11242, #39160, #32081, #18822, #52915, #60982, #45805, #33014, #54317, #16942, #39616, #61905, #53863, #74715, #9835, #89830, #82729, #47678, #11702, #67615, #2743, #3680, #25440, #4600, #31623, #71352, #13135, #6015, #19280, #49559, #93111, #5081, #27322, #26851, #13590, #63801, #91221, #69938, #84130, #34890, #50015, #6951, #41503, #33962, #70884, #62866, #6483, #92630, #78908, #35362, #34427, #41971, #20689, #26388, #56208, #42442, #92165, #20219, #27802, #55275, #56695, #64283, #85067, #62376, #48139, #63334, #55739, #28266, #57155, #77041, #12172, #49097, #85541, #19741, #77995, #85996, #78454, #21145, #41015, #14055, #42919, #91699, #71833, #84591, #48609, #77509, #12658, #70431, #5557, #8330, #23478, #74120, #14978, #43384, #44303, #72279, #73670, #37211, #52344, #8781, #7856, #15437, #87846, #64738, #779, #80763, #65665, #87387, #30571, #50955, #66118, #36743, #29662, #303, #37659, #1232, #93566, #15915, #73214, #58542, #58997, #81221, #29183, #22534, #43834, #86933, #51406, #79838, #58080, #30114, #22995, #45218, #59468, #51870, #88323, #36280, #35824, #80298, #16367, #28723, #65200, #57608, #44770, #66567, #22085, #86451, #72736, #1689, #21609, #50492, #79393, #14529, #7399, #2635, #54210, #83079, #90626, #31971, #39049, #47565, #60864, #24874, #9241, #67505, #10648, #17310, #32446, #61349, #52801, #38119, #90183, #9722, #82154, #74593, #68902, #38601, #75525, #46625, #3557, #53270, #31514, #32906, #67030, #24393, #59942, #25331, #39506, #88782, #18234, #39985, #45685, #67961, #60402, #47086, #68427, #2166, #16828, #31055, #75990, #25788, #23930, #46165, #89240, #17770, #75068, #11119, #4034, #54670, #61794, #10180, #82622, #83543, #81679, #3086, #18701, #89707, #53756, #71247, #91590, #13030, #77400, #48500, #40908, #78346, #48984, #11591, #56585, #20102, #12536, #5911, #28164, #69828, #41387, #55632, #33848, #70320, #26746, #4963, #41865, #63696, #85890, #6376, #56098, #35247, #76933, #76471, #5451, #64173, #57054, #12061, #21042, #70778, #13488, #62757, #69356, #84482, #34319, #19631, #84953, #42335, #93005, #85438, #63225, #27687, #20588, #40439, #92057, #27211, #4486, #77883, #34781, #33363, #92522, #49458, #62264, #91097, #26267, #55161, #84024, #19170, #48028, #29077, #21503, #15804, #79284, #22428, #87281, #44193, #195, #43283, #73564, #13951, #65095, #6850, #73097, #15332, #42807, #671, #22890, #14878, #88209, #49910, #50854, #14425, #51760, #44663, #71723, #35725, #21980, #51300, #7296, #79736, #58892, #29555, #64638, #78805, #37105, #65557, #43732, #66014, #87738, #93466, #1126, #59358, #58436, #86352, #1580, #72180, #28619, #80193, #30007, #57508, #50380, #36176, #8227, #80649, #8673, #37551, #66462, #72632, #30462, #57968, #86822, #7752, #36637, #24280, #23366, #2525, #38941, #89129, #53155, #3438, #31861, #23822, #89591, #59832, #39866, #31402, #46515, #10073, #90069, #9604, #66916, #75873, #24761, #52233, #82037, #18119, #52685, #38005, #81116, #81566, #17194, #32332, #32793, #46055, #60750, #67850, #17662, #3917, #82966, #74961, #2976, #46971, #10998, #53644, #82514, #16714, #25221, #61234, #60292, #54094, #75416, #74011, #16259, #10532, #39399, #68787, #68314, #61682, #45109, #9128, #2053, #30944, #88673, #45569, #74474, #38492, #67397, #27563, #55977, #77761, #19980, #83908, #92403, #26145, #91475, #18580, #62149, #40793, #84831, #54556, #90978, #56459, #12910, #78231, #55039, #19060, #69710, #13370, #48381, #47915, #20470, #49337, #34203, #4841, #5335, #47445, #83424, #76354, #35123, #11480, #26625, #48857, #42211, #76818, #55516, #33725, #11944, #84365, #62635, #19514, #27090, #41748, #6255, #85320, #70202, #71125, #77284, #90513, #12414, #25677, #40330, #41265, #69246, #70661, #4374, #63108, #33252, #91936, #5790, #34664, #63578, #1018, #29896, #44074, #57392, #15218, #72976, #51643, #86702, #83, #8562, #21866, #79626, #64045, #28500, #65437, #72071, #87168, #22317, #13831, #92886, #51188, #64524, #43170, #35608, #58780, #93349, #36521, #7637, #58325, #14309, #86234, #87623, #28047, #79163, #20924, #80075, #29434, #56937, #14767, #36992, #28962, #85774, #49793, #64980, #21386, #65904, #22774, #78690, #42682, #36063, #552, #50255, #57848, #8106, #43620, #80529, #71601, #15683, #44548, #6735, #50742, #7188, #73451, #72517, #66350, #44999, #59240, #9960, #25113, #75765, #16605, #73901, #45940, #9017, #75302, #38832, #53987, #10421, #9483, #17072, #89479, #1465, #2413, #82402, #67283, #89017, #32213, #52576, #67739, #38370, #31293, #1931, #39285, #2865, #30351, #17550, #74847, #68203, #46402, #30826, #3323, #61120, #82856, #60179, #24164, #37441, #53045, #81920, #88086, #59722, #31749, #45460, #60641, #24639, #81004, #23244, #53527, #37896, #74360, #66801, #89958, #88565, #18008, #46861, #52122, #81456, #23713, #16147, #68674, #26030, #61575, #34094, #70079, #3808, #55404, #77646, #69598, #49226, #10885, #11829, #69136, #12797, #70557, #32689, #90407, #76703, #77172, #62032, #40680, #19872, #84257, #48270, #25564, #91827, #41638, #47321, #4728, #4264, #55871, #12302, #39748, #18463, #54444, #41146, #92293, #83317, #83793, #76238, #19407, #11369, #48742, #5222, #27450, #5680, #33606, #62996, #26981, #40220, #62514, #84723, #91355, #26515, #34555, #54913, #63464, #56342, #85204, #33142, #20354, #90866, #18947, #47802, #21758, #14199, #7531, #29790, #42572, #43060, #57286, #35499, #71964, #93241, #71488, #14662, #65332, #87514, #72864, #57742, #7990, #78581, #78123, #79048, #36883, #58670, #13719, #22661, #72415, #79968, #64414, #71013, #28394, #35955, #6619, #86587, #15105, #28856, #51080, #7082, #13261, #42098, #64874, #86128, #43965, #65798, #6145, #35016, #50149, #50633, #21277, #93700, #87061, #79523, #43517, #63931, #436, #910, #20816, #36416, #29324, #58217, #22210, #92769, #85668, #27937, #56827, #49686, #91110, #30710, #59131, #60073, #87974, #90638, #24060, #69368, #25801, #23606, #31187, #11132, #80423, #16498, #4046, #81348, #9374, #47577, #66696, #81813, #52474, #45350, #16042, #54681, #52936, #15568, #32916, #88910, #74252, #76001, #4498, #44895, #38257, #59609, #8912, #67171, #1824, #73798, #18243, #39996, #62275, #76482, #47095, #11605, #52009, #51534, #2304, #40450, #33376, #80895, #44439, #68915, #83555, #37789, #73345, #88459, #61806, #18714, #8456, #37337, #66243 ),
 ( #1358, #30241, #23126, #5462, #57065, #70788, #76945, #84035, #5923, #20115, #85903, #41877, #71260, #13964, #48997, #56111, #64651, #77896, #34793, #26279, #84496, #27699, #34332, #49469, #78359, #69840, #55174, #13499, #26758, #63238, #91602, #21055, #55643, #92533, #63708, #20599, #70333, #19642, #49922, #19180, #41399, #12072, #42347, #85451, #48040, #56597, #93017, #84964, #40920, #4974, #27223, #48510, #28175, #78819, #33860, #62770, #92069, #6388, #77411, #13040, #35259, #64185, #42822, #12549, #71737, #6863, #35738, #58453, #57986, #44680, #1144, #28633, #7312, #21518, #66031, #81134, #38025, #72647, #36191, #8242, #65110, #37571, #30025, #16278, #66481, #65574, #73115, #51778, #57522, #87297, #73582, #29572, #51316, #88228, #14893, #58908, #688, #22443, #86839, #1598, #87754, #86367, #8691, #37122, #80208, #22907, #45129, #21997, #15348, #7769, #50869, #44208, #43747, #79751, #80667, #15823, #9147, #23384, #30481, #52253, #213, #93480, #59376, #74030, #50396, #29093, #79301, #14441, #43298, #36653, #72195, #53177, #24782, #2545, #46534, #3938, #32812, #46992, #60313, #18138, #11500, #23840, #59851, #66934, #54115, #82533, #2995, #82988, #75894, #88692, #11018, #76374, #75436, #9625, #18602, #89151, #81587, #68336, #39888, #30963, #2072, #16735, #39419, #68809, #3459, #10554, #32354, #60771, #83447, #67416, #31424, #61253, #52706, #67872, #45590, #46074, #17682, #38960, #31881, #61702, #90089, #24300, #25241, #38512, #47467, #74980, #90534, #53664, #25694, #82056, #74493, #54576, #17213, #10092, #89611, #27584, #47935, #91000, #4395, #76838, #84386, #70680, #13388, #19535, #91957, #70221, #20001, #42231, #56481, #48401, #5356, #85339, #20490, #77304, #34222, #11965, #34684, #5810, #91492, #63598, #63128, #62169, #69266, #27112, #12436, #92422, #55996, #48879, #33272, #84851, #49356, #26169, #26647, #78250, #55060, #40813, #40349, #83929, #19081, #69730, #4863, #77782, #33746, #12930, #41770, #55537, #62658, #41286, #90374, #88983, #31714, #90830, #18426, #18911, #89442, #60606, #75268, #47766, #82818, #2832, #54875, #83755, #68635, #10382, #39711, #53009, #24131, #81884, #76664, #24601, #61079, #39250, #82365, #25077, #46366, #53489, #61541, #47285, #40641, #25989, #10847, #11791, #17515, #31257, #32178, #69561, #60145, #68165, #17039, #25529, #33105, #3285, #45905, #89921, #17970, #53951, #3768, #61994, #74811, #11331, #46822, #76202, #40182, #9926, #75725, #32653, #38800, #54409, #83281, #67703, #69101, #4228, #12756, #27901, #56789, #48230, #4689, #85631, #5178, #41596, #70037, #64379, #34053, #70975, #42061, #92729, #48701, #91789, #28356, #62474, #19833, #55366, #20777, #63893, #91316, #49188, #71445, #63427, #43023, #33564, #5645, #62955, #6582, #93204, #26477, #84218, #70519, #6108, #55828, #34520, #42534, #78082, #34979, #77132, #49650, #35460, #41106, #92256, #26940, #78544, #57247, #12263, #84684, #27413, #86090, #21240, #56301, #85167, #20318, #13226, #50109, #79004, #14159, #88419, #16004, #43928, #51495, #30202, #7048, #36845, #23085, #7950, #29751, #66657, #87023, #8419, #72824, #65762, #36377, #73759, #44400, #35917, #51966, #15524, #872, #1320, #59093, #93659, #80383, #8871, #64835, #79930, #37749, #57703, #72375, #71926, #1784, #37298, #87934, #80857, #65291, #30667, #7492, #58632, #28820, #43479, #22174, #66204, #86546, #395, #59570, #44856, #23569, #29285, #58181, #51042, #52436, #87473, #15066, #81311, #16457, #73308, #22621, #21717, #50592, #79486, #14621, #83637, #2265, #38216, #45309, #32546, #60957, #75158, #61438, #54298, #67131, #90269, #54760, #24970, #81773, #90718, #67595, #60034, #46713, #25420, #9333, #74214, #88871, #17862, #83170, #75616, #53845, #10740, #39140, #61886, #45782, #74694, #82711, #31147, #46254, #24020, #24485, #89809, #17406, #10270, #18321, #39597, #9816, #68520, #16923, #25878, #53365, #3657, #32062, #47177, #31604, #52894, #4123, #76087, #38689, #68051, #40076, #2724, #60493, #89330, #82251, #3178, #11221, #68993, #32995, #56188, #34408, #13116, #93094, #78436, #48590, #63315, #13572, #42422, #19719, #92146, #77022, #85524, #27782, #91681, #49541, #27301, #69449, #76560, #85048, #12635, #71334, #20197, #4579, #41952, #77974, #11683, #49076, #20669, #77490, #57135, #18801, #41481, #12151, #6464, #35339, #40533, #33454, #84572, #70865, #69919, #70412, #56676, #5996, #34869, #62356, #63782, #64265, #55256, #5537, #40996, #92611, #28248, #47659, #26367, #91198, #84111, #19261, #48119, #26832, #5058, #33942, #62847, #55720, #58525, #8765, #30097, #58062, #65646, #44287, #21127, #50937, #37196, #22069, #43818, #80746, #7382, #22518, #86915, #79821, #50472, #87829, #87368, #49995, #66103, #29645, #14962, #15419, #37644, #79376, #72717, #65183, #43368, #7840, #36262, #14512, #51389, #73194, #1674, #15898, #761, #44754, #86434, #85977, #36727, #73655, #66552, #21593, #30556, #80280, #22980, #72264, #78890, #286, #8313, #29166, #1215, #51854, #14037, #58981, #42899, #71812, #6933, #35806, #64720, #93546, #28705, #57590, #75055, #59454, #23915, #60849, #67490, #82608, #17755, #9224, #88305, #46608, #59930, #38587, #31040, #25316, #88769, #31956, #3071, #53742, #9706, #52787, #83064, #23463, #74578, #67948, #81665, #89692, #2150, #75974, #2621, #75510, #46151, #32431, #45670, #38105, #18218, #24858, #52329, #24377, #54195, #16813, #74105, #81206, #31499, #60387, #68413, #68884, #89226, #10632, #10166, #39490, #39968, #47068, #53256, #39035, #11103, #4014, #82138, #3542, #17295, #61330, #90168, #16352, #45202, #67015, #51904, #30144, #16860, #59973, #3116, #45717, #82188, #80796, #38631, #60893, #15944, #74153, #89743, #73701, #1718, #1262, #24904, #60432, #75556, #8810, #59506, #30603, #52375, #67066, #81250, #16397, #38150, #2201, #31085, #88811, #23958, #52834, #67534, #4063, #68932, #18735, #56129, #91131, #11154, #63255, #92086, #76962, #47596, #48058, #61377, #3591, #90210, #77916, #25359, #32480, #39534, #26775, #55194, #69385, #55661, #48528, #54239, #84513, #49019, #19198, #76022, #84982, #61825, #83109, #40938, #19660, #18260, #68457, #47113, #12091, #77429, #69858, #4994, #33879, #33394, #20135, #40015, #32933, #62787, #90658, #40468, #25818, #76498, #84051, #11622, #4518, #12571, #41420, #54698, #70352, #62293, #91620, #26301, #5478, #34348, #27242, #14458, #228, #70806, #41894, #27719, #79320, #29108, #43315, #86382, #72211, #6881, #30857, #13514, #42364, #21533, #92550, #13980, #13058, #85919, #28648, #78834, #42840, #86859, #50415, #71276, #7327, #49485, #59751, #21070, #36207, #93495, #81032, #93035, #56617, #66826, #65126, #5940, #71756, #9044, #6403, #85468, #34812, #35277, #35754, #22014, #23740, #64667, #58004, #57539, #50884, #88591, #73927, #16176, #45028, #37922, #1965, #52603, #63725, #64205, #20615, #78375, #49940, #28191, #57080, #38402, #45486, #32241, #75331, #18489, #3350, #39780, #9514, #61149, #47354, #74385, #89505, #76270, #67311, #81946, #81484, #11396, #46889, #68704, #10911, #74876, #83343, #17104, #82429, #2441, #53071, #31776, #75790, #31319, #45970, #40248, #3834, #69164, #9986, #38859, #60669, #4291, #39312, #67765, #33169, #62060, #25138, #24671, #89984, #60206 ),
 ( #89044, #2892, #53557, #32716, #24194, #17579, #90894, #61601, #26058, #46428, #10446, #68230, #16632, #54014, #82881, #18036, #90434, #25590, #54474, #63495, #76733, #18979, #11860, #93274, #40709, #47831, #54946, #42130, #70586, #84752, #71046, #63963, #69629, #6180, #64448, #34588, #91390, #6656, #77200, #4757, #56373, #35048, #33637, #83825, #62547, #27482, #92804, #85240, #92326, #20388, #48771, #71521, #55433, #84285, #49260, #26545, #55898, #19435, #34122, #5713, #27011, #19900, #27970, #78154, #48299, #13292, #12330, #35534, #63026, #56860, #41668, #85702, #41174, #70115, #13758, #20847, #5253, #77678, #49718, #91857, #12830, #78613, #42606, #29361, #37367, #37822, #472, #65835, #44002, #22693, #8944, #88010, #58253, #72899, #23163, #52047, #87096, #8024, #86621, #1390, #66276, #7563, #59164, #36920, #79081, #86159, #943, #22246, #80931, #29821, #80454, #50184, #58703, #43093, #87546, #15600, #51568, #44473, #73379, #51116, #44929, #28887, #57776, #8489, #14234, #80002, #28427, #36449, #30273, #15140, #16076, #73830, #66729, #21792, #57319, #64906, #21312, #65364, #71998, #7117, #35986, #14694, #7, #50667, #79553, #43549, #72445, #90337, #2341, #16530, #59648, #31220, #2792, #10811, #11294, #67666, #39210, #17476, #89881, #76161, #61505, #31674, #46327, #25492, #54370, #60566, #75230, #60105, #68595, #39672, #74769, #32615, #10344, #52506, #88493, #68124, #89404, #83244, #3248, #53913, #23640, #32139, #18391, #81382, #9887, #47249, #45382, #88945, #1856, #40147, #61036, #82781, #25041, #24092, #3731, #52969, #24558, #74284, #67208, #45862, #17933, #9408, #81846, #30745, #46784, #38293, #16996, #38762, #53443, #82326, #75685, #40606, #92686, #27855, #12713, #48190, #77565, #90792, #33067, #25952, #13641, #54833, #61957, #69063, #56262, #84643, #5134, #85121, #78044, #83713, #20273, #78503, #48663, #11753, #20737, #91273, #18874, #70478, #49148, #47730, #4192, #34939, #4652, #41555, #5606, #63386, #19328, #62432, #56747, #76630, #84180, #69520, #92217, #34480, #33526, #19794, #42019, #34013, #26439, #55330, #69994, #77092, #70935, #63853, #12222, #41069, #62915, #27372, #91751, #26902, #13185, #6066, #85590, #55791, #49607, #73266, #78961, #7450, #7002, #87433, #43886, #71406, #50065, #64335, #15027, #30162, #80812, #21668, #14112, #51001, #42975, #80343, #72782, #59044, #15485, #14578, #22133, #829, #6538, #36332, #22579, #72330, #352, #37258, #57657, #7907, #43434, #65246, #35875, #44356, #36797, #35415, #51454, #79886, #29239, #65717, #87892, #64791, #58134, #50545, #93616, #86980, #86505, #28774, #29711, #58593, #51922, #66164, #8378, #1279, #71881, #42492, #23044, #93162, #28315, #79442, #57204, #86045, #21194, #2219, #8829, #31103, #67552, #45268, #89287, #46668, #75572, #89760, #9288, #60914, #24922, #3610, #38648, #45737, #54255, #2681, #31560, #15961, #74171, #17360, #23978, #39093, #68006, #59525, #44815, #3135, #16415, #88829, #81270, #38170, #46212, #32015, #25375, #10694, #24440, #39551, #67086, #73718, #16878, #68474, #61394, #59990, #90225, #10226, #17815, #52852, #37708, #81730, #60452, #74647, #53321, #32496, #66614, #53798, #9774, #82667, #1736, #30624, #82206, #75116, #88374, #23524, #52393, #83125, #47613, #84527, #91151, #12589, #41435, #32950, #18276, #70367, #83592, #62310, #54714, #49033, #18755, #55677, #26791, #77444, #33411, #76516, #13072, #47130, #4535, #40033, #5492, #48543, #76043, #33895, #56144, #48074, #27735, #11172, #84066, #11639, #84996, #77929, #68949, #4080, #55212, #19675, #40486, #19216, #92102, #62802, #34365, #61843, #63270, #20152, #25835, #76978, #69402, #27257, #41908, #90675, #26317, #12107, #70821, #5953, #40953, #69874, #5013, #91637, #34826, #63738, #92564, #73149, #718, #28663, #36220, #14923, #85482, #21547, #7797, #86395, #14471, #51347, #71771, #86874, #57550, #50432, #21084, #58482, #29122, #20629, #36682, #241, #79336, #79780, #8273, #49955, #43328, #35768, #13994, #72226, #6893, #65605, #44238, #7340, #65140, #1173, #58019, #22028, #56632, #78847, #50897, #64681, #43776, #72678, #6417, #49499, #29604, #57094, #93507, #28206, #22474, #85934, #87326, #80239, #15376, #37153, #42856, #66061, #78389, #13529, #42378, #71291, #35293, #64219, #93050, #3026, #88724, #68365, #30055, #30997, #88263, #31912, #89643, #51808, #87787, #2107, #2576, #81165, #59884, #38990, #74526, #67448, #80702, #17247, #60804, #66510, #23872, #23420, #75012, #31454, #58936, #37600, #15853, #60343, #17713, #22937, #9180, #1630, #38545, #30512, #67903, #89180, #46566, #24814, #52738, #9661, #82088, #44711, #81620, #10124, #16769, #45623, #53697, #45161, #24332, #53209, #46107, #52285, #82565, #75465, #73612, #10586, #39449, #8723, #59408, #16309, #74060, #38058, #66967, #54609, #91032, #18637, #61735, #33782, #84421, #12966, #91994, #76872, #27147, #3971, #3494, #4426, #56033, #48916, #32845, #77817, #91527, #5392, #83480, #90121, #47504, #55097, #90567, #11998, #34257, #63163, #77339, #25725, #48435, #19113, #33304, #19569, #12473, #25273, #41321, #41805, #40847, #39924, #32387, #76411, #18171, #4897, #70258, #61287, #54150, #47024, #69766, #84887, #62697, #26683, #55573, #26202, #20038, #11533, #40380, #83019, #75927, #62202, #11053, #69297, #47968, #83964, #68843, #50792, #79220, #71183, #43222, #13425, #87218, #78742, #132, #57447, #43673, #56990, #20527, #29492, #72123, #5847, #35664, #65490, #6312, #85378, #34719, #35180, #71655, #79676, #80127, #42740, #14363, #86288, #65032, #51239, #36575, #6788, #21441, #607, #58375, #64579, #50315, #64103, #72568, #14818, #49846, #7690, #7239, #27621, #63633, #36115, #93404, #22365, #29015, #57900, #92458, #86756, #15266, #56519, #13886, #70716, #49396, #92943, #78287, #42270, #21918, #28103, #85828, #20979, #28556, #73501, #45048, #65955, #15736, #88139, #9538, #8158, #44598, #10008, #31340, #31796, #8613, #37489, #23297, #60690, #1986, #66399, #67786, #2912, #81505, #52171, #52623, #1066, #37041, #29945, #82452, #58830, #87675, #44126, #60227, #1515, #81053, #38423, #22826, #30401, #38879, #89066, #89530, #59293, #16196, #73949, #24694, #30877, #9064, #53577, #73030, #16652, #37942, #45506, #51694, #80583, #66851, #59771, #88612, #23759, #74408, #24216, #67332, #2464, #53091, #81970, #17126, #45992, #74897, #90915, #54034, #64351, #39802, #32263, #18999, #6079, #75352, #46450, #61169, #83846, #34953, #47852, #26081, #76754, #11417, #35429, #18057, #46909, #54970, #3375, #18513, #17600, #90455, #33192, #83363, #47377, #92699, #13197, #75810, #42033, #82901, #93177, #25612, #70947, #4314, #85603, #3854, #90005, #71418, #63865, #10467, #76291, #13654, #10934, #25160, #39333, #68724, #40268, #27869, #28329, #69185, #56762, #62082, #20750, #57219, #78517, #49621, #42506, #6550, #68251, #32734, #61623, #54495, #59060, #1294, #65260, #23059, #36811, #42991, #50079, #65732, #79901, #51937, #7920, #44369, #14126, #843, #80827, #78974, #366, #15978, #71897, #86517, #86059, #44830, #51468, #73280, #15498, #79456, #87908, #21682, #86994, #7017, #50559, #35888, #64806, #14591, #22146, #30176, #1754, #58148, #29724, #58606, #80357, #66629, #73733, #51014, #87447, #8845, #37723 ),
 ( #15039, #22593, #43448, #43899, #30641, #8393, #37271, #93630, #66177, #21209, #28787, #72796, #72345, #57674, #7463, #36346, #29252, #81286, #32035, #47150, #4095, #38664, #67102, #68025, #2236, #3626, #60930, #76059, #32514, #31579, #39112, #17835, #88390, #24459, #10712, #89303, #17377, #54271, #74665, #89777, #60468, #53338, #23995, #61410, #24940, #23541, #39569, #3152, #82223, #82685, #11188, #52868, #46229, #67568, #16897, #75133, #9789, #81747, #53817, #46687, #68965, #83141, #75589, #18292, #60006, #59540, #10243, #40048, #52411, #88846, #16432, #68491, #90242, #45755, #45284, #2697, #25391, #74187, #9306, #38188, #31120, #13088, #26336, #77944, #41926, #20645, #55693, #77463, #83610, #90690, #12606, #26807, #63754, #48560, #85017, #54732, #41451, #92584, #25850, #40969, #27753, #18771, #33426, #32966, #56648, #92119, #20169, #56160, #55229, #34843, #62330, #33911, #47629, #4552, #76995, #27273, #76533, #91170, #85498, #49049, #49515, #84084, #19234, #12124, #78407, #84544, #48091, #13546, #42394, #70383, #69892, #5511, #11655, #40502, #69421, #71306, #5031, #62820, #61859, #70837, #34381, #91654, #5969, #19691, #63286, #22489, #15870, #79794, #42871, #51824, #28679, #21101, #7810, #87340, #64236, #35311, #49969, #72691, #51362, #36700, #14936, #65621, #256, #22950, #6906, #35781, #43791, #85949, #7353, #6436, #79349, #22041, #72239, #36235, #80253, #731, #64694, #29617, #71784, #80717, #14484, #58495, #86887, #73167, #86408, #78860, #58953, #15389, #93066, #65153, #1187, #93520, #14011, #28221, #57565, #29139, #44256, #44726, #58034, #8286, #50910, #37166, #57109, #66075, #30068, #87801, #21563, #50447, #43342, #38559, #45174, #3042, #39004, #59898, #31925, #23886, #52754, #10138, #2590, #16323, #60358, #52301, #82579, #88740, #82105, #9677, #60817, #66984, #88278, #53712, #89195, #8738, #81636, #89660, #81178, #30525, #37615, #74076, #16783, #67918, #75479, #45637, #31470, #67461, #53223, #10604, #24829, #74546, #24348, #17726, #46581, #17264, #46122, #9195, #73626, #66526, #75025, #1645, #59427, #38073, #2122, #23433, #31011, #1486, #80096, #22792, #86255, #44093, #30369, #28521, #72538, #59258, #50279, #65002, #64545, #88106, #29915, #51661, #87644, #57869, #66368, #104, #65457, #21406, #36083, #14787, #58799, #57416, #28983, #23264, #80548, #52142, #86725, #21889, #43640, #81022, #22336, #50761, #16166, #45018, #8127, #7657, #72998, #79187, #14331, #43191, #9036, #72091, #7208, #93371, #15705, #15237, #574, #44566, #73469, #79645, #8581, #73919, #37011, #36542, #29458, #58346, #87187, #65925, #37459, #51207, #1037, #52594, #10438, #25130, #39304, #17569, #3341, #31768, #54464, #38391, #67303, #46420, #23731, #38849, #37914, #17093, #53548, #68694, #3825, #18026, #31311, #82873, #46880, #25581, #60660, #67757, #76259, #89497, #82421, #66818, #2431, #68221, #45961, #61140, #89976, #81475, #1951, #54004, #60197, #74866, #9503, #32706, #89035, #32232, #75321, #75782, #81938, #24185, #61592, #30848, #53063, #88583, #10902, #39769, #59741, #90424, #83334, #2883, #16624, #45478, #24660, #9978, #18480, #47342, #74377, #69154, #77191, #77666, #62535, #41164, #20376, #55889, #48761, #62051, #92315, #42117, #47820, #70101, #69618, #56362, #12818, #40239, #18967, #33160, #41658, #92789, #49704, #84275, #76722, #19890, #11848, #49247, #70575, #27957, #78142, #12320, #84743, #63484, #4282, #5242, #85225, #34113, #63015, #6167, #26534, #5700, #91846, #27001, #4746, #13280, #34575, #90885, #71033, #27469, #35036, #63950, #56847, #33626, #85688, #19426, #91376, #20835, #55422, #48288, #11387, #26048, #54934, #83814, #40698, #73361, #79067, #78600, #79541, #37353, #30257, #14219, #59149, #72884, #80439, #64893, #71507, #26508, #36435, #43079, #58237, #65818, #79987, #87081, #43987, #72433, #1375, #71984, #7102, #22230, #64434, #14680, #13743, #57761, #457, #50653, #43536, #58687, #51100, #35973, #15124, #21298, #87993, #86607, #8009, #65350, #51551, #28874, #28414, #66260, #36901, #42592, #7550, #8473, #21777, #93260, #6640, #29344, #926, #87530, #23146, #29806, #22678, #15584, #44455, #35520, #57305, #86147, #50170, #17918, #75669, #52952, #2776, #16515, #25025, #61019, #31204, #82765, #31657, #8928, #16059, #60548, #45845, #46768, #67650, #10328, #73815, #89387, #10794, #44912, #60089, #39654, #37806, #52490, #52029, #68578, #17459, #39195, #75214, #45366, #53897, #81365, #81830, #66713, #23623, #2324, #46309, #1841, #74269, #3714, #68107, #32599, #9392, #38276, #88928, #61489, #9870, #67189, #90321, #80914, #24541, #24076, #53425, #30728, #59629, #88476, #16980, #74750, #38746, #82309, #3232, #32123, #89865, #12697, #34461, #18374, #41536, #34921, #5118, #61939, #70916, #47714, #40130, #26887, #70462, #83228, #54355, #69047, #91734, #47232, #84164, #5589, #55312, #77075, #20254, #40590, #55774, #26421, #91257, #83695, #27355, #84627, #76143, #63369, #62898, #19312, #48646, #6049, #18856, #48174, #4635, #76614, #12206, #69504, #11737, #19775, #92199, #63835, #49130, #33995, #78026, #25935, #25475, #41051, #13166, #11277, #54817, #4176, #77546, #56243, #33509, #33049, #62415, #69977, #85104, #42002, #90776, #29691, #72765, #86028, #43868, #7888, #80325, #21650, #28757, #37242, #50527, #14560, #92666, #57187, #334, #6984, #22115, #50984, #42475, #27838, #79869, #93142, #71863, #64317, #58575, #28297, #65229, #36313, #86962, #42957, #21177, #22562, #56727, #14093, #49590, #15009, #58117, #85573, #43417, #65697, #57640, #20720, #78486, #93599, #50046, #811, #87415, #13622, #71387, #64774, #29219, #78943, #86485, #36778, #72312, #51436, #6519, #15466, #44338, #35397, #79425, #35857, #73248, #8359, #7433, #18241, #32456, #76942, #92066, #48994, #83552, #47093, #19177, #75998, #48507, #12069, #27220, #77408, #76479, #84032, #62767, #33857, #69837, #68434, #55171, #12546, #69365, #10657, #39513, #11602, #68912, #41396, #70330, #61356, #3566, #40447, #40916, #61803, #4495, #19639, #48037, #4971, #90190, #91599, #5459, #11129, #33373, #4043, #55640, #26755, #25338, #39993, #54218, #84493, #56107, #83087, #18711, #32913, #34329, #90635, #63235, #84961, #20112, #25797, #62272, #54678, #47574, #91107, #26276, #29090, #13961, #35735, #72644, #93014, #14438, #78815, #49919, #42345, #79748, #50393, #13037, #57983, #21515, #42819, #7309, #29569, #71256, #71734, #57062, #35256, #6860, #28172, #6385, #43295, #65107, #87294, #7765, #57519, #36650, #78356, #77893, #64648, #65571, #58449, #13496, #22440, #72192, #14890, #64182, #70785, #85900, #93477, #21052, #86363, #43744, #685, #86836, #28630, #21993, #50866, #41874, #79298, #36188, #5920, #209, #34790, #63705, #92530, #27696, #56594, #85448, #20596, #49466, #51313, #38509, #51775, #30477, #22903, #17210, #80664, #23837, #88689, #45586, #1595, #44677, #74977, #15344, #66478, #8239, #67413, #44205, #80205, #66028, #52703, #2542, #81584, #30960, #16732, #45126, #67869, #15820, #73579, #59848, #37119, #52250, #73112, #59373, #66931, #23381, #81131, #31421, #74490, #8688, #9622, #87751, #2992, #88225, #60310, #38021, #24297, #37567, #1140, #10089, #89148, #30022, #16275, #46071, #74027, #58905, #9144, #2069, #53174 ),
 ( #82053, #38957, #31878, #60767, #89608, #24778, #25690, #82984, #26643, #84382, #46531, #82530, #90530, #90995, #75889, #54572, #33741, #69262, #62165, #75433, #11961, #55533, #61250, #83443, #18134, #69726, #26164, #53661, #32351, #10551, #55056, #12431, #63124, #3934, #90085, #33268, #25237, #62654, #83925, #41281, #91489, #18597, #4391, #76834, #17679, #47463, #4858, #76370, #11496, #19531, #39884, #19077, #40345, #47931, #46988, #48397, #40809, #39416, #77300, #70218, #5352, #34218, #54111, #68333, #11014, #3456, #68805, #32808, #61698, #19996, #64539, #79640, #36537, #71141, #5806, #6751, #34680, #36078, #93365, #14782, #64996, #64061, #71617, #50272, #27108, #56952, #43185, #28062, #49809, #86719, #13384, #28515, #92903, #85789, #56476, #99, #57409, #55992, #72087, #35624, #20940, #21400, #43635, #85335, #78705, #6270, #49352, #13847, #42227, #20486, #86249, #79180, #7652, #21884, #14325, #50756, #92418, #91953, #42699, #72533, #84847, #27579, #48874, #7203, #28978, #78247, #77778, #35138, #57863, #12925, #41766, #70677, #63594, #45474, #58795, #16620, #74374, #53059, #88101, #1480, #9974, #23260, #81018, #65452, #29911, #66815, #73465, #88579, #23727, #15233, #568, #52590, #65921, #44562, #37008, #31307, #1033, #37910, #9032, #59737, #15700, #87639, #89031, #29453, #80544, #22332, #81471, #30843, #58341, #16162, #38386, #30365, #87183, #51203, #66364, #22788, #67299, #60193, #80091, #44089, #37455, #1946, #51657, #59254, #9498, #45014, #2427, #72993, #24180, #81934, #52138, #73915, #8577, #17088, #45956, #74862, #8122, #24655, #38846, #67753, #82417, #53543, #75317, #17565, #46416, #2879, #31764, #60656, #89493, #42332, #66339, #20099, #34778, #34316, #1453, #93463, #22760, #57505, #27684, #37430, #63693, #35243, #56095, #5908, #78343, #28616, #92054, #92518, #30339, #51631, #23231, #56582, #85435, #13485, #52111, #85887, #20585, #59229, #88075, #71720, #71243, #42804, #84949, #27208, #48981, #73889, #77879, #13026, #63222, #80517, #49907, #64170, #15670, #44537, #41862, #73440, #44988, #13947, #70775, #80994, #49455, #6372, #35721, #8550, #93002, #28160, #57051, #6847, #16136, #64635, #86349, #21039, #78802, #25555, #9472, #38358, #17540, #88554, #9950, #9006, #81910, #24629, #74837, #38822, #82846, #46392, #67272, #75292, #45449, #54435, #17062, #32202, #89468, #75754, #89006, #52565, #61565, #10411, #37885, #67729, #3798, #2402, #23702, #66790, #31282, #2856, #17998, #18453, #31738, #39275, #53516, #3313, #83308, #68662, #60631, #82392, #68193, #61109, #1920, #89948, #53977, #25103, #46851, #32679, #24154, #10875, #39738, #90398, #60168, #47312, #30814, #59711, #81445, #16593, #74349, #53034, #45928, #40671, #12293, #55395, #33597, #70071, #91345, #69589, #12789, #63455, #85660, #71005, #55863, #6136, #76694, #76228, #77163, #35008, #27928, #11820, #56818, #70549, #78114, #62505, #69127, #26505, #34085, #4719, #84715, #13253, #42090, #56334, #84247, #27442, #85196, #63923, #5212, #41138, #20807, #62988, #91819, #11358, #19398, #77638, #48261, #5672, #34547, #26021, #40211, #92285, #26972, #19864, #47792, #92761, #48734, #41629, #20346, #49218, #4255, #33133, #62023, #90857, #54904, #83783, #18937, #15098, #13711, #428, #22653, #14653, #87967, #49678, #50625, #14191, #51526, #15560, #71479, #42563, #21748, #22203, #7074, #79515, #58662, #29315, #87054, #6611, #36876, #80415, #86120, #43509, #43052, #901, #51073, #78573, #57278, #35491, #79961, #37327, #64406, #28848, #21269, #58209, #50141, #87506, #43958, #66235, #44431, #72407, #79039, #93233, #72857, #1350, #28386, #57734, #71956, #7982, #35947, #73337, #65791, #30233, #8448, #7523, #29783, #59123, #64866, #36408, #93692, #65323, #86579, #17893, #38250, #53399, #24052, #88902, #81340, #25003, #89360, #52001, #3208, #60524, #52926, #46285, #68554, #16488, #81805, #2296, #74244, #16954, #67163, #45343, #82284, #10302, #32576, #46746, #2753, #75647, #52466, #23118, #45819, #10770, #3691, #9366, #61469, #17435, #53874, #31179, #16035, #60064, #74725, #9846, #31634, #82740, #39630, #32094, #38719, #68083, #60996, #80887, #67625, #24518, #44886, #75189, #39172, #73788, #89841, #8904, #37781, #66688, #1816, #30702, #59601, #88451, #90751, #69479, #61915, #56219, #25909, #62875, #33971, #84602, #40565, #83671, #20230, #54330, #11712, #47209, #19752, #55749, #83204, #41024, #63344, #55286, #34899, #90299, #91233, #54792, #92176, #85079, #18351, #76120, #62390, #91709, #47688, #26398, #5567, #69950, #26861, #11252, #77520, #27332, #33024, #84140, #18833, #41514, #48619, #25451, #76590, #40107, #12672, #70440, #69022, #4154, #4610, #34438, #49107, #78004, #5092, #13144, #19289, #41980, #33484, #48148, #70893, #77052, #12181, #6025, #42931, #79401, #35833, #64749, #43844, #72286, #64293, #36288, #6493, #80306, #71840, #86941, #50503, #36753, #50024, #13599, #22541, #65207, #92642, #28733, #58550, #93119, #78463, #27814, #28275, #93575, #72743, #73226, #57617, #7408, #14537, #58091, #44314, #29669, #86460, #43392, #87394, #51414, #21621, #311, #57165, #65675, #7864, #6960, #787, #29194, #20698, #56704, #22093, #50963, #15445, #79846, #14986, #85551, #8338, #63810, #49568, #42451, #71363, #35374, #86005, #21154, #78917, #14066, #24401, #60410, #30580, #39056, #66576, #38127, #59006, #8789, #81229, #2644, #1241, #37668, #3094, #53280, #24882, #1697, #59481, #16376, #53763, #88790, #88334, #60871, #89718, #74605, #45226, #45694, #87854, #30123, #23003, #75533, #51881, #80774, #37219, #82164, #52810, #67040, #17321, #46172, #15924, #75076, #46632, #16838, #73678, #82629, #23486, #9734, #38611, #31522, #74130, #52353, #17778, #44778, #9249, #2177, #89249, #10187, #31063, #81689, #67968, #59951, #66126, #23938, #67514, #31978, #67631, #31640, #87512, #29789, #37787, #38256, #23124, #1822, #74731, #16495, #9372, #22659, #52933, #2759, #8454, #30708, #30239, #16960, #67169, #908, #73343, #51532, #2302, #53405, #10308, #44893, #37334, #74250, #66241, #9852, #31185, #82290, #38725, #66694, #45348, #24058, #58668, #59607, #45825, #88457, #23604, #60530, #80893, #60071, #52472, #81346, #59129, #89367, #88908, #80421, #24524, #81811, #17441, #46291, #75195, #87973, #65797, #73795, #52007, #15566, #16040, #8910, #44437, #1356, #48625, #33979, #18840, #62882, #39637, #39178, #40113, #91716, #84609, #68561, #19758, #33491, #41031, #25457, #32102, #54336, #90758, #3697, #47696, #69958, #5099, #19296, #32582, #84147, #48155, #26869, #61922, #69028, #77527, #25916, #54799, #68089, #61475, #40572, #47216, #62398, #91240, #82746, #3214, #26405, #83210, #18357, #10776, #55756, #75653, #4160, #76126, #77059, #4617, #61002, #46752, #89847, #55293, #25009, #53880, #11259, #33031, #76597, #83678, #12188, #17899, #30476, #51774, #79747, #87293, #66027, #42818, #72643, #58904, #43743, #65570, #8687, #29089, #44204, #14889, #7764, #72191, #15819, #80204, #71732, #87750, #51312, #36649, #37118, #59372, #7308, #683, #86834, #65106, #29568, #57982, #36187, #73111, #1139, #23380, #37566, #22439, #66477, #14437, #12678, #58448, #1594, #88224, #43294, #52249, #8238, #44676, #208, #6859, #21992, #15343, #50865, #30021, #73578 ),
 ( #22902, #80663, #35734, #64647, #93476, #28629, #57518, #86362, #21514, #50392, #79296, #18133, #2991, #39415, #9143, #60766, #46987, #45125, #89147, #75888, #66930, #81583, #81130, #11013, #46530, #68332, #10550, #74489, #82983, #16731, #82052, #38020, #52702, #31420, #45585, #9621, #60309, #3933, #38956, #38508, #39883, #68804, #24777, #24296, #89607, #2068, #74026, #30959, #25689, #59847, #88688, #16274, #3455, #31877, #17209, #32350, #90084, #23836, #61249, #90529, #53660, #67412, #32807, #2541, #53173, #82529, #25236, #46070, #74976, #10088, #17678, #54110, #75432, #61697, #67868, #48396, #71140, #55055, #83924, #63123, #40344, #55532, #54571, #33740, #70217, #26642, #84381, #34679, #91952, #19076, #27107, #90994, #6269, #62653, #77777, #41280, #27578, #40808, #4390, #13383, #55991, #83442, #19530, #49351, #47930, #69261, #18596, #76833, #77299, #63593, #64060, #12430, #84846, #5351, #48873, #35137, #20485, #34217, #19995, #78246, #42226, #12924, #41765, #11960, #56475, #92417, #91488, #85334, #70676, #11495, #47462, #5805, #92902, #76369, #33267, #62164, #26163, #69725, #4857, #85788, #36077, #58794, #13846, #28514, #28061, #87638, #87182, #15232, #51202, #21399, #29910, #57408, #28977, #49808, #93364, #72086, #22331, #20939, #86248, #22787, #44088, #15699, #29452, #72992, #78704, #56951, #42698, #567, #8121, #58340, #7651, #80090, #21883, #44561, #50271, #79179, #36536, #71616, #57862, #6750, #7202, #43634, #98, #86718, #37007, #65451, #14324, #65920, #64538, #73464, #64995, #1032, #14781, #51656, #43184, #35623, #80543, #8576, #50755, #79639, #37454, #72532, #66363, #59253, #1945, #2426, #10434, #10898, #67298, #38845, #17087, #89492, #75778, #61135, #31306, #45955, #89972, #25126, #60192, #74861, #59736, #68217, #39299, #74373, #32227, #9973, #52137, #88100, #67752, #89030, #54000, #2878, #53542, #23259, #31763, #82869, #81017, #9497, #18022, #16161, #30842, #1479, #46875, #60655, #82416, #24654, #88578, #3337, #23726, #24179, #45013, #66814, #45473, #17564, #73914, #52589, #39764, #46415, #30364, #81470, #16619, #38385, #9031, #53058, #81933, #37909, #75316, #12315, #47815, #77186, #90420, #32702, #25577, #13275, #54459, #61588, #68689, #55884, #84270, #4741, #84737, #77661, #83330, #19885, #78137, #48283, #11383, #20371, #90880, #18476, #4277, #41159, #5695, #34570, #48756, #62046, #12813, #41653, #56356, #91370, #33621, #3821, #26529, #19421, #47337, #33155, #70095, #76717, #91841, #26996, #76254, #40234, #70570, #69149, #11843, #26043, #63479, #54928, #5236, #34108, #63010, #18962, #83809, #92309, #40693, #69612, #62529, #27464, #85219, #55418, #49242, #15119, #7097, #80435, #42112, #43074, #6634, #43981, #8004, #63945, #6161, #14213, #14675, #93255, #71978, #51095, #86602, #79536, #92783, #29338, #72879, #78595, #35968, #35515, #87076, #43531, #71028, #49699, #27952, #72428, #29802, #35031, #21292, #13737, #50648, #42587, #79982, #7545, #58683, #36895, #64888, #21771, #452, #56842, #93713, #22225, #28868, #57756, #65812, #57300, #36429, #65345, #58232, #64429, #922, #87527, #85683, #22674, #51546, #20830, #71502, #28409, #86142, #50165, #79062, #66707, #9387, #30723, #73810, #45840, #2771, #25020, #10323, #88923, #39190, #16054, #15580, #16510, #68102, #61014, #44907, #89860, #9865, #17454, #1836, #8469, #59623, #67183, #3227, #32118, #52947, #88471, #24071, #37349, #73357, #66256, #53892, #1371, #30253, #44450, #31653, #31199, #45361, #60543, #24536, #59144, #89381, #87988, #81824, #52023, #23141, #37801, #80909, #16975, #53420, #8923, #23618, #52485, #74744, #82303, #38740, #67645, #46304, #38271, #81360, #74264, #2318, #75208, #60084, #83690, #82760, #61934, #4630, #54812, #18851, #62893, #91252, #83223, #55306, #25470, #5584, #90770, #12201, #69499, #55769, #69042, #32594, #41531, #84159, #17912, #47709, #77541, #18368, #3709, #46763, #47228, #76608, #91729, #92194, #11732, #26416, #33503, #77070, #63364, #48639, #40585, #62410, #12691, #70457, #19307, #48169, #76138, #84622, #26882, #25929, #19770, #41044, #39649, #75664, #69972, #5112, #34455, #33990, #27350, #10788, #68572, #61484, #90316, #54349, #11272, #40125, #4171, #33044, #86958, #21644, #43412, #79420, #49585, #58113, #85568, #57182, #78021, #27833, #6514, #50522, #20249, #56722, #22111, #72307, #43864, #20715, #78481, #35392, #72761, #14087, #13617, #64312, #14555, #7428, #6044, #56236, #36308, #42470, #93137, #71380, #50980, #28292, #28752, #93594, #65224, #86023, #21172, #79865, #49125, #50041, #13161, #328, #29214, #41997, #6979, #15005, #78936, #807, #85099, #42952, #71858, #7882, #36773, #70911, #34916, #35852, #57635, #64769, #86478, #65693, #63828, #92661, #80321, #16855, #60426, #66142, #88352, #87871, #74623, #31080, #58571, #37238, #51432, #2196, #17338, #67985, #8806, #1258, #38143, #30140, #67529, #59968, #46189, #2659, #1714, #9266, #81706, #87411, #23503, #9752, #59500, #81246, #24416, #44794, #88806, #30598, #52371, #23020, #31538, #23953, #22558, #38626, #67060, #16393, #52828, #75094, #51899, #45244, #37687, #80792, #74149, #73697, #15940, #45710, #89266, #39072, #53296, #82182, #10203, #59024, #29687, #15460, #44333, #73244, #66593, #8355, #91125, #4988, #83103, #89737, #18256, #54694, #32475, #76495, #33874, #62783, #76958, #90205, #48053, #12086, #84509, #25814, #32929, #41415, #83568, #18730, #3111, #61372, #4513, #3585, #76016, #68450, #91616, #25354, #69381, #40463, #26296, #47109, #54234, #26771, #60886, #11149, #53779, #55190, #62289, #24899, #47591, #69854, #61821, #31994, #82646, #4059, #40011, #55656, #19655, #17795, #46648, #68928, #33390, #90653, #11618, #40934, #84048, #19194, #75550, #48524, #77425, #39529, #12564, #10674, #21530, #71752, #5474, #77912, #92082, #42835, #57999, #14905, #49482, #13054, #78831, #41890, #14455, #6878, #86855, #43312, #42360, #49935, #28645, #34344, #35272, #50410, #6400, #28188, #65122, #85465, #35751, #71273, #64201, #34808, #72208, #64664, #63251, #79316, #13977, #93032, #93492, #22011, #63721, #57077, #78372, #27714, #85916, #20612, #92546, #57535, #86379, #79763, #225, #7325, #29105, #70801, #70348, #21067, #50881, #27237, #5936, #56125, #36203, #84978, #56613, #20129, #13511, #49014, #73128, #23401, #74507, #9638, #23854, #37136, #88706, #52720, #32713, #66494, #73594, #83340, #1611, #59390, #43761, #8255, #45144, #51790, #66948, #2087, #87309, #72660, #30977, #16750, #81602, #22920, #38525, #88242, #702, #7781, #52267, #37583, #68701, #81147, #59865, #65587, #16291, #3831, #36667, #80680, #61598, #29586, #44220, #58465, #90431, #9161, #45605, #25587, #66044, #54470, #1156, #44693, #22456, #15360, #87768, #38040, #51329, #30039, #80222, #58920, #15836, #8705, #30496, #74043, #35045, #70109, #83822, #42125, #71042, #55895, #91385, #27007, #40245, #76266, #69161, #56856, #4288, #11393, #18486, #5707, #34119, #48295, #34583, #27478, #33166, #63492, #27967, #91853, #54942, #63959, #40705, #62057, #19896, #92323, #90892, #47349, #26055, #84749, #56370, #48767, #77673, #12826, #12326, #92799, #18974, #47827, #41665, #76729, #19432, #11856, #26541, #63021, #84281, #77197, #85234, #70582, #69625, #20385, #4753 ),
 ( #49255, #33633, #55428, #62543, #78150, #41170, #13288, #5249, #6176, #65360, #80449, #86157, #85697, #86618, #44467, #37363, #21308, #66270, #79997, #87541, #71994, #78609, #7112, #43545, #50181, #467, #22688, #51561, #65830, #79077, #36912, #937, #73372, #14690, #21788, #30267, #72442, #7560, #20843, #14229, #87091, #4, #15134, #43997, #35531, #49714, #72894, #43090, #64903, #57315, #15594, #35983, #58248, #29356, #8018, #28884, #57772, #8484, #13754, #50664, #42602, #29816, #51111, #71517, #36445, #58697, #79550, #6651, #64444, #22240, #1385, #93270, #28424, #80926, #23156, #31214, #31667, #16525, #88938, #68117, #9880, #2786, #16069, #46320, #89875, #1851, #24087, #23634, #10338, #60560, #88003, #66723, #44923, #89398, #46778, #3724, #38286, #30738, #67660, #59640, #3243, #24552, #75679, #32133, #60099, #38756, #17470, #52040, #52963, #39205, #81840, #16990, #53907, #74279, #53436, #45855, #74761, #52499, #61029, #82320, #73825, #25036, #75224, #82775, #17927, #10804, #81376, #39666, #67199, #45376, #68588, #9402, #2335, #59159, #8938, #37816, #88487, #84174, #4186, #56254, #85114, #69988, #11747, #41062, #54364, #90331, #83238, #70928, #18385, #25485, #32610, #19786, #48184, #62426, #48657, #41547, #47242, #77558, #42012, #12216, #69057, #78037, #54827, #76154, #34005, #12707, #11287, #61499, #40141, #5128, #70471, #62909, #91745, #26896, #26431, #49140, #33060, #61949, #55784, #90786, #33520, #25946, #40600, #77085, #4645, #91267, #5599, #84637, #83705, #34473, #18867, #13177, #69514, #63379, #19322, #92209, #47724, #76624, #20264, #27365, #55324, #64784, #821, #6531, #20730, #63846, #35407, #6995, #15019, #15477, #71873, #43427, #21661, #345, #80335, #65709, #35867, #50537, #29702, #58585, #93609, #79435, #64327, #72775, #43879, #78954, #36789, #14571, #56737, #92678, #72322, #28767, #87424, #7443, #58127, #27848, #36325, #22572, #85583, #14104, #51446, #49600, #93153, #6059, #44348, #65239, #86972, #29232, #28308, #7900, #57197, #57650, #78496, #71398, #50058, #22126, #13634, #86038, #34931, #50994, #42485, #21187, #42968, #86498, #79879, #53313, #59983, #8370, #81262, #89280, #80805, #30153, #37251, #15953, #23516, #38641, #75108, #52385, #31095, #38162, #52844, #10218, #24431, #16407, #67077, #60444, #82198, #45259, #2211, #44809, #2673, #67544, #59517, #31552, #88822, #1271, #66155, #23970, #74163, #17352, #81721, #16870, #59036, #45729, #46203, #87883, #88366, #73258, #73710, #30615, #23036, #51914, #8820, #37700, #66606, #74639, #1728, #9766, #9279, #85886, #35720, #14422, #29552, #28159, #64634, #30004, #51297, #51757, #28615, #93462, #43279, #80646, #21977, #57504, #87735, #22887, #7749, #72177, #72629, #21038, #57050, #49906, #8670, #78801, #13946, #64169, #80189, #79733, #192, #15329, #73094, #42803, #44189, #73561, #43729, #6846, #15801, #86348, #71719, #65554, #8224, #21499, #93001, #50377, #36633, #37102, #668, #58432, #87278, #57965, #44660, #79281, #7293, #22425, #36173, #65092, #29073, #86819, #14875, #50850, #66011, #1123, #58889, #38002, #10070, #74008, #54091, #45566, #60747, #24277, #10529, #81113, #90066, #38938, #66459, #2522, #32329, #66912, #52230, #1577, #2050, #38488, #46512, #46968, #9601, #74958, #53152, #31858, #18116, #3434, #67394, #82033, #61231, #25218, #31399, #17191, #30941, #39396, #75413, #16711, #68311, #46053, #88206, #30459, #67847, #60289, #82963, #2973, #89588, #59354, #24759, #75870, #23363, #74470, #37548, #16256, #59829, #45106, #9125, #53641, #82511, #17659, #88670, #23819, #52682, #89126, #81563, #76351, #55037, #70199, #68785, #11477, #70658, #91933, #92400, #69243, #40327, #83905, #27560, #62632, #4371, #34661, #63575, #48379, #19057, #19511, #32791, #3914, #61679, #49334, #90511, #25674, #10994, #27087, #26623, #40790, #55974, #19977, #54553, #84828, #20467, #84362, #47442, #56455, #33249, #83421, #12411, #48853, #18576, #39863, #62146, #77281, #77759, #41261, #5332, #34200, #4838, #85317, #90975, #26141, #63105, #47912, #11941, #76815, #69707, #55513, #33721, #91472, #12907, #41745, #5787, #50739, #20921, #1015, #86232, #7635, #64978, #51186, #64521, #22771, #78228, #79160, #42679, #80073, #44072, #6252, #42208, #50253, #79623, #35606, #14307, #87166, #28960, #21864, #35120, #65435, #15216, #49790, #43168, #71597, #29432, #14765, #13367, #85771, #64041, #43618, #65902, #71122, #57390, #78687, #86700, #13828, #22315, #72515, #29894, #72974, #72069, #57846, #36519, #92883, #7186, #58323, #36061, #81, #8103, #93347, #549, #36990, #58778, #6732, #87620, #28044, #56934, #28498, #21384, #81454, #74845, #3321, #16145, #16603, #30823, #9015, #45458, #66799, #44997, #81918, #38830, #61117, #46400, #31291, #75300, #52120, #51641, #52574, #10419, #32211, #81002, #89956, #45937, #53524, #37894, #44546, #1929, #9481, #73899, #60177, #82400, #17548, #31746, #59720, #2863, #60639, #39283, #74358, #38367, #80527, #67281, #2411, #15680, #88563, #53043, #23711, #9958, #67737, #1462, #73449, #89477, #89015, #24162, #23240, #68201, #17070, #24637, #8559, #37439, #66348, #30348, #59238, #88084, #40219, #75762, #48269, #84256, #82854, #69597, #91826, #83791, #34093, #4263, #55870, #4727, #10883, #18006, #33605, #18946, #84722, #40679, #77171, #46859, #62513, #19871, #39746, #33141, #48741, #68671, #25563, #25111, #77645, #19406, #12301, #41145, #18461, #26980, #54443, #26029, #3806, #90406, #69135, #70078, #32687, #83316, #12796, #5220, #41637, #47320, #76236, #62031, #70556, #76702, #11368, #5679, #34554, #91353, #90865, #26514, #61573, #54912, #47801, #63463, #11828, #55403, #53985, #62995, #14198, #28393, #79522, #7530, #85203, #14661, #7988, #71963, #35015, #43964, #20815, #13260, #93699, #43516, #56341, #27449, #42097, #64873, #72414, #28855, #7081, #57741, #86127, #15104, #92768, #27935, #35954, #78122, #93240, #92292, #71486, #43059, #64413, #57285, #36415, #86586, #56826, #21757, #63930, #72863, #6618, #50632, #79047, #65331, #78580, #71012, #51079, #435, #20353, #21276, #87060, #85667, #6144, #49225, #49685, #50148, #29323, #36882, #58216, #22209, #79967, #13718, #42571, #35498, #15996, #30659, #45774, #9808, #80848, #59561, #44391, #52886, #22612, #31597, #8411, #862, #81304, #67122, #43920, #15058, #29743, #52429, #2257, #16450, #88410, #45302, #73751, #2717, #80375, #15516, #23561, #65753, #44848, #79921, #59084, #1775, #51957, #8863, #60027, #74207, #73299, #9325, #51487, #60486, #87926, #38208, #66649, #81766, #66196, #58624, #38682, #31140, #72815, #37741, #74685, #37289, #87465, #7941, #1312, #88864, #24013, #89323, #16916, #67587, #24478, #36835, #30194, #23077, #83162, #4116, #20552, #78312, #54291, #32988, #17855, #27650, #63660, #32538, #85404, #61879, #10263, #17398, #90710, #47170, #49422, #68986, #12992, #75151, #27175, #13451, #46247, #61431, #42302, #39133, #53838, #53357, #71211, #20065, #41830, #77844, #46706, #56549, #82704, #18314, #68044, #24962, #3648, #48946, #3171, #75609, #6338, #70741, #35209, #10733, #39589, #90263, #64137, #11211, #68512, #92970, #82243, #56062, #25412, #84915, #32055, #60949, #89800, #76079, #40068, #5875, #34745, #92483, #57930, #7263, #65517 ),
 ( #65979, #7716, #51264, #21467, #85853, #50343, #160, #93430, #21945, #80157, #15295, #58400, #28582, #29520, #636, #8189, #29039, #36140, #29971, #86786, #50818, #28128, #57474, #43697, #43249, #36600, #87246, #42767, #57017, #22392, #86315, #72147, #79249, #73059, #14390, #72596, #44152, #37070, #65059, #79702, #1090, #49873, #14844, #71686, #21006, #78771, #6816, #13912, #35690, #64604, #57317, #18977, #19898, #77198, #20845, #78610, #40707, #76731, #84750, #85238, #70113, #48769, #27968, #63493, #56371, #69627, #6178, #49716, #55431, #77676, #12328, #63961, #20386, #47829, #26542, #4755, #49258, #6654, #11858, #91855, #84283, #27480, #19433, #56858, #78152, #35532, #85700, #12829, #92324, #71044, #33635, #41666, #92802, #70584, #5710, #13756, #34120, #13290, #34586, #42127, #41172, #42604, #35046, #62545, #71519, #64446, #93272, #28425, #91388, #48297, #5251, #63023, #27009, #55896, #86158, #65362, #8022, #58250, #87094, #66274, #941, #86620, #58701, #28885, #8942, #469, #15598, #72897, #59162, #72443, #35984, #44927, #87544, #21309, #51114, #80929, #21790, #7115, #50182, #50665, #22244, #1388, #1854, #80000, #29819, #36917, #80452, #66727, #52045, #15138, #65833, #16073, #73829, #44000, #22691, #79551, #88008, #30271, #29359, #23161, #51566, #43091, #79079, #44471, #73375, #37820, #8487, #37366, #14232, #30743, #71996, #64904, #5, #57773, #14692, #43547, #7561, #36447, #25039, #46782, #82779, #52967, #61503, #88942, #60564, #81380, #31218, #9885, #53911, #23638, #60103, #25490, #75683, #47246, #24090, #81844, #38760, #76159, #17474, #16994, #83242, #18389, #3246, #67664, #68121, #16528, #52503, #45380, #4190, #9406, #38291, #59646, #10808, #75228, #89402, #68593, #3729, #67206, #32613, #69061, #39208, #2339, #11292, #45860, #74767, #61034, #90335, #2790, #88491, #31671, #32137, #54368, #17931, #40145, #24556, #53441, #82324, #46325, #10342, #49605, #41067, #56260, #19792, #6064, #19326, #76628, #85588, #5604, #61954, #91749, #27853, #33524, #47728, #90790, #62430, #34011, #42017, #42490, #5132, #70476, #48661, #27370, #13639, #92684, #62913, #77563, #56744, #20735, #26900, #12711, #91271, #34936, #70933, #12220, #63851, #41553, #83710, #25950, #34478, #55788, #78501, #63384, #85119, #54831, #92214, #71403, #18872, #69992, #33065, #11751, #26436, #40604, #69518, #20270, #49146, #78042, #55328, #4650, #84178, #84641, #48188, #77090, #13183, #65715, #64333, #7000, #66161, #87431, #87890, #64789, #35873, #50542, #23042, #58132, #71879, #30160, #59042, #43884, #79440, #15025, #28313, #93159, #57202, #44814, #86043, #21192, #6536, #22577, #22131, #36330, #51452, #15483, #50063, #80341, #15959, #79884, #42973, #51920, #28772, #78959, #7905, #44354, #14109, #35413, #93614, #72780, #73264, #36795, #827, #29708, #350, #80810, #57655, #86503, #58591, #21666, #7448, #14577, #43432, #51000, #72328, #65244, #8376, #37256, #29237, #86977, #1277, #16413, #25373, #2217, #88372, #75114, #60911, #37706, #8826, #23522, #46210, #89758, #10224, #53319, #39091, #67550, #90223, #74169, #9286, #82204, #59523, #74645, #73716, #52850, #89285, #45735, #9772, #53796, #17358, #38168, #68004, #45265, #54253, #81727, #3133, #60450, #46666, #59988, #52391, #32494, #32013, #66612, #38647, #68472, #67084, #81268, #1734, #31101, #2679, #82665, #83123, #31558, #24920, #24437, #17813, #18274, #39549, #75570, #10692, #3607, #61392, #30622, #88827, #23976, #16876, #56143, #26315, #77928, #91635, #4078, #11170, #26789, #40951, #13071, #62800, #5491, #68947, #55675, #41907, #40030, #55210, #70820, #32948, #47611, #47128, #5952, #12588, #34364, #70366, #40484, #49032, #76514, #48072, #61841, #18753, #91149, #41434, #90673, #11637, #34824, #63269, #63737, #69400, #4533, #84064, #92563, #5011, #33409, #27734, #56631, #84526, #19213, #19674, #25833, #54712, #83590, #85481, #62308, #76976, #76041, #92100, #48542, #12105, #27256, #84995, #69872, #20151, #33893, #77443, #42377, #78388, #71289, #58935, #6416, #13528, #20628, #7796, #36219, #50430, #36681, #29602, #35292, #65604, #30054, #240, #57093, #66059, #42855, #64218, #22027, #717, #93049, #49498, #28205, #86872, #58481, #50896, #29121, #79779, #14470, #37152, #21083, #49954, #58018, #85933, #21546, #78846, #93506, #65139, #86394, #79335, #87325, #14922, #13992, #43775, #71770, #1172, #28662, #72677, #7339, #22473, #6892, #35767, #73148, #51346, #64680, #43327, #15375, #57549, #72225, #80238, #44237, #8272, #3025, #3493, #59883, #31453, #9660, #82087, #68364, #82564, #23871, #38544, #17712, #46565, #88723, #67447, #52284, #60803, #31911, #66966, #24813, #2575, #44710, #51807, #60342, #81619, #75464, #89179, #46106, #15852, #24331, #10585, #80701, #2106, #39448, #73611, #88262, #87786, #32386, #53208, #75011, #17246, #81164, #89642, #23419, #52737, #8721, #59407, #38057, #10123, #37599, #16308, #22936, #38989, #66509, #45160, #74059, #30996, #1629, #45622, #9179, #30511, #16768, #67902, #74525, #33303, #4896, #76871, #55572, #41804, #27146, #91031, #11997, #56032, #84886, #62201, #40846, #25724, #34256, #70257, #40379, #91993, #69765, #18170, #25272, #33781, #55096, #20037, #62696, #19568, #83018, #91526, #48915, #54149, #69296, #77816, #47023, #61734, #61286, #12965, #26682, #48434, #84420, #54608, #63162, #90566, #26201, #75926, #32844, #11532, #77338, #11052, #83479, #70715, #12472, #5846, #18636, #47503, #4425, #90120, #19112, #76410, #39923, #68842, #41320, #83963, #5391, #3970, #47967, #56518, #73029, #85377, #27620, #34718, #21917, #50314, #64578, #50791, #43672, #20526, #79675, #44125, #14362, #71182, #80126, #56989, #49395, #36114, #14817, #92457, #63632, #78286, #7238, #72567, #65031, #43221, #131, #28555, #51238, #35179, #64102, #72122, #13424, #35663, #42269, #13885, #79219, #6787, #93403, #7689, #29014, #92942, #57899, #6311, #15265, #42739, #86755, #21440, #36574, #20978, #28102, #87217, #65489, #85827, #57446, #29491, #49845, #78741, #71654, #86287, #606, #58374, #22364, #81052, #15735, #16651, #44597, #45991, #74407, #24693, #74896, #73948, #81504, #60226, #37040, #66850, #53090, #37941, #59770, #2911, #23296, #38422, #9063, #1985, #66398, #10007, #9537, #65954, #81969, #45505, #30876, #31339, #53576, #1514, #88611, #16195, #59292, #23758, #52170, #30400, #67331, #89065, #17599, #31795, #2463, #60689, #8612, #8157, #52622, #89529, #82451, #37488, #46449, #24215, #38878, #88138, #1065, #45047, #17125, #67785, #29944, #58829, #87674, #22825, #51693, #80582, #73500, #63045, #4313, #11416, #19920, #33191, #90914, #75351, #39801, #76753, #83362, #4777, #33659, #25159, #10466, #62568, #75809, #54494, #46908, #41199, #10933, #47851, #18998, #69649, #25611, #68723, #5273, #39332, #90454, #32262, #91409, #40732, #68250, #26080, #48321, #40267, #3374, #61168, #76290, #3853, #77222, #70137, #90004, #54033, #47376, #11881, #32733, #69184, #84304, #54969, #26564, #82900, #55453, #12350, #18056, #62081, #61622, #19454, #34142, #18512, #83845, #91876, #27030, #55919, #84771, #49278, #21331, #85260, #66627, #56880, #72019, #35554, #23057, #35066, #92345, #8843, #50201, #77700, #13776, #44828, #78173, #63517, #12849, #13311, #49737 ),
 ( #41687, #93294, #51935, #42625, #88388, #48792, #78634, #42149, #80825, #15976, #70605, #5732, #20866, #79105, #6199, #71544, #59058, #28445, #86180, #34607, #36007, #73731, #20408, #6677, #71067, #1292, #14254, #27500, #56398, #63986, #43112, #37721, #92826, #27989, #85721, #57338, #64467, #87906, #7136, #1752, #30639, #64925, #30174, #59538, #52409, #82221, #68488, #53335, #75131, #18290, #38662, #53815, #24457, #89301, #81744, #25389, #89775, #81284, #3624, #60928, #17375, #46685, #68963, #16895, #46227, #2695, #74663, #10241, #67566, #45752, #82683, #10710, #32964, #47148, #3150, #76056, #23993, #23539, #39110, #11186, #4093, #52866, #68023, #9787, #32512, #24938, #16430, #31118, #45282, #17833, #40046, #61857, #31577, #60004, #32033, #88844, #61408, #75587, #74185, #90240, #39567, #54269, #83139, #9304, #38185, #67100, #2234, #60466, #85496, #12122, #27271, #91652, #62818, #55227, #92582, #63284, #25848, #70835, #34379, #26805, #20166, #42392, #84082, #55691, #69890, #48089, #84542, #40967, #19231, #56158, #77942, #6434, #20643, #70381, #49513, #91167, #90688, #19689, #78405, #71304, #26334, #35308, #85015, #27750, #76993, #83607, #5028, #48558, #33909, #5509, #56646, #13544, #5967, #77461, #41924, #34841, #54730, #12603, #41449, #18769, #92117, #49047, #47627, #13086, #63752, #76531, #11653, #40500, #69419, #4550, #33424, #62328, #43341, #35780, #30067, #93519, #36699, #7809, #58494, #14483, #57564, #87800, #28220, #79348, #21100, #87339, #29616, #57108, #14935, #37165, #29138, #8737, #64234, #65152, #28678, #66074, #58952, #85948, #49968, #36234, #65619, #21562, #255, #73165, #43790, #730, #78859, #51361, #1186, #6905, #22949, #50445, #14010, #51823, #22488, #93064, #58032, #80715, #64693, #42869, #71783, #86407, #86886, #8285, #73625, #22040, #80252, #79793, #15388, #44725, #15869, #50909, #72690, #72238, #7352, #44254, #82104, #2120, #10603, #46580, #16782, #68379, #17262, #88276, #1644, #46121, #31469, #3510, #53222, #89659, #59425, #75024, #32401, #30524, #45636, #61300, #23432, #38072, #37614, #90136, #3041, #24827, #60816, #31010, #39462, #66983, #38558, #52300, #9194, #81635, #31924, #81177, #59897, #25286, #53711, #54163, #88739, #23885, #74545, #83032, #89194, #52753, #18186, #47038, #10137, #9675, #39003, #16321, #45173, #74075, #75939, #67460, #2589, #66525, #82578, #67917, #60357, #17725, #75478, #24347, #27159, #20538, #84433, #47517, #56533, #33318, #25739, #12485, #92006, #68854, #39937, #54621, #77351, #56047, #41336, #19581, #70270, #4909, #27634, #11545, #40392, #48450, #90579, #12011, #11068, #83977, #26696, #76884, #40861, #84901, #5404, #69310, #34269, #76423, #85389, #19125, #63176, #91540, #47980, #20050, #48931, #83493, #3983, #77828, #4438, #69779, #62214, #70727, #91044, #12978, #41816, #5859, #55111, #26217, #34730, #32858, #33795, #61747, #63646, #92468, #18651, #55585, #49408, #62709, #22838, #78298, #79232, #42751, #80139, #44136, #6323, #42284, #50325, #50801, #35675, #14373, #87228, #29024, #21928, #35191, #65499, #15279, #20990, #43234, #71668, #29503, #79686, #13437, #85839, #64118, #14828, #65965, #71196, #57457, #49857, #86767, #78756, #22376, #43682, #1076, #51249, #72132, #57911, #36585, #92954, #7248, #58385, #36124, #65041, #73041, #93415, #72578, #144, #7700, #6801, #8171, #618, #28114, #37054, #29956, #58841, #87685, #57002, #64590, #13897, #86300, #28566, #21452, #66861, #16209, #81980, #38889, #61179, #46461, #31351, #75363, #52182, #51705, #52635, #10478, #3385, #81064, #32273, #46003, #53590, #37954, #44609, #1996, #9548, #45060, #60239, #82462, #17610, #31808, #73960, #2923, #60701, #39344, #74419, #81515, #90016, #38435, #67343, #80593, #9074, #53103, #23770, #89541, #89077, #30889, #24226, #88151, #68263, #59781, #74907, #2474, #24704, #88623, #1526, #15750, #17137, #73514, #16662, #8623, #45517, #66409, #37500, #10019, #67798, #30412, #59303, #23310, #62580, #40743, #19465, #5743, #84783, #54982, #69660, #19933, #48801, #26093, #4791, #83378, #91886, #34153, #4326, #55929, #33670, #75823, #82914, #91422, #19010, #77710, #26575, #77233, #46921, #55464, #12860, #18068, #33203, #41698, #10947, #25624, #25170, #70616, #84314, #12363, #48332, #18526, #27040, #54506, #83858, #39813, #90467, #69197, #41210, #68735, #47392, #34618, #70148, #63528, #76303, #11428, #62094, #54044, #76766, #40280, #3866, #32746, #5284, #90928, #63057, #61634, #47863, #11894, #36950, #49287, #85270, #92355, #79583, #14265, #28456, #14725, #7592, #20419, #43578, #8058, #72029, #35079, #44031, #20877, #13321, #38, #72476, #56409, #27516, #42161, #64937, #36478, #28918, #7145, #57806, #86191, #15173, #92836, #27999, #36019, #78183, #93306, #71078, #71554, #43125, #64478, #86656, #49749, #57351, #65395, #21821, #50696, #6210, #507, #29390, #63997, #21343, #56891, #58282, #87124, #85731, #78646, #13786, #22276, #80032, #42638, #6690, #35565, #51148, #50214, #72933, #79117, #82357, #9919, #37856, #45417, #24124, #971, #30781, #17032, #1890, #23671, #60599, #80962, #2372, #66760, #59680, #30307, #67696, #38328, #29852, #45897, #9442, #88523, #88976, #17505, #59195, #52537, #44958, #23198, #81412, #16106, #88043, #31250, #53003, #75259, #89434, #74317, #24592, #66308, #65863, #16562, #53480, #46358, #1423, #10374, #60137, #2824, #52079, #58736, #73858, #67242, #8976, #81877, #31707, #87579, #74802, #38792, #22723, #51598, #80486, #15634, #44503, #73409, #8519, #37398, #39241, #3760, #40632, #47277, #62464, #91305, #82810, #68157, #26468, #39703, #18417, #10839, #5168, #68626, #11782, #76655, #33554, #83273, #32645, #62946, #3277, #54400, #89913, #55357, #4680, #32170, #83745, #12251, #4219, #77596, #61070, #40174, #61533, #41097, #34043, #25069, #53941, #11323, #70026, #17961, #76193, #91780, #46814, #90364, #75716, #26931, #84209, #19356, #48220, #25521, #55819, #69093, #33094, #61985, #90820, #25980, #77122, #54865, #18902, #84675, #19824, #48690, #47757, #69550, #56780, #29274, #64369, #78073, #36367, #65280, #50099, #85622, #21230, #34511, #70509, #63418, #51033, #92247, #5636, #12745, #93649, #28347, #42524, #28809, #21705, #27404, #57693, #22165, #86079, #49179, #58169, #34970, #56292, #14148, #86536, #85156, #41587, #20308, #78993, #50581, #43012, #71916, #7037, #6573, #87013, #13216, #42052, #35907, #70966, #13674, #6098, #20768, #57237, #78535, #71436, #79476, #64825, #63884, #14611, #92720, #27890, #49640, #43468, #93195, #72365, #35450, #7482, #385, #82896, #45501, #75347, #11412, #17121, #31335, #74403, #45987, #17595, #25607, #26076, #82447, #54029, #32258, #10929, #90910, #76286, #46445, #61163, #40263, #69180, #10462, #90000, #74892, #83358, #54490, #89525, #47372, #25155, #67327, #9533, #18052, #39328, #4309, #46904, #68719, #38418, #75805, #68246, #39797, #67781, #3370, #18508, #3849, #32730, #2459, #61618, #33187, #53086, #90450, #10003, #62077, #54965, #60222, #24211, #89061, #16647, #81965, #38874, #53572, #2907, #31791, #60685, #27984, #56393, #6672, #56875, #55914, #63512, #42144, #18994, #48787, #35061, #19916, #41682, #78629, #5268, #20403, #84766, #77695, #48316, #85716, #85255, #47847, #63981, #27495 ),
 ( #49273, #26560, #35549, #91871, #13306, #70600, #20861, #70132, #33655, #42620, #78168, #76749, #12844, #13771, #84300, #4773, #11877, #19450, #5727, #92821, #93289, #34602, #71062, #92340, #6194, #64462, #49732, #71539, #28440, #83841, #40728, #69645, #62564, #77217, #91405, #55449, #63040, #12345, #41194, #34137, #27025, #8040, #51134, #23179, #956, #37381, #79100, #29835, #52062, #21326, #65378, #80944, #43107, #57790, #57333, #16089, #50196, #59178, #66742, #58718, #23, #8957, #79567, #72014, #87562, #44941, #14249, #86175, #7131, #37836, #1868, #36002, #64920, #28902, #80017, #86640, #21808, #50681, #14710, #43563, #58268, #72459, #36463, #7578, #44016, #490, #10823, #39221, #31232, #3260, #67223, #47260, #38774, #53925, #17487, #3744, #17008, #74297, #83257, #32150, #59662, #89416, #25503, #60118, #45398, #88505, #88957, #31686, #39683, #40158, #2804, #68139, #46339, #25052, #11306, #90347, #60581, #75241, #54381, #18401, #24570, #10356, #24104, #32626, #68607, #9900, #61516, #61051, #81394, #23652, #89894, #53458, #76174, #82793, #17945, #52518, #46796, #69075, #16542, #67678, #30760, #9421, #52985, #38308, #2354, #75698, #81859, #45877, #74783, #82339, #33538, #5149, #25963, #69532, #48202, #63401, #61967, #4665, #63867, #85135, #85605, #62443, #91286, #77104, #20752, #55803, #26452, #27871, #56764, #41570, #12235, #12727, #54844, #90804, #83726, #42508, #18886, #47741, #4203, #20290, #19807, #34026, #49164, #13199, #76639, #77576, #34955, #11764, #41082, #92701, #40616, #55341, #33078, #49623, #92230, #78057, #27386, #84192, #6081, #19340, #62930, #70006, #91764, #26916, #56276, #84655, #48675, #78519, #42035, #13656, #70492, #5620, #34495, #70949, #29253, #42993, #2587, #31467, #15040, #50561, #79902, #93179, #35431, #28331, #17260, #57221, #64353, #71420, #59895, #86995, #7464, #88737, #81633, #86061, #23883, #82101, #51015, #14128, #24345, #93632, #21211, #72797, #52751, #50081, #6552, #78976, #43900, #16780, #7921, #36812, #65733, #65261, #89192, #71899, #7019, #844, #35890, #72346, #64808, #79458, #22147, #43449, #36347, #45634, #29725, #28789, #74542, #57676, #53220, #14592, #9673, #58149, #38556, #86519, #21684, #60355, #67458, #367, #3039, #53709, #10135, #75022, #46119, #31922, #60814, #39001, #67915, #89656, #24825, #82576, #35870, #22129, #7446, #71401, #86041, #36328, #65242, #42488, #21190, #6062, #14574, #50540, #20733, #72325, #50061, #92212, #5602, #78957, #35410, #348, #57200, #93612, #14107, #34934, #43430, #79438, #49603, #29235, #42971, #27368, #34476, #71876, #64330, #58130, #6998, #28770, #63382, #64787, #86975, #56257, #78499, #50997, #85117, #42015, #41550, #79882, #57653, #86501, #21664, #63849, #70474, #70931, #6534, #20267, #13180, #85586, #49143, #78040, #92681, #27851, #56740, #13637, #93156, #28311, #59040, #31556, #66609, #80339, #38645, #67548, #52389, #87887, #23520, #36793, #72778, #65713, #53317, #825, #7903, #15022, #2215, #30619, #44812, #31099, #23974, #29706, #59986, #24435, #88370, #51449, #60448, #37254, #58589, #16411, #88825, #87428, #43882, #22575, #81266, #52848, #45263, #74167, #9283, #8824, #89283, #15481, #44352, #38166, #73262, #15957, #8374, #23040, #59521, #80808, #73714, #81725, #67081, #66159, #16874, #1275, #30157, #51918, #45732, #1732, #74643, #37704, #9769, #2677, #54710, #17356, #47126, #76973, #82662, #3131, #46207, #17811, #83121, #91146, #91633, #54251, #25831, #4075, #76512, #62798, #48070, #18272, #32946, #12103, #40948, #76039, #61838, #69870, #5008, #11168, #90671, #46664, #55208, #26313, #61389, #19211, #83587, #39089, #75112, #18751, #40028, #33891, #47609, #40481, #10222, #11635, #26787, #68002, #90221, #82201, #32011, #75568, #60909, #89756, #69398, #4530, #33407, #10690, #84062, #39547, #68945, #24917, #53794, #32492, #62306, #68470, #3605, #25370, #42852, #72222, #13069, #84993, #92561, #48540, #42375, #27254, #79332, #12585, #93046, #85479, #64216, #41432, #70364, #5489, #34362, #63267, #92098, #56140, #71768, #71287, #20626, #64678, #28660, #41905, #21544, #70818, #35289, #49497, #78386, #6414, #28203, #57091, #50427, #85931, #21081, #49952, #1626, #16305, #59404, #37596, #23416, #22934, #45619, #29600, #58479, #81161, #14919, #87784, #29119, #8270, #44707, #1170, #51804, #9176, #38054, #87323, #66963, #715, #74521, #37150, #30993, #73608, #59880, #15373, #72675, #38541, #88720, #58015, #80696, #23868, #22471, #51343, #22025, #44235, #52734, #67444, #79776, #73144, #66057, #18167, #90563, #76868, #62198, #32382, #82083, #3022, #2571, #33300, #61731, #83476, #25721, #89638, #4422, #31908, #3489, #24328, #67899, #46562, #54605, #60339, #60800, #91028, #18632, #83960, #24808, #53694, #75461, #19109, #54146, #82561, #26197, #55091, #39918, #10582, #11048, #53205, #89176, #17241, #40842, #46103, #75008, #31450, #47498, #47020, #61283, #76407, #11529, #10120, #40376, #11993, #75922, #38986, #47964, #17709, #39445, #3967, #69293, #68361, #90117, #25269, #68839, #83015, #32841, #49390, #35175, #63628, #86283, #70252, #5387, #78282, #55568, #70711, #69761, #48910, #85372, #41800, #5842, #49841, #13420, #34252, #42265, #12468, #21436, #77812, #92937, #56513, #42734, #56027, #19564, #28551, #71178, #4892, #34714, #64574, #63158, #84416, #33776, #91989, #92453, #78738, #79215, #27616, #6307, #20522, #64097, #50310, #35659, #28098, #56985, #93399, #57442, #85823, #20974, #27142, #71649, #13881, #12961, #6782, #14358, #26678, #62689, #91522, #48430, #77334, #41315, #84882, #20033, #22820, #73944, #7235, #51235, #9059, #36110, #15262, #15731, #603, #73025, #52165, #87670, #80578, #128, #30396, #37937, #79673, #8153, #7686, #88134, #44592, #72119, #50788, #65028, #73496, #30872, #81500, #22361, #14814, #51689, #43669, #81048, #8608, #59766, #16191, #44121, #37484, #1510, #29011, #37036, #23292, #65950, #1061, #66846, #58371, #66394, #29940, #58825, #36571, #45043, #59288, #57896, #1981, #88607, #23755, #52618, #43218, #65486, #86752, #80123, #29486, #21914, #87213, #72564, #85732, #42639, #64938, #50215, #35080, #79118, #84784, #55466, #56410, #14266, #7146, #19934, #36021, #49750, #57352, #41700, #48333, #70617, #13322, #48803, #63998, #86192, #21344, #35566, #77711, #6691, #64480, #43126, #78184, #85271, #39, #42163, #71079, #84315, #12861, #56893, #63529, #78647, #13787, #5285, #19466, #71555, #5744, #34619, #27041, #72031, #92356, #28000, #92837, #93307, #27517, #20420, #77234, #12364, #49289, #41211, #28457, #20878, #70149, #6211, #34155, #63058, #91887, #28919, #29853, #87126, #30782, #88524, #50697, #45418, #29391, #58283, #37399, #14726, #58737, #57807, #8059, #44504, #972, #87580, #8977, #66309, #22277, #1424, #65396, #74318, #36951, #52080, #15635, #1891, #15174, #72477, #81413, #30308, #86657, #22724, #23672, #51149, #43579, #21822, #80033, #51599, #37857, #38329, #80487, #59196, #73410, #23199, #9443, #52538, #8520, #88044, #16563, #67243, #80963, #16107, #44032, #59681, #66761, #65864, #79585, #44959, #7593, #36479, #73859, #508, #72934, #17962, #54401, #24125, #75717, #33096, #60138, #10375, #61987, #81878, #2825, #2373, #90822, #61534, #83274, #25522, #89435 ),
 ( #53004, #40634, #17033, #88977, #31251, #18418, #46815, #32171, #47278, #11324, #45898, #76194, #11784, #10840, #38793, #47759, #24593, #74803, #3761, #40175, #9920, #67697, #31708, #68627, #69094, #32646, #39704, #90365, #89914, #25982, #60600, #53481, #3278, #54867, #76657, #82358, #17506, #4221, #83747, #46359, #75260, #39242, #53942, #68158, #18904, #61071, #25070, #82811, #62948, #20770, #49642, #57239, #92249, #5638, #14150, #27406, #85158, #69552, #34045, #70968, #77598, #92722, #27892, #19358, #4682, #56782, #70028, #48692, #41099, #35452, #5170, #42054, #13218, #63886, #19826, #91782, #93197, #33556, #84677, #26470, #85624, #34972, #62466, #20310, #42526, #34513, #91307, #55359, #70511, #26933, #71438, #64371, #84211, #48222, #41589, #6100, #55821, #63420, #78537, #49181, #13676, #77124, #6575, #28349, #12253, #56294, #12747, #86081, #21232, #78075, #50101, #78995, #16801, #31944, #82595, #22167, #50583, #52774, #79478, #82125, #45657, #60835, #17282, #16341, #23903, #2607, #71918, #9213, #89214, #74094, #2139, #39021, #58171, #74565, #45191, #38093, #7484, #46139, #9694, #7039, #24365, #81653, #67003, #67478, #89679, #36369, #31028, #51035, #387, #59915, #87015, #65282, #38575, #31487, #53729, #67936, #60375, #88757, #3059, #43470, #57695, #35909, #72367, #53243, #75042, #43014, #10154, #24846, #64827, #93651, #28811, #86538, #21707, #14613, #29276, #81195, #18669, #62230, #75957, #84448, #26712, #90596, #48466, #91061, #68397, #75495, #26235, #11560, #77366, #33333, #69794, #39477, #55128, #12502, #10619, #25756, #41354, #3527, #18202, #17742, #70286, #76899, #4927, #40876, #11088, #19598, #47054, #47535, #32417, #83050, #61763, #12029, #61316, #39954, #5419, #33813, #34284, #68870, #4000, #54637, #63192, #69326, #32875, #92022, #27177, #83993, #83511, #19140, #90154, #25302, #54180, #56064, #76439, #40408, #46596, #62725, #47995, #4455, #91555, #55600, #77846, #7265, #638, #64606, #27652, #36602, #13453, #5877, #86317, #72149, #48948, #20067, #34747, #57476, #36142, #21469, #93432, #50345, #78773, #7718, #85406, #20554, #28584, #70743, #85855, #84917, #64139, #6818, #57019, #21008, #65061, #79251, #49424, #14392, #56551, #65519, #92972, #43251, #71688, #57932, #71213, #63662, #43699, #162, #12994, #78314, #49875, #42304, #29041, #86788, #41832, #92485, #6340, #21947, #72598, #29522, #28130, #35211, #50820, #13914, #79704, #14846, #42769, #35692, #30427, #37969, #16678, #87248, #23328, #9565, #88169, #16224, #53118, #73529, #88638, #59318, #52198, #22854, #60255, #30907, #22394, #38453, #2014, #81080, #81530, #10034, #51720, #45075, #37515, #15768, #73975, #8638, #80610, #23786, #45533, #67813, #81998, #66877, #17154, #58857, #58402, #9092, #46020, #38904, #87703, #2938, #52650, #89092, #44627, #51266, #66425, #59797, #1544, #74434, #24244, #74923, #67359, #2489, #31366, #80159, #15297, #44154, #73061, #8191, #37072, #65981, #1092, #29973, #33215, #39826, #54999, #83871, #75379, #31824, #19023, #32290, #10959, #3399, #91437, #61195, #4338, #69209, #26106, #75836, #25184, #55479, #89554, #46934, #82477, #47877, #90942, #24722, #76316, #4805, #90479, #70163, #60715, #32758, #90032, #33685, #26589, #53606, #17624, #3880, #62111, #82927, #61646, #40756, #11442, #76780, #46475, #11907, #62594, #10492, #84328, #69674, #39361, #25636, #19478, #54057, #68277, #18080, #68750, #54520, #48345, #41224, #83389, #77248, #47406, #12377, #18539, #40293, #55940, #84796, #12873, #41712, #27054, #19946, #63070, #77723, #5298, #48817, #34168, #91900, #51363, #58496, #45175, #88279, #31471, #16324, #52755, #22490, #74077, #60359, #87341, #8739, #89196, #80254, #1188, #732, #24349, #59899, #81637, #23887, #87802, #2591, #30069, #1646, #15390, #66076, #44727, #88741, #44257, #58954, #53224, #16784, #82106, #22951, #51825, #73627, #17265, #52302, #80718, #46123, #75026, #38074, #37616, #9196, #73168, #8287, #37167, #39005, #15871, #66527, #29618, #45638, #66985, #30526, #74547, #9678, #59428, #38560, #10139, #2123, #23434, #81179, #31012, #67462, #69311, #55113, #31926, #3043, #82580, #40393, #83978, #4439, #47519, #33319, #61748, #84434, #68380, #3511, #76424, #53713, #68855, #67919, #47039, #83494, #39939, #3984, #47981, #11546, #32403, #62215, #10605, #19582, #75940, #91045, #54622, #40862, #54165, #26219, #89661, #19126, #4910, #60818, #11070, #33797, #17727, #61301, #24830, #62711, #76885, #12012, #69780, #90137, #91541, #25287, #32859, #46582, #39463, #18187, #26697, #75480, #83033, #55586, #48451, #77352, #90580, #25740, #18652, #12486, #92956, #12979, #65042, #145, #78757, #20539, #49858, #63177, #5405, #92008, #79687, #27160, #34270, #41337, #28568, #57003, #71197, #57458, #50326, #56048, #86301, #50802, #20992, #77830, #86769, #63647, #84902, #42752, #21453, #20051, #70272, #48932, #13898, #79233, #71669, #6803, #35676, #35192, #57912, #41817, #70728, #64591, #5861, #42285, #34731, #49409, #85840, #13438, #6324, #14375, #93416, #92469, #43235, #27635, #21930, #78299, #72133, #28115, #7249, #56534, #85391, #29025, #36125, #64120, #73515, #9549, #15280, #29504, #72579, #44137, #15751, #23771, #24227, #80594, #52184, #30413, #9075, #89078, #74420, #44611, #59304, #38436, #67345, #8624, #88152, #73042, #81516, #52636, #87686, #45518, #23311, #65500, #7701, #81065, #37501, #2475, #16210, #58843, #31352, #66410, #80140, #60240, #53104, #45061, #22839, #73961, #36586, #619, #58386, #14829, #87229, #22377, #43683, #1997, #37955, #1527, #30890, #16663, #51250, #59783, #8172, #66862, #37056, #65966, #1077, #29957, #88624, #51706, #46004, #17138, #2924, #54507, #69198, #83379, #61635, #47393, #75824, #4793, #82464, #17611, #90468, #67799, #82915, #81982, #61180, #3868, #54045, #18069, #62096, #25625, #46462, #18527, #24705, #33671, #90018, #11430, #68737, #54983, #68264, #31809, #40744, #76304, #74909, #46922, #76767, #75365, #60702, #10020, #10479, #10948, #90929, #91423, #39814, #40281, #32747, #4327, #62581, #47864, #33204, #26094, #11895, #69661, #83859, #19012, #39345, #26577, #38890, #25171, #89542, #53591, #3386, #32274, #93361, #42695, #79637, #64536, #7200, #70674, #28512, #14779, #12922, #56949, #43632, #34677, #49349, #48871, #72530, #14322, #36075, #72084, #42224, #50753, #78244, #49806, #5803, #20483, #92900, #43182, #41763, #13381, #7649, #64993, #36534, #71138, #6267, #21397, #85332, #65449, #85786, #96, #35621, #21881, #35135, #92415, #565, #50268, #77775, #13844, #29450, #64058, #63591, #27575, #28059, #78702, #57860, #58338, #20937, #86246, #57406, #28975, #87180, #56473, #71614, #79177, #6748, #86716, #44086, #8119, #80088, #1030, #29908, #72989, #58792, #37005, #22329, #51200, #15230, #65918, #48497, #33361, #69825, #39505, #91093, #77396, #75523, #25786, #12533, #3556, #18231, #17768, #41384, #76930, #4960, #40905, #11116, #19628, #47082, #18699, #68426, #83078, #61791, #12058, #10645, #75988, #70317, #33845, #5447, #39983, #68898, #90623, #34315, #69354, #4030, #63221, #92053, #55158, #54667, #26264, #32445, #61346, #90181, #56094, #25329, #54209, #46623, #62754, #62260, #47562, #91586, #26743, #32903, #55629, #27207, #84020, #83540, #76467 ),
 ( #11589, #84478, #40436, #4484, #19168, #48025, #21037, #72176, #191, #77877, #7292, #667, #64633, #27683, #36632, #13484, #5907, #86347, #36171, #48980, #20098, #34777, #57503, #65091, #21498, #93460, #50376, #78800, #7748, #85434, #20583, #28614, #70774, #85885, #84948, #64168, #6845, #57048, #49905, #29072, #79280, #49454, #14421, #56581, #65553, #93000, #43278, #71718, #57964, #71242, #63692, #43728, #86818, #13025, #13945, #79732, #78342, #92517, #41861, #42331, #42802, #21976, #29551, #35719, #50849, #14874, #72627, #6371, #35242, #28158, #9124, #24276, #82032, #59353, #38001, #22886, #31398, #67392, #37547, #89125, #66911, #15327, #22424, #2049, #52229, #53151, #74007, #16710, #80188, #30939, #17190, #51296, #66458, #46052, #44188, #58888, #58431, #74957, #23818, #45565, #81562, #51755, #60288, #87734, #88204, #73093, #30003, #8669, #52681, #8223, #80645, #10068, #74469, #38937, #15800, #44659, #1576, #67846, #16255, #73560, #2972, #87277, #59828, #30458, #88669, #37101, #66010, #1122, #23362, #81112, #2521, #45105, #9600, #38487, #82510, #89587, #76349, #25672, #62631, #47440, #83904, #53640, #11475, #91470, #24758, #39862, #26621, #17658, #32328, #31857, #55512, #90974, #19055, #55035, #25217, #33720, #61230, #32790, #46510, #3433, #75869, #26140, #75412, #90065, #84360, #47911, #19510, #54090, #82961, #10993, #48378, #83420, #18115, #77280, #12409, #69241, #68784, #40326, #10528, #39395, #68310, #70198, #46967, #3913, #60746, #76814, #4370, #61678, #11939, #40788, #90510, #69706, #41259, #33248, #54552, #18575, #62144, #4836, #6731, #86231, #63103, #34199, #19975, #71595, #21382, #35604, #78686, #64519, #92881, #21863, #5785, #34659, #13826, #84826, #6250, #5331, #78226, #20920, #71120, #35119, #79158, #42678, #63573, #93345, #41744, #50737, #13365, #28496, #85770, #72067, #85316, #48851, #57844, #57389, #91931, #64039, #80, #92399, #77756, #27086, #27559, #28043, #14306, #14763, #56933, #50252, #49789, #43166, #79621, #64977, #7184, #36059, #28958, #86698, #43617, #55973, #56454, #12905, #70657, #20465, #49332, #42206, #9013, #73447, #44544, #36988, #74356, #44995, #7633, #52572, #16143, #8557, #1927, #24160, #65900, #66346, #51639, #29892, #1460, #87618, #1012, #37892, #59718, #81916, #67279, #52118, #2409, #72972, #72513, #30346, #31289, #53040, #8101, #17068, #66797, #9479, #58776, #65433, #22769, #59236, #80525, #81000, #38365, #60175, #81452, #15678, #23709, #16600, #89013, #88082, #23238, #36518, #73896, #30821, #547, #88561, #45456, #29430, #58320, #87164, #22313, #51184, #80071, #15214, #44070, #17546, #11826, #75298, #18459, #83314, #40217, #89954, #39281, #69595, #9956, #61115, #2861, #69133, #11365, #38828, #90404, #18944, #10881, #84253, #45935, #46857, #10417, #47798, #40677, #67735, #31744, #18004, #47318, #3319, #75760, #54910, #25561, #76234, #60637, #33139, #76700, #82398, #39744, #68199, #90863, #4261, #74843, #53522, #89474, #62029, #33603, #24635, #25109, #46398, #54441, #32208, #83789, #26027, #62511, #4725, #68668, #91351, #26512, #53983, #3804, #55401, #32685, #82852, #61571, #35013, #85201, #20351, #93238, #27933, #19869, #85665, #55868, #35952, #27447, #42568, #6141, #86125, #5677, #62993, #71961, #20813, #48267, #78120, #14196, #48739, #34091, #77169, #77643, #49223, #28391, #28853, #13258, #56824, #63928, #13716, #93697, #79044, #42095, #92766, #43057, #7079, #71010, #49683, #12794, #21274, #57283, #92290, #50146, #78578, #70076, #12299, #71484, #6616, #64871, #35496, #64411, #41143, #57739, #19404, #5218, #56339, #91824, #26977, #41635, #84720, #70554, #34552, #63460, #16038, #79965, #88455, #22207, #87510, #14659, #58213, #36880, #52005, #50630, #87058, #52470, #73792, #74248, #51077, #15102, #65795, #9370, #44435, #43962, #16492, #45346, #30237, #905, #1354, #43514, #79520, #72412, #31183, #7528, #36413, #86584, #8908, #8452, #22657, #37785, #1820, #65329, #66692, #2300, #66239, #29321, #38254, #72861, #433, #87971, #30706, #7986, #21754, #29787, #59127, #59605, #23122, #80891, #44891, #80419, #67167, #58666, #51530, #23602, #15564, #73341, #37331, #81344, #67629, #4158, #32580, #76594, #33028, #32098, #39634, #18355, #88906, #25007, #11256, #89845, #17897, #54796, #75193, #90303, #61000, #53878, #24522, #61919, #61473, #24056, #40111, #3695, #82744, #83208, #11716, #53403, #46750, #39176, #17439, #75651, #10306, #82288, #25455, #47213, #69484, #83675, #68558, #18837, #60528, #60069, #10774, #47692, #40569, #89364, #4614, #54334, #90755, #46289, #52930, #68087, #76124, #3212, #69026, #25913, #81809, #16958, #45823, #74729, #9850, #38723, #2757, #31638, #71843, #85082, #49110, #33488, #91713, #34902, #41517, #56707, #85553, #77056, #62394, #20701, #33975, #12675, #5096, #93122, #62879, #6028, #70896, #27817, #77523, #26865, #57168, #91237, #48622, #84144, #49571, #92645, #26402, #78007, #6496, #92180, #55290, #19293, #34441, #55753, #35377, #28278, #48152, #12185, #5570, #63813, #84606, #63347, #42454, #13147, #78466, #41028, #13603, #64296, #69954, #27335, #19755, #71366, #86008, #70443, #56222, #20233, #21158, #50027, #41983, #78920, #14069, #42934, #23378, #66475, #38506, #89145, #17675, #2989, #81581, #31875, #7411, #6963, #9141, #60764, #53658, #36292, #82527, #2539, #10086, #88222, #93578, #52247, #59845, #1592, #16729, #38954, #67866, #82050, #30474, #53170, #17207, #89605, #30957, #38018, #46528, #88686, #23834, #35836, #59370, #9619, #16272, #31418, #60307, #50506, #64753, #24294, #81128, #45123, #72290, #24775, #74024, #74487, #45582, #46068, #66928, #2066, #28737, #57620, #52700, #86463, #74974, #67410, #21624, #79404, #14540, #43395, #19992, #75430, #76367, #39881, #77297, #41278, #3453, #39413, #47460, #47928, #32805, #11493, #84379, #26161, #19074, #32348, #62651, #12427, #18131, #40342, #68802, #26640, #76831, #10548, #82981, #61247, #11958, #63121, #68329, #54569, #46985, #83922, #75885, #19528, #40806, #91950, #48394, #69259, #55053, #33738, #90082, #4388, #55530, #33265, #62162, #70215, #90527, #69723, #90991, #4854, #3931, #5349, #91486, #25234, #34215, #27105, #55989, #84844, #54108, #61695, #11011, #25687, #83439, #18594, #13445, #92476, #62718, #77359, #27642, #56542, #33805, #12493, #91052, #5868, #41824, #12019, #63654, #41346, #83502, #90588, #70279, #26704, #85398, #48458, #84909, #54630, #5412, #20546, #25749, #40869, #49416, #18661, #33326, #32867, #78306, #92015, #20057, #56055, #26227, #34738, #62223, #91548, #47527, #4446, #76891, #27167, #76432, #55120, #42293, #48939, #71205, #83985, #19133, #69787, #61756, #84441, #47988, #11553, #40400, #34277, #4918, #63184, #69318, #55593, #19589, #77838, #12986, #70735, #44617, #87238, #21938, #36133, #22385, #15288, #92964, #51257, #15758, #79695, #42759, #51712, #28576, #21000, #7709, #80148, #64129, #35200, #49865, #72587, #44145, #36593, #14837, #65508, #153, #22845, #6810, #35684, #43690, #85847, #7257, #6332, #79242, #50810, #72141, #65050, #73050, #627, #64599, #29512, #71677, #80601, #14383, #58393, #86778, #8180, #86309, #78764, #58849, #37063, #28122, #29033, #1083, #93424, #13906, #57011, #57466, #57921, #65972, #21461, #29963 ),
 ( #50335, #43243, #87692, #89084, #9556, #60707, #82469, #66416, #89547, #82920, #53110, #16216, #25176, #2004, #88159, #74915, #24711, #37507, #8630, #23318, #46010, #53596, #10026, #81989, #38896, #67351, #90023, #73967, #9081, #17144, #59310, #74426, #73521, #52642, #24233, #45524, #38443, #17616, #67805, #37961, #2929, #45067, #54050, #81522, #31814, #60246, #46467, #59789, #52190, #32280, #75371, #1534, #2481, #68269, #66868, #81071, #30419, #30897, #31358, #10484, #18074, #39350, #3391, #61185, #88630, #23777, #16669, #76773, #91429, #12867, #70623, #47871, #26583, #11436, #19940, #55935, #26100, #77717, #55473, #3873, #10953, #84322, #40750, #41706, #62587, #5291, #68743, #19472, #5750, #39820, #54990, #34625, #32752, #47399, #46927, #63536, #12370, #34161, #70155, #40286, #48811, #76309, #11901, #61640, #48339, #75829, #69203, #77240, #83865, #63064, #91893, #90473, #25630, #27048, #4332, #19018, #18532, #92362, #33209, #41218, #84790, #27524, #90935, #62103, #56417, #54512, #69667, #83384, #85276, #4799, #33678, #64944, #87132, #79125, #58743, #20426, #21350, #78653, #22283, #80040, #42171, #78190, #86198, #86664, #71562, #50221, #29397, #45, #57813, #71085, #7598, #51155, #56899, #14272, #13793, #65402, #21828, #49295, #28006, #6217, #50703, #8066, #13328, #93313, #85738, #28925, #20884, #58289, #79591, #36956, #15181, #43132, #14732, #72483, #35086, #72037, #515, #7152, #36027, #44039, #35572, #43585, #36485, #72941, #42645, #65870, #978, #64005, #29859, #92843, #49756, #6697, #64486, #28463, #57357, #66766, #44965, #81418, #8983, #52086, #24129, #74808, #3282, #82362, #67247, #17511, #88050, #87586, #88529, #46363, #39246, #23206, #68162, #81882, #89439, #73865, #80493, #37862, #45423, #80969, #2377, #24597, #53486, #67701, #16114, #38797, #2829, #75264, #16568, #23677, #32175, #74323, #31712, #22731, #59686, #31255, #9447, #17037, #51605, #10379, #52543, #38333, #15641, #44510, #60142, #88981, #1897, #60604, #73416, #30788, #8526, #53007, #37405, #66315, #45903, #9924, #1430, #30314, #59203, #82815, #40638, #91787, #25074, #69098, #26938, #46819, #61538, #61076, #55826, #26474, #48227, #84215, #54405, #62953, #90370, #61991, #17966, #32650, #11328, #55363, #53947, #25526, #84682, #77129, #48698, #83278, #18422, #40179, #77603, #18908, #47282, #19831, #12753, #4686, #4225, #69557, #75721, #10844, #39708, #5643, #68632, #3765, #89918, #12259, #76661, #90826, #41103, #70033, #76199, #5176, #70516, #33560, #33101, #41594, #25986, #54871, #62470, #34050, #83752, #47763, #11788, #91312, #19363, #35914, #14155, #93656, #28354, #51040, #34977, #63891, #43020, #20316, #35458, #34518, #13681, #50106, #6580, #64376, #14618, #71923, #92726, #7044, #70973, #79927, #42532, #57700, #21237, #7489, #20775, #78080, #87020, #64832, #63425, #93202, #29281, #27898, #49186, #92254, #56787, #57244, #36374, #43475, #71443, #65287, #79001, #85163, #27411, #28816, #86086, #392, #86543, #21713, #56299, #50589, #58178, #13223, #79483, #22172, #42059, #85629, #6106, #15064, #72372, #43926, #72822, #49647, #78542, #37296, #8869, #29749, #73306, #51963, #67127, #65760, #8417, #67592, #88869, #89328, #66202, #1318, #80855, #24483, #59567, #30200, #31602, #60491, #45307, #16002, #16455, #58630, #870, #87471, #46252, #22618, #51493, #7947, #24018, #23567, #37747, #52892, #16921, #80381, #81771, #17404, #81309, #44397, #53362, #59090, #15522, #9331, #45779, #87932, #36842, #23083, #74212, #74690, #38213, #2263, #31145, #1781, #82248, #44854, #73757, #60032, #66655, #30665, #88417, #52434, #9814, #38687, #2722, #55254, #83635, #75614, #47657, #17860, #91678, #83168, #4577, #61884, #48117, #61436, #24968, #33938, #76558, #10268, #40074, #69917, #10738, #89805, #39138, #39595, #76084, #84109, #84569, #47175, #18798, #90716, #69447, #55718, #40994, #11216, #25876, #5055, #62845, #68991, #54758, #68517, #3653, #32544, #11681, #60954, #4121, #75156, #54296, #40531, #32993, #33452, #19259, #62354, #90267, #91195, #46711, #26830, #18319, #26363, #77020, #12149, #25418, #53843, #19716, #68049, #3176, #32060, #82709, #49072, #63312, #12631, #77971, #49538, #57587, #59323, #20666, #85974, #64261, #42895, #30432, #14509, #78432, #93091, #43365, #72261, #13569, #28245, #13113, #21590, #86431, #27778, #79372, #57132, #5534, #41477, #21124, #42419, #7378, #49992, #6930, #70409, #78887, #36259, #34405, #56672, #65179, #92143, #41949, #48587, #1549, #14034, #35803, #71808, #70862, #50469, #5993, #71331, #27298, #20193, #92608, #64716, #56185, #34866, #88175, #93543, #77487, #63779, #85521, #6461, #85044, #35335, #28702, #46939, #75841, #60720, #2494, #31829, #45080, #81085, #73980, #61651, #9097, #16229, #23334, #10497, #38909, #53123, #39366, #32296, #37974, #68282, #32763, #2943, #59802, #68755, #45538, #66882, #24729, #3404, #2020, #52203, #30912, #89559, #61201, #53611, #82482, #17629, #17160, #39832, #90037, #88643, #18085, #46481, #10964, #23791, #52655, #24249, #3886, #81535, #16683, #74439, #75384, #25189, #9571, #38458, #67364, #74928, #31371, #54062, #82933, #60260, #89097, #82003, #46025, #10039, #67818, #19484, #26594, #35096, #48350, #12383, #90484, #55005, #91905, #4810, #19951, #48822, #40299, #25642, #77729, #90947, #69679, #62116, #56426, #26111, #63075, #34173, #84801, #40761, #83877, #20437, #54525, #11912, #47412, #12879, #55946, #83394, #41229, #63545, #55484, #18544, #76321, #91443, #19028, #92374, #85288, #11447, #69214, #62601, #27059, #47882, #84333, #5761, #70169, #41717, #4343, #70633, #27533, #33220, #77253, #76786, #34634, #49306, #33690, #5303, #78200, #13339, #42180, #71093, #6226, #71572, #72493, #6708, #8079, #36497, #80505, #36967, #36038, #43597, #22293, #92854, #28937, #15191, #56, #21839, #58755, #79134, #524, #64955, #57823, #28474, #65880, #65414, #28017, #44051, #7609, #86674, #87143, #15653, #57367, #50715, #43143, #21361, #79601, #14283, #86209, #29409, #72047, #989, #49767, #64496, #64014, #29871, #58299, #51164, #80051, #50230, #87597, #93322, #14742, #85748, #35581, #7163, #72952, #56908, #22743, #51618, #44523, #73427, #8537, #20895, #78662, #13803, #42655, #8994, #61093, #89932, #74820, #16578, #45914, #59214, #1440, #88060, #75736, #23217, #30325, #37416, #24614, #53018, #67257, #53500, #46376, #52097, #82376, #46834, #17048, #73876, #82829, #59697, #80981, #38809, #17526, #16124, #66327, #44975, #9935, #75276, #67713, #2843, #31725, #31267, #53962, #37872, #66777, #60616, #1908, #38344, #30798, #45434, #81896, #9458, #2389, #10395, #89454, #88540, #39260, #23689, #17982, #74334, #68175, #24140, #3296, #52553, #81429, #25088, #32187, #60154, #88993, #26958, #18438, #61551, #68647, #47296, #54888, #70055, #12772, #83767, #62489, #69574, #84233, #41614, #55849, #18923, #4703, #91806, #84702, #47777, #33580, #76213, #34070, #5197, #90842, #62972, #91329, #32664, #39723, #26491, #76679, #19849, #55381, #48247, #90385, #19383, #48720, #3781, #10860, #77149, #4238, #25540, #11804, #40196, #77623, #54421, #11342, #69113, #33118, #83292, #62007, #26003, #40655, #12279, #41123, #18282, #2226, #31110, #10233, #81277, #2688, #1744, #74656, #17368 ),
 ( #11179, #67559, #39101, #46219, #89768, #76048, #61400, #31569, #75123, #90232, #25381, #60459, #68013, #59997, #68480, #10701, #9780, #32503, #3142, #52400, #59532, #32024, #89294, #54261, #60921, #53807, #23531, #24930, #83131, #88381, #38655, #47138, #16423, #88836, #30632, #40039, #82675, #17824, #46677, #23986, #3616, #52859, #24449, #45275, #67093, #45744, #75580, #74178, #81737, #9296, #39558, #38178, #16887, #53328, #82214, #85488, #26797, #40492, #92572, #27742, #12595, #48080, #77451, #90681, #32957, #25841, #13536, #54722, #61850, #68955, #56150, #84534, #5020, #85005, #77935, #83598, #20159, #19681, #27263, #18761, #48550, #5959, #47619, #76985, #34833, #76522, #69410, #4086, #63744, #34371, #49039, #92109, #62318, #70827, #4541, #69881, #11645, #33416, #19222, #63276, #91158, #26323, #56638, #13078, #20635, #55218, #84072, #12114, #49505, #55683, #40959, #78395, #33901, #41441, #62808, #70373, #91643, #5498, #41914, #80708, #93056, #35300, #42384, #29609, #58025, #72231, #58487, #51354, #64226, #87332, #51815, #22033, #78852, #87793, #64686, #57100, #43783, #22480, #6425, #71297, #85940, #14928, #80244, #72683, #50902, #7802, #36227, #58945, #42862, #71776, #79786, #28212, #43334, #21091, #21554, #86879, #14476, #7345, #15381, #36689, #6899, #65611, #14002, #22942, #50438, #723, #29129, #44245, #28670, #49961, #1179, #73155, #35773, #93512, #8278, #57555, #37158, #86400, #79341, #65145, #66067, #246, #30060, #53214, #31460, #10129, #90127, #75470, #45628, #60349, #10593, #39454, #16774, #89186, #74068, #82569, #24819, #88729, #46572, #24339, #66518, #73617, #82094, #9667, #68371, #3501, #74535, #17254, #32393, #61292, #38550, #46113, #9187, #17717, #53702, #23877, #25278, #75016, #1637, #8729, #38995, #67453, #54155, #67907, #3033, #37605, #31916, #15858, #30518, #52745, #44717, #59415, #16314, #88269, #23425, #60808, #89649, #52291, #38065, #81170, #45166, #2581, #66974, #2113, #59889, #31003, #81627, #83484, #48922, #70262, #70720, #47509, #18642, #33310, #5852, #40853, #54613, #12970, #41809, #26688, #62206, #91531, #11059, #47028, #39929, #27626, #68847, #75931, #83024, #5396, #4901, #19117, #34261, #91998, #3975, #63168, #92462, #62701, #25731, #34723, #11537, #32850, #84425, #27151, #61739, #18178, #90571, #55577, #56039, #19573, #48441, #77343, #76876, #63639, #76415, #40384, #12477, #69302, #83969, #4430, #91036, #33787, #55102, #47972, #84892, #41327, #26208, #20042, #12003, #69771, #77821, #79680, #43227, #29496, #42744, #6316, #15273, #29019, #85382, #65960, #7243, #64109, #57906, #20531, #56994, #57451, #65494, #1071, #28560, #138, #72127, #50796, #37048, #35668, #13890, #50319, #71660, #20983, #86761, #43677, #56525, #51244, #36119, #80133, #85832, #49400, #86293, #44131, #8165, #49850, #78291, #14823, #58379, #6793, #13429, #64583, #14367, #78749, #65036, #87223, #22370, #36580, #93408, #7695, #613, #21446, #73036, #42276, #71189, #21922, #72573, #35184, #79225, #92947, #28107, #53097, #81975, #73508, #29951, #17131, #30407, #9069, #1520, #89535, #59298, #2469, #67338, #24221, #73954, #23303, #53583, #87680, #45055, #80588, #45997, #89072, #22832, #74413, #2918, #88618, #58835, #51700, #30883, #88146, #31802, #24699, #15744, #44604, #1991, #31346, #81059, #59776, #38884, #9543, #60234, #8618, #74902, #60696, #66404, #23765, #52177, #10014, #67793, #37495, #16204, #37948, #17605, #46456, #66856, #81510, #16657, #38429, #45512, #75358, #10473, #39339, #41205, #69191, #76761, #55458, #32268, #62089, #48326, #33198, #54977, #91882, #18521, #33665, #4321, #90922, #61629, #5279, #69655, #61174, #77228, #40738, #26088, #26570, #48796, #90462, #83853, #91417, #34148, #83372, #90010, #47385, #19005, #32740, #11888, #63053, #27036, #12357, #25619, #70142, #55925, #47858, #84777, #19928, #41693, #4785, #62575, #3380, #54501, #84309, #11423, #19461, #77706, #46916, #25165, #12855, #3860, #76298, #68730, #54039, #40275, #82909, #18063, #75818, #10941, #39808, #502, #34612, #85726, #27508, #33, #36014, #63523, #21338, #43573, #35560, #15168, #70611, #71548, #35073, #72471, #36473, #92350, #56404, #42632, #43118, #27994, #6683, #79576, #50208, #14260, #85265, #57801, #7587, #13316, #64473, #63990, #21816, #72024, #5738, #78178, #20414, #7141, #58277, #49282, #49744, #42156, #79112, #71073, #14720, #64932, #87119, #65389, #93301, #28913, #86651, #6205, #28451, #50691, #57346, #86186, #29384, #20872, #22269, #51143, #80027, #92831, #56886, #78641, #13781, #24116, #81405, #73852, #67235, #89427, #8513, #8969, #23192, #1415, #37847, #59189, #37392, #74308, #31243, #53471, #38785, #23664, #67689, #73403, #44026, #44952, #2817, #24583, #66301, #82350, #65858, #8053, #966, #72926, #29845, #36945, #58728, #60130, #59673, #66753, #88969, #52996, #87573, #81870, #22717, #52530, #80478, #51592, #30302, #15628, #45409, #17021, #88035, #52073, #80956, #16554, #45890, #9434, #38321, #2365, #1881, #60592, #16100, #30774, #74795, #88516, #9912, #31699, #91661, #34388, #84551, #19698, #92591, #27280, #19241, #85024, #55236, #35318, #26814, #41933, #5518, #85505, #5038, #62337, #71313, #20176, #46351, #28228, #63293, #26343, #49056, #75252, #48098, #48567, #27760, #57116, #77470, #56167, #92126, #13095, #93074, #78414, #12613, #77952, #13553, #42402, #41458, #70844, #77002, #20652, #56656, #55700, #49522, #5977, #69428, #10367, #34850, #70390, #6443, #63761, #64243, #40509, #17498, #4559, #33433, #91177, #84091, #12131, #40977, #69899, #33918, #62827, #73176, #15398, #79356, #87810, #21571, #86895, #14018, #57572, #36243, #51371, #49976, #86415, #51833, #8295, #73636, #50454, #14491, #65161, #8747, #43799, #43349, #15879, #44735, #29626, #264, #741, #72246, #87349, #29147, #44265, #37176, #35788, #85956, #66084, #7361, #58043, #22049, #80726, #50918, #58504, #22498, #80262, #79802, #14944, #37624, #78868, #72699, #42878, #1196, #30077, #71791, #36708, #58962, #7818, #30534, #21108, #65629, #22959, #1654, #6913, #64701, #93527, #28686, #31935, #16792, #89205, #68388, #10147, #3051, #16333, #46590, #90145, #2131, #24357, #23895, #10613, #60826, #88287, #66994, #81187, #89670, #47047, #3992, #38568, #31020, #67927, #59907, #3520, #24838, #75948, #32411, #31479, #39013, #17735, #23442, #53232, #39471, #82115, #17273, #54173, #74556, #53721, #60367, #46131, #52764, #61309, #82588, #52310, #25295, #75488, #75034, #83042, #11079, #81645, #18195, #67470, #45646, #39947, #9686, #2599, #68863, #59436, #45183, #74085, #9204, #38082, #88749, #49986, #50930, #8758, #1666, #79367, #30548, #44279, #51844, #36254, #42889, #65173, #7832, #14503, #29637, #80739, #15890, #30090, #43360, #1208, #87822, #79814, #22972, #44746, #88298, #36720, #753, #78880, #22511, #7373, #14955, #73648, #58516, #87361, #6924, #37188, #37637, #21582, #43810, #72256, #66545, #51382, #14028, #57582, #71802, #80273, #59447, #35798, #29158, #50464, #15411, #278, #64711, #73187, #93538, #28697, #22061, #8306, #66096, #58055, #72710, #86906, #53247, #75046, #18208, #38579, #53733, #24369, #89218, #81657, #25306, #89683, #52321, #3531, #60840, #82129, #46600, #68874, #16805, #17286, #2613 ),
 ( #90158, #9698, #67007, #75962, #24850, #81199, #32879, #67940, #31032, #82599, #16345, #23907, #46143, #32421, #61767, #10158, #17746, #39027, #75501, #4004, #83054, #3063, #31948, #47058, #11092, #10623, #39481, #45661, #54184, #61320, #31491, #39958, #68402, #74098, #45195, #23455, #9217, #38097, #2143, #59921, #88761, #52778, #74569, #67482, #60379, #27658, #76443, #91069, #90600, #56556, #55133, #27182, #77851, #6344, #85410, #70293, #20558, #26240, #25760, #91560, #49430, #42308, #83997, #71217, #84922, #92490, #76904, #83516, #12034, #48471, #19145, #5424, #78318, #13457, #70748, #48000, #41837, #5882, #26717, #34752, #35216, #54643, #77371, #12508, #18673, #40881, #92027, #4933, #20073, #48953, #40412, #47539, #13001, #69799, #33820, #62235, #11564, #62730, #63197, #34289, #63667, #55604, #84453, #69330, #4461, #19603, #33338, #41359, #56069, #28134, #14849, #37075, #29044, #8641, #64143, #65066, #28589, #65984, #29976, #85861, #57023, #36145, #36605, #21472, #165, #73064, #43702, #7723, #21012, #51269, #1095, #6821, #57936, #57479, #15300, #65523, #92976, #71692, #49879, #641, #51723, #78777, #43254, #35695, #72601, #64609, #8194, #29525, #80615, #58860, #86791, #58405, #22397, #13918, #21950, #44159, #50823, #79707, #87706, #79254, #87251, #80162, #22857, #86320, #15771, #44630, #42775, #73532, #93435, #50349, #14395, #72152, #7268, #67362, #16681, #88641, #31369, #52653, #10037, #66428, #46937, #82001, #45078, #38907, #1547, #37972, #38456, #46479, #75839, #9568, #74926, #53121, #31827, #18083, #3402, #2492, #17157, #32293, #61199, #60258, #46023, #2017, #10495, #75382, #45536, #68280, #67816, #88172, #30430, #2941, #89095, #90035, #60718, #89557, #59321, #24726, #25187, #23332, #74437, #54060, #52201, #66880, #37518, #82931, #53609, #82480, #17627, #30910, #39364, #59800, #24247, #81083, #9095, #81533, #16227, #73978, #23789, #70631, #91903, #92371, #69212, #40297, #55002, #27531, #62597, #76319, #34632, #63543, #48348, #83875, #19482, #32761, #68753, #61649, #49303, #90482, #3884, #10962, #27057, #26592, #40759, #55944, #19949, #25640, #84799, #20435, #84331, #47409, #56424, #33218, #54523, #12380, #48820, #83392, #39829, #18542, #77251, #77726, #41227, #70166, #5301, #4808, #85285, #11445, #4341, #34171, #62114, #11910, #90945, #19026, #55482, #76784, #69677, #12877, #63073, #26109, #41715, #47880, #33688, #91441, #5758, #64953, #51162, #64494, #28015, #36965, #36036, #72950, #93320, #14740, #79132, #50228, #42652, #80049, #50713, #13337, #58297, #21837, #14280, #7607, #29869, #71570, #43141, #57365, #35579, #72045, #28472, #6705, #43595, #65412, #87595, #8077, #57821, #65878, #78660, #78198, #7161, #987, #58753, #13801, #22741, #72491, #15189, #86207, #71091, #21358, #54, #28935, #86672, #44049, #42178, #87141, #79599, #29406, #22291, #36495, #6224, #35094, #64012, #522, #92851, #56906, #85746, #20893, #49765, #74818, #9933, #1438, #51615, #38807, #52095, #30796, #23215, #17524, #80979, #24138, #88991, #45912, #1906, #44973, #75274, #15651, #66775, #8535, #67711, #17046, #44521, #2387, #24611, #16576, #89930, #80503, #52551, #16122, #53498, #46374, #73425, #37414, #23687, #53016, #8992, #81427, #60614, #31265, #81894, #66324, #2841, #82374, #88058, #45432, #73874, #31723, #89452, #30323, #59212, #37870, #10393, #39258, #59695, #88538, #74332, #60152, #9456, #68173, #3294, #32185, #61090, #38342, #67255, #77146, #53960, #83764, #70052, #54885, #83290, #26955, #84699, #46832, #82827, #90839, #91326, #76211, #18920, #34067, #69571, #62486, #75734, #12276, #55845, #61549, #47774, #18436, #5194, #26488, #17980, #32662, #10858, #55378, #12769, #63440, #4236, #90383, #33577, #25538, #62969, #84230, #41611, #91803, #26000, #4700, #41120, #39721, #76675, #19846, #11801, #40652, #48717, #40193, #19379, #48244, #77620, #47294, #70533, #5657, #68645, #34532, #25086, #3778, #54419, #11340, #69111, #33116, #62004, #49663, #86104, #13696, #56802, #28833, #79499, #7965, #87036, #71939, #22187, #92744, #92270, #93217, #51055, #43941, #27915, #72838, #86563, #411, #78558, #85182, #42548, #50123, #85644, #7060, #29298, #58193, #72389, #20792, #43493, #7506, #28369, #36391, #79943, #36859, #79021, #14174, #27427, #71463, #93675, #6596, #21732, #50608, #42074, #56317, #14635, #35474, #64391, #63909, #15081, #57261, #64848, #35930, #65304, #21253, #43037, #20331, #49201, #57717, #78097, #13238, #70990, #6122, #34992, #38703, #30683, #10285, #65775, #66670, #15541, #24499, #38232, #884, #75172, #16471, #73321, #67145, #29765, #66218, #1798, #74709, #58644, #37765, #9347, #81324, #60048, #46268, #31618, #59583, #45326, #60509, #89344, #88434, #74228, #30215, #67610, #9830, #44870, #2738, #2279, #22636, #87486, #31162, #23583, #53381, #88886, #24034, #51508, #52910, #82266, #80396, #73772, #17419, #44413, #1333, #8432, #37311, #81788, #16937, #45799, #59106, #87948, #23100, #52450, #51982, #80871, #16019, #8886, #3192, #39611, #5075, #26382, #26846, #3673, #68535, #83187, #55734, #90734, #10754, #62861, #91694, #76574, #18334, #47673, #60975, #32076, #89824, #77504, #24985, #53858, #39155, #55270, #54775, #69007, #84125, #48133, #82724, #19275, #48604, #18816, #75631, #84586, #61452, #17876, #40548, #77036, #46728, #68067, #32560, #11697, #12167, #69463, #4595, #33468, #33009, #19736, #90283, #25434, #62371, #54312, #40091, #47190, #76103, #83652, #11236, #4138, #41010, #91214, #61900, #69933, #25893, #33957, #20683, #37093, #660, #80636, #92625, #41966, #56689, #30451, #65545, #77989, #37539, #66450, #51288, #85536, #22416, #34422, #70426, #63329, #52222, #92160, #5552, #12651, #1114, #29544, #42437, #29995, #22878, #27317, #58880, #23355, #87270, #49091, #59344, #34885, #56203, #15318, #87726, #85062, #41496, #20213, #80180, #51744, #44178, #73084, #8215, #6478, #88195, #13130, #70879, #66002, #6010, #13585, #63796, #49554, #58424, #78449, #71347, #15792, #44651, #27796, #73552, #36624, #8661, #1568, #10518, #67838, #54081, #67383, #30931, #39852, #53632, #16248, #90501, #31849, #88662, #82502, #45098, #81555, #82023, #90055, #25661, #53143, #24749, #2963, #75404, #61669, #46958, #17180, #60738, #75860, #10983, #46044, #89579, #45558, #82951, #25208, #60280, #18105, #17650, #37994, #74000, #46501, #74949, #68775, #39387, #68302, #9117, #3423, #3904, #66902, #89117, #32781, #2041, #16703, #81105, #59821, #32318, #61221, #23811, #74459, #52674, #9591, #10059, #38479, #2513, #31390, #24268, #38929, #55025, #20455, #41735, #42197, #19046, #55963, #18564, #83895, #55503, #63563, #64030, #26612, #91922, #70188, #48840, #35110, #49323, #84352, #5322, #78217, #13356, #19501, #34190, #47902, #27550, #92390, #33709, #85306, #63094, #11466, #47430, #27077, #48368, #71110, #84817, #12897, #76340, #19966, #6241, #40317, #62621, #92871, #69232, #76804, #54543, #83411, #77745, #70648, #5776, #11930, #56444, #40778, #77271, #4361, #26130, #4826, #34650, #33238, #69697, #62134, #90965, #91461, #12400, #41247, #72059, #44536, #79613, #93337, #51630, #80516, #65425, #7176, #36510, #49781, #85762, #78677, #66338, #13818, #20912, #28034, #15205, #43609, #57836, #44063, #36980 ),
 ( #28488, #56923, #28950, #15668, #73439, #57381, #8549, #22305, #29884, #14297, #42670, #43158, #14754, #86224, #7624, #58768, #87610, #8092, #21374, #72964, #65892, #86689, #1004, #22758, #71587, #72505, #37429, #21854, #6723, #35596, #50729, #50244, #64511, #79149, #36051, #64969, #71, #538, #29422, #58312, #87156, #51176, #80063, #88074, #31281, #81909, #16135, #23701, #73888, #60167, #9471, #1452, #44987, #23229, #38356, #9949, #30337, #59710, #9005, #67271, #37884, #17061, #2401, #67728, #45926, #52564, #89005, #24153, #59228, #74348, #74836, #45447, #53032, #52110, #81444, #38821, #80993, #66789, #1919, #30812, #88553, #16592, #66180, #29728, #22150, #15501, #37726, #50564, #51018, #65264, #43452, #79905, #7467, #79461, #22596, #73283, #1757, #80830, #65736, #15981, #86522, #86064, #86998, #44833, #66632, #21687, #30644, #80360, #87911, #72349, #78979, #36350, #43903, #14595, #847, #23062, #51940, #1297, #370, #37274, #30179, #15043, #59063, #73736, #21214, #72800, #7924, #50084, #29256, #87450, #58152, #44372, #8396, #35893, #14131, #8848, #36815, #58609, #57679, #42996, #51471, #71902, #7022, #64811, #93635, #28792, #83144, #23544, #74668, #16435, #82688, #24943, #60009, #88849, #68028, #45287, #60471, #59543, #38667, #75136, #31582, #89306, #39572, #3155, #23998, #32038, #2239, #76062, #67571, #17838, #46232, #32517, #45758, #9309, #18295, #60933, #88393, #68968, #10246, #67105, #89780, #52414, #52871, #24462, #68494, #4098, #53341, #53820, #39115, #46690, #40051, #25394, #82226, #75592, #54274, #47153, #17380, #10715, #81750, #61413, #3629, #2700, #90245, #11191, #74190, #81289, #38191, #31123, #16900, #9792, #85020, #54735, #12609, #63757, #90693, #40973, #92587, #18774, #33429, #32969, #27756, #92122, #20172, #56163, #26339, #34846, #62333, #33914, #83613, #4555, #76998, #27276, #25853, #91173, #56652, #49052, #20648, #55232, #84087, #12127, #49518, #84547, #19237, #85501, #78410, #70386, #69895, #41454, #47632, #76536, #11658, #71309, #40505, #69424, #61862, #77947, #48563, #62823, #13091, #41929, #48094, #70840, #42398, #5514, #5034, #13549, #91657, #26810, #34384, #5973, #55696, #19694, #77466, #63289, #87345, #7814, #79798, #65625, #260, #22955, #29622, #51829, #64697, #36239, #79352, #57568, #29143, #21567, #93523, #36704, #22494, #15875, #1192, #14940, #30073, #6909, #6439, #7357, #58958, #80722, #35784, #44731, #737, #8291, #86411, #93070, #50450, #58039, #28682, #43795, #37172, #66080, #80258, #14487, #51367, #15394, #65157, #44261, #87806, #35314, #86891, #22045, #64239, #43345, #58500, #72242, #73172, #28224, #49972, #57112, #85952, #50914, #72695, #71787, #21104, #78864, #14014, #42874, #67923, #23891, #66989, #3515, #37620, #88745, #30530, #3047, #39009, #66531, #24353, #46586, #38564, #18191, #73632, #74551, #38078, #75484, #39467, #1650, #59432, #45642, #46127, #31016, #9682, #82584, #53228, #17269, #88283, #60822, #10609, #16329, #67466, #2127, #24834, #75030, #8743, #81183, #23438, #10143, #61305, #52306, #52760, #45179, #82110, #74081, #17731, #31931, #90141, #68384, #2595, #89665, #53717, #9200, #31475, #32407, #60363, #89201, #25291, #81641, #54169, #83038, #59903, #16788, #48934, #19585, #75944, #27163, #84437, #76887, #12015, #26222, #4442, #40865, #62219, #11549, #77355, #34273, #56537, #41820, #26700, #70731, #47523, #47043, #47984, #5864, #92472, #76428, #27638, #41341, #77834, #33322, #39943, #91048, #4914, #40396, #55589, #12982, #34734, #56051, #69314, #92011, #84905, #69783, #20053, #63650, #85394, #33800, #62714, #11074, #55116, #48454, #83981, #70275, #5408, #90584, #68859, #63180, #19129, #91544, #18656, #3988, #12489, #32863, #61752, #25745, #54626, #83498, #44139, #78302, #35679, #71200, #43686, #79690, #13441, #65045, #87231, #79236, #58845, #20542, #21456, #78760, #22379, #80142, #42288, #6327, #86304, #86772, #71672, #50329, #29506, #148, #57915, #35195, #7704, #51252, #57006, #14378, #13901, #65502, #21933, #49412, #28118, #64123, #50805, #8174, #92959, #93419, #85843, #29028, #20995, #58388, #14832, #37058, #15282, #43238, #72582, #36588, #49861, #72136, #621, #7252, #36128, #73044, #64594, #65968, #1079, #29959, #42755, #6806, #28571, #57461, #67801, #31354, #23773, #17140, #39347, #52186, #66864, #9551, #59785, #88626, #2926, #2477, #88154, #60242, #30415, #10481, #1999, #46006, #74422, #60704, #73963, #37503, #46464, #89080, #22841, #3388, #38438, #1529, #24229, #51708, #23313, #52638, #31811, #32276, #81518, #53106, #67347, #81984, #68266, #53593, #16665, #74911, #82466, #17613, #45520, #10022, #81067, #89544, #24707, #30892, #75367, #38892, #44613, #80596, #87688, #15753, #73517, #8626, #66412, #59306, #16212, #45063, #9077, #37957, #91890, #46924, #61637, #61182, #27044, #26580, #48336, #84318, #54509, #63061, #90470, #62099, #82917, #32749, #11432, #55469, #25173, #25627, #55932, #77237, #48807, #83381, #18529, #40283, #77714, #19015, #47395, #84787, #19937, #4796, #69200, #69664, #18071, #54047, #75826, #5747, #10950, #39816, #90020, #12367, #76770, #90932, #41215, #70152, #68739, #5288, #70620, #40747, #3870, #12864, #76306, #4329, #62584, #34158, #33206, #26097, #54986, #33675, #41703, #91426, #19469, #83862, #47867, #11898, #35083, #64002, #43129, #20423, #35569, #34622, #36482, #20881, #78187, #87129, #7149, #63532, #44035, #79122, #42167, #36024, #92359, #92840, #64483, #43582, #72937, #6694, #72034, #50218, #28922, #15177, #512, #93310, #14269, #29394, #58286, #28460, #64941, #28003, #65399, #72480, #13790, #22280, #42, #49292, #27521, #57810, #57354, #51152, #86661, #21825, #56414, #50700, #80036, #13325, #42642, #71082, #6214, #56896, #85735, #49753, #79588, #14729, #78650, #71559, #86195, #21347, #8980, #29856, #73413, #52083, #68510, #65867, #8523, #68984, #90261, #90708, #66312, #37402, #80966, #25869, #59683, #1427, #32986, #61877, #45420, #16111, #16565, #58740, #975, #87583, #47649, #22728, #51602, #8063, #25410, #23674, #37859, #54289, #18312, #80490, #83160, #18790, #81415, #44507, #54751, #30311, #15638, #10731, #47168, #59200, #88047, #23203, #74320, #76077, #39587, #3645, #32536, #1894, #83628, #44962, #73862, #61429, #66763, #30785, #88526, #52540, #11208, #40066, #4114, #56666, #85037, #77015, #49067, #19253, #93084, #84563, #5988, #63306, #42413, #12624, #27292, #71324, #6454, #77481, #56179, #69910, #49532, #85515, #55712, #13563, #20187, #33445, #40523, #77964, #70402, #35329, #92137, #34860, #4571, #13107, #64255, #69441, #19710, #28239, #62348, #12143, #76551, #57126, #41944, #63773, #92602, #5049, #78425, #33931, #41470, #91189, #48111, #26825, #70856, #26356, #62839, #85968, #27772, #21118, #91672, #48581, #5529, #11674, #34399, #20661, #55247, #84104, #72090, #13852, #43190, #56484, #92425, #85342, #72997, #49359, #27587, #34687, #21888, #50278, #64544, #50760, #43639, #78253, #79644, #44092, #14330, #71147, #80095, #56957, #13391, #36082, #14786, #42234, #63601, #6276, #7207, #72537, #65001, #103, #28982, #28520, #51206, #35145, #64068, #57868, #92908, #35629, #28068, #42705, #79186, #6756, #93370, #7656, #86724, #85794, #36541, #20945, #15236, #71623 ) ),
 .UNSPECIFIED., .F., .F., .F.,
 ( 4, 3, 3, 3, 3, 3, 3, 3, 3, 3, 3, 3, 4 ),
 ( 4, 3, 3, 3, 3, 3, 3, 3, 3, 3, 3, 3, 3, 3, 3, 3, 3, 3, 3, 3, 3, 3, 3, 3, 3, 3, 3, 3, 3, 3, 3, 3, 3, 3, 3, 3, 3, 3, 3, 3, 3, 3, 3, 3, 3, 3, 3, 3, 3, 3, 3, 3, 3, 3, 3, 3, 3, 3, 3, 3, 3, 3, 3, 3, 3, 3, 3, 3, 3, 3, 3, 3, 3, 3, 3, 3, 3, 3, 3, 3, 3, 3, 3, 3, 3, 3, 3, 3, 3, 3, 3, 3, 3, 3, 3, 3, 3, 3, 3, 3, 3, 3, 3, 3, 3, 3, 3, 3, 3, 3, 3, 3, 3, 3, 3, 3, 3, 3, 3, 3, 3, 3, 3, 3, 3, 3, 3, 3, 3, 3, 3, 3, 3, 3, 3, 3, 3, 3, 3, 3, 3, 3, 3, 3, 3, 3, 3, 3, 3, 3, 3, 3, 3, 3, 3, 3, 3, 3, 3, 3, 3, 3, 3, 3, 3, 3, 3, 3, 3, 3, 3, 3, 3, 3, 3, 3, 3, 3, 3, 3, 3, 3, 3, 3, 3, 3, 3, 3, 3, 3, 3, 3, 3, 3, 3, 3, 3, 3, 3, 3, 3, 3, 3, 3, 3, 3, 3, 3, 3, 3, 3, 3, 3, 3, 3, 3, 3, 3, 3, 3, 3, 3, 3, 3, 3, 3, 3, 3, 3, 3, 3, 3, 3, 3, 3, 3, 3, 3, 3, 3, 3, 3, 3, 3, 3, 3, 3, 3, 3, 3, 3, 3, 3, 3, 3, 3, 3, 3, 3, 3, 3, 3, 3, 3, 3, 3, 3, 3, 3, 3, 3, 3, 3, 3, 3, 3, 3, 3, 3, 3, 3, 3, 3, 3, 3, 3, 3, 3, 3, 3, 3, 3, 3, 3, 3, 3, 3, 3, 3, 4 ),
 ( 0.4999999999939828133, 0.5624999999954868324, 0.6249999999969908515, 0.6562499999977429166, 0.6874999999984949817, 0.7187499999992470467, 0.7499999999999990008, 0.7812500000007509549, 0.8125000000015030199, 0.8437500000022550850, 0.8750000000030071501, 0.9375000000045111692, 1.000000000006015188 ),
 ( -0.05833358852679956102, -0.001562739243874584211, -0.0006756947238288813938, 0.0002113497962168214232, 0.001985438836308227057, 0.005533616916491038325, 0.009081794996673850026, 0.01262997307685666086, 0.01440406211694806801, 0.01617815115703947343, 0.01972632923722228426, 0.02327450731740509510, 0.02682268539758790593, 0.02859677443767931135, 0.03037086347777071677, 0.03391904155795352760, 0.03746721963813633843, 0.04101539771831914927, 0.04278948675841055815, 0.04456357579850196010, 0.04811175387868477094, 0.05165993195886758177, 0.05520811003905039260, 0.05698219907914180149, 0.05875628811923321038, 0.06230446619941602121, 0.06585264427959883204, 0.06940082235978164982, 0.07117491139987305870, 0.07294900043996446759, 0.07649717852014727149, 0.08004535660033007538, 0.08359353468051289315, 0.08536762372060430204, 0.08714171276069571093, 0.09068989084087851482, 0.09423806892106131872, 0.09778624700124413649, 0.09956033604133554538, 0.1013344250814269543, 0.1048826031616097582, 0.1084307812417925621, 0.1119789593219753798, 0.1137530483620667887, 0.1155271374021581976, 0.1190753154823410015, 0.1226234935625238054, 0.1261716716427066232, 0.1279457606827980043, 0.1297198497228894132, 0.1332680278030722310, 0.1368162058832550487, 0.1403643839634378665, 0.1421384730035292754, 0.1439125620436206843, 0.1474607401238035020, 0.1510089182039863198, 0.1545570962841691098, 0.1563311853242604910, 0.1581052743643518999, 0.1616534524445347176, 0.1652016305247175354, 0.1687498086049003532, 0.1705238976449917621, 0.1722979866850831709, 0.1758461647652659887, 0.1793943428454488065, 0.1829425209256315965, 0.1847166099657229776, 0.1864906990058143865, 0.1900388770859972043, 0.1935870551661800221, 0.1971352332463628398, 0.1989093222864542487, 0.2006834113265456576, 0.2042315894067284754, 0.2077797674869112932, 0.2113279455670940832, 0.2131020346071854643, 0.2148761236472768732, 0.2184243017274596910, 0.2219724798076425087, 0.2255206578878253265, 0.2272947469279167354, 0.2290688359680081443, 0.2326170140481909621, 0.2361651921283737798, 0.2397133702085565699, 0.2414874592486479510, 0.2432615482887393599, 0.2468097263689221776, 0.2503579044491049954, 0.2539060825292878132, 0.2556801715693792221, 0.2574542606094706310, 0.2610024386896534487, 0.2645506167698362665, 0.2680987948500190843, 0.2698728838901104932, 0.2716469729302019021, 0.2751951510103847198, 0.2787433290905675376, 0.2822915071707502999, 0.2840655962108417087, 0.2858396852509330621, 0.2893878633311158799, 0.2929360414112986977, 0.2964842194914815154, 0.3000323975716643332, 0.3035805756518471510, 0.3071287537320299688, 0.3106769318122127865, 0.3142251098923956043, 0.3177732879725784221, 0.3213214660527612399, 0.3248696441329440576, 0.3284178222131268754, 0.3301919112532182843, 0.3319660002933096932, 0.3355141783734925109, 0.3390623564536752732, 0.3426105345338580355, 0.3443846235739494444, 0.3461587126140408532, 0.3497068906942236710, 0.3532550687744064888, 0.3568032468545893066, 0.3585773358946807154, 0.3603514249347721243, 0.3638996030149549421, 0.3674477810951377599, 0.3709959591753205776, 0.3727700482154119865, 0.3745441372555033954, 0.3780923153356862132, 0.3816404934158690310, 0.3851886714960518487, 0.3869627605361432576, 0.3887368495762346665, 0.3922850276564174843, 0.3958332057366002465, 0.3993813838167830088, 0.4011554728568744177, 0.4029295618969658266, 0.4064777399771486444, 0.4100259180573314621, 0.4135740961375142799, 0.4153481851776056888, 0.4171222742176970977, 0.4206704522978799154, 0.4242186303780627332, 0.4277668084582455510, 0.4295408974983369599, 0.4313149865384283688, 0.4348631646186111865, 0.4384113426987940043, 0.4419595207789768221, 0.4437336098190682310, 0.4455076988591596399, 0.4490558769393424576, 0.4526040550195252754, 0.4561522330997080932, 0.4579263221397995021, 0.4597004111798909110, 0.4632485892600737287, 0.4667967673402565465, 0.4703449454204393643, 0.4721190344605307732, 0.4738931235006221820, 0.4774413015808049998, 0.4809894796609877621, 0.4845376577411705243, 0.4863117467812619332, 0.4880858358213533421, 0.4916340139015361599, 0.4951821919817189777, 0.4987303700619017954, 0.5005044591019931488, 0.5022785481420846132, 0.5058267262222674310, 0.5093749043024502487, 0.5129230823826330665, 0.5146971714227244199, 0.5164712604628158843, 0.5200194385429987021, 0.5235676166231815198, 0.5271157947033643376, 0.5288898837434556910, 0.5306639727835471554, 0.5342121508637299732, 0.5377603289439127909, 0.5413085070240956087, 0.5430825960641869621, 0.5448566851042784265, 0.5484048631844612443, 0.5519530412646440620, 0.5555012193448268798, 0.5572753083849182332, 0.5590493974250096976, 0.5625975755051924043, 0.5661457535853752221, 0.5696939316655580399, 0.5714680207056493932, 0.5732421097457407466, 0.5767902878259235644, 0.5803384659061063822, 0.5838866439862891999, 0.5856607330263805533, 0.5874348220664720177, 0.5909830001466548355, 0.5945311782268376533, 0.5980793563070204710, 0.5998534453471118244, 0.6016275343872032888, 0.6051757124673861066, 0.6087238905475689243, 0.6122720686277517421, 0.6140461576678430955, 0.6158202467079345599, 0.6193684247881173777, 0.6229166028683001954, 0.6264647809484830132, 0.6282388699885743666, 0.6300129590286658310, 0.6335611371088486488, 0.6371093151890314665, 0.6406574932692142843, 0.6424315823093056377, 0.6442056713493971021, 0.6477538494295799198, 0.6513020275097627376, 0.6548502055899455554, 0.6566242946300369088, 0.6583983836701283732, 0.6619465617503111909, 0.6654947398304940087, 0.6690429179106768265, 0.6708170069507681799, 0.6725910959908596443, 0.6761392740710423510, 0.6796874521512251688, 0.6832356302314079866, 0.6850097192714993399, 0.6867838083115906933, 0.6903319863917735111, 0.6938801644719563289, 0.6974283425521391466, 0.6992024315922305000, 0.7009765206323219644, 0.7045246987125047822, 0.7080728767926875999, 0.7116210548728704177, 0.7133951439129617711, 0.7151692329530532355, 0.7187174110332360533, 0.7222655891134188710, 0.7258137671936016888, 0.7275878562336930422, 0.7293619452737845066, 0.7329101233539673244, 0.7364583014341501421, 0.7400064795143329599, 0.7417805685544243133, 0.7435546575945157777, 0.7471028356746985954, 0.7506510137548814132, 0.7541991918350642310, 0.7559732808751555844, 0.7577473699152470488, 0.7612955479954298665, 0.7648437260756126843, 0.7683919041557955021, 0.7701659931958868555, 0.7719400822359783199, 0.7754882603161611376, 0.7790364383963439554, 0.7825846164765267732, 0.7843587055166181266, 0.7861327945567095909, 0.7896809726368922977, 0.7932291507170751155, 0.7967773287972579332, 0.7985514178373492866, 0.8003255068774406400, 0.8038736849576234578, 0.8074218630378062755, 0.8109700411179890933, 0.8127441301580804467, 0.8145182191981719111, 0.8180663972783547289, 0.8216145753585375466, 0.8251627534387203644, 0.8269368424788117178, 0.8287109315189031822, 0.8322591095990860000, 0.8358072876792688177, 0.8393554657594516355, 0.8429036438396344533, 0.8464518219198172710, 0.8500000000000000888 ),
 .UNSPECIFIED. ) ;
#68541 = CARTESIAN_POINT ( 'NONE',  ( -100.2162370998004661, -296.5324065943632945, -307.6733667738163831 ) ) ;
#68542 = ORIENTED_EDGE ( 'NONE', *, *, #18738, .F. ) ;
#68543 = CARTESIAN_POINT ( 'NONE',  ( 34.80532095757826738, -292.4204426637509755, -284.3629331368638304 ) ) ;
#68544 = CARTESIAN_POINT ( 'NONE',  ( 10.46917891676551093, -277.0633869961445157, -330.6572904885218804 ) ) ;
#68545 = CARTESIAN_POINT ( 'NONE',  ( -0.5462705402492801232, -274.5558203383570230, -207.2981618509985253 ) ) ;
#68546 = CARTESIAN_POINT ( 'NONE',  ( 37.33707448775041371, -274.2526925033810130, -252.8519235993141194 ) ) ;
#68547 = DIRECTION ( 'NONE',  ( 0.000000000000000000, 0.000000000000000000, -1.000000000000000000 ) ) ;
#68548 = CARTESIAN_POINT ( 'NONE',  ( -68.46841309576564072, -271.6430645188398785, -202.1114116155810052 ) ) ;
#68549 = CIRCLE ( 'NONE', #3519, 0.5000000000000004441 ) ;
#68550 = CARTESIAN_POINT ( 'NONE',  ( -65.37033610184988675, -296.8367015690104722, -341.4596994596136028 ) ) ;
#68551 = B_SPLINE_CURVE_WITH_KNOTS ( 'NONE', 3,
 ( #49592, #21179, #93144, #6986, #58119, #43419, #42477, #50529, #57642, #92201, #28299, #7435, #86487, #56245 ),
 .UNSPECIFIED., .F., .F.,
 ( 4, 2, 2, 2, 2, 2, 4 ),
 ( 0.000000000000000000, 0.0003894434397089267179, 0.0007788868794178534357, 0.001168330319126780316, 0.001557773758835706871, 0.002336660638253565837, 0.003115547517671425019 ),
 .UNSPECIFIED. ) ;
#68552 = CARTESIAN_POINT ( 'NONE',  ( 200.9306832106270804, -125.2391364535880882, 0.000000000000000000 ) ) ;
#68553 = CIRCLE ( 'NONE', #67000, 1.000000000000000888 ) ;
#68554 = CARTESIAN_POINT ( 'NONE',  ( -110.6996360347542776, -285.6244184340591801, -270.9253420812303261 ) ) ;
#68555 = CARTESIAN_POINT ( 'NONE',  ( 36.21657354682313468, -283.5539769589865955, -289.4177281235543546 ) ) ;
#68556 = CARTESIAN_POINT ( 'NONE',  ( -103.5743098842943226, -284.3193555158867980, -239.3035658067771010 ) ) ;
#68557 = CARTESIAN_POINT ( 'NONE',  ( 17.10777756799823379, -274.6591231268566276, -320.1965719770602732 ) ) ;
#68558 = CARTESIAN_POINT ( 'NONE',  ( 12.76761964058083088, -284.2044992727001045, -325.1326575853840382 ) ) ;
#68559 = CARTESIAN_POINT ( 'NONE',  ( -51.43223250054848705, -275.7154883937388377, -342.6948213860720216 ) ) ;
#68560 = EDGE_CURVE ( 'NONE', #3498, #15284, #88311, .T. ) ;
#68561 = CARTESIAN_POINT ( 'NONE',  ( 35.91155138593595808, -276.6837768033442444, -274.3156557491608964 ) ) ;
#68562 = ADVANCED_FACE ( 'NONE', ( #23393 ), #15741, .T. ) ;
#68563 = CARTESIAN_POINT ( 'NONE',  ( 194.6714370800177676, 41.21621202809333084, 14.07240042052004725 ) ) ;
#68564 = CARTESIAN_POINT ( 'NONE',  ( -114.0502448525816277, -279.4109720149994587, -265.8936817706091347 ) ) ;
#68565 = EDGE_LOOP ( 'NONE', ( #53360, #72419, #75288, #18680, #38135, #37340 ) ) ;
#68566 = CARTESIAN_POINT ( 'NONE',  ( 197.3380612925966489, 18.22700036951276914, 11.15593255764728831 ) ) ;
#68567 = CARTESIAN_POINT ( 'NONE',  ( -109.5017692797823514, -286.1170155089739069, -293.4956305377884291 ) ) ;
#68568 = CARTESIAN_POINT ( 'NONE',  ( -97.32160743803765968, -295.1664816039354378, -312.2539866627246852 ) ) ;
#68569 = CARTESIAN_POINT ( 'NONE',  ( -75.62014853386071422, -288.8976352219044088, -337.0549945700602734 ) ) ;
#68571 = CARTESIAN_POINT ( 'NONE',  ( -68.20357379545868071, -289.8810540651671772, -203.0752192651493999 ) ) ;
#68570 = CARTESIAN_POINT ( 'NONE',  ( 2.783371771579112863, -285.1769438582871317, -208.6735704435149614 ) ) ;
#68572 = CARTESIAN_POINT ( 'NONE',  ( -69.16753041430311555, -284.6854772919191987, -336.5130849264336348 ) ) ;
#68573 = CARTESIAN_POINT ( 'NONE',  ( 21.06697382105475214, -274.1995948486199381, -317.4284998610248749 ) ) ;
#68574 = CARTESIAN_POINT ( 'NONE',  ( 7.447648527805312391, -286.8528826659853053, -332.0731907457429770 ) ) ;
#68575 = CARTESIAN_POINT ( 'NONE',  ( -46.29274066174475166, -287.9387348557513633, -195.8971701904704332 ) ) ;
#68576 = CARTESIAN_POINT ( 'NONE',  ( 25.61645148577000342, -284.9993870828843683, -229.2965399195133216 ) ) ;
#68577 = AXIS2_PLACEMENT_3D ( 'NONE', #42941, #14076, #58559 ) ;
#68578 = CARTESIAN_POINT ( 'NONE',  ( -5.921152389044468833, -283.5699898319567751, -336.5274465075643207 ) ) ;
#68579 = CARTESIAN_POINT ( 'NONE',  ( 6.877081978565874998, -290.4525920709832008, -331.2095906079471774 ) ) ;
#68580 = DIRECTION ( 'NONE',  ( 0.000000000000000000, 0.000000000000000000, 1.000000000000000000 ) ) ;
#68581 = DIRECTION ( 'NONE',  ( -1.000000000000000000, 0.000000000000000000, 0.000000000000000000 ) ) ;
#68582 = CARTESIAN_POINT ( 'NONE',  ( -89.69635647249970134, -297.7033392421006397, -324.9152747110364885 ) ) ;
#68583 = CARTESIAN_POINT ( 'NONE',  ( -66.83331135974327708, -277.6655957160806452, -201.3888194779807748 ) ) ;
#68584 = CARTESIAN_POINT ( 'NONE',  ( -2.120726005228241284, -291.7035516898681067, -202.0555087003184838 ) ) ;
#68585 = CARTESIAN_POINT ( 'NONE',  ( -109.9326886625786841, -294.7775098989829416, -283.7349414300272201 ) ) ;
#68586 = CARTESIAN_POINT ( 'NONE',  ( 28.58610029905434047, -280.6754999593893558, -302.9537583182598723 ) ) ;
#68587 = CARTESIAN_POINT ( 'NONE',  ( -36.69956105920720546, -272.1401272554613797, -195.9112232137441936 ) ) ;
#68588 = CARTESIAN_POINT ( 'NONE',  ( -5.311542420477732840, -295.9367735326890738, -336.5211685940752204 ) ) ;
#68589 = CARTESIAN_POINT ( 'NONE',  ( -37.37352853689063892, -300.5519495502701943, -195.3611179825600175 ) ) ;
#68590 = CARTESIAN_POINT ( 'NONE',  ( -51.65143983541086214, -296.3523193208734483, -195.3543580251313188 ) ) ;
#68591 = CARTESIAN_POINT ( 'NONE',  ( 10.54214184089140538, -292.6414439185925289, -329.4298554152745169 ) ) ;
#68592 = AXIS2_PLACEMENT_3D ( 'NONE', #51439, #80327, #67068 ) ;
#68593 = CARTESIAN_POINT ( 'NONE',  ( -28.04979484130534217, -293.5975427623568521, -197.3097182586588190 ) ) ;
#68594 = DIRECTION ( 'NONE',  ( 0.6056179655966479336, -0.7957555401921982963, 0.000000000000000000 ) ) ;
#68595 = CARTESIAN_POINT ( 'NONE',  ( 35.78239982941985176, -294.3242115016623188, -268.0227998142505612 ) ) ;
#68596 = DIRECTION ( 'NONE',  ( -0.000000000000000000, -0.000000000000000000, -1.000000000000000000 ) ) ;
#68598 = CARTESIAN_POINT ( 'NONE',  ( -36.99554865599080955, -295.0476662810420407, -343.3727214492190569 ) ) ;
#68597 = CARTESIAN_POINT ( 'NONE',  ( -102.9966077819564845, -282.0806788966253862, -307.4511841741179410 ) ) ;
#68599 = CARTESIAN_POINT ( 'NONE',  ( 24.25510323288072456, -282.1671030528345909, -316.5653798607781937 ) ) ;
#68600 = CARTESIAN_POINT ( 'NONE',  ( -98.03037258737450088, -283.5859558642252978, -317.7175254347922078 ) ) ;
#68601 = CARTESIAN_POINT ( 'NONE',  ( -73.49076889010724756, -289.5716214850342567, -204.7798224669997751 ) ) ;
#68602 = DIRECTION ( 'NONE',  ( -0.000000000000000000, -0.000000000000000000, -1.000000000000000000 ) ) ;
#68603 = CARTESIAN_POINT ( 'NONE',  ( -0.7253004819445844076, -281.0547819986877016, -337.3232660508965068 ) ) ;
#68604 = AXIS2_PLACEMENT_3D ( 'NONE', #11633, #53792, #32944 ) ;
#68605 = CARTESIAN_POINT ( 'NONE',  ( -37.51474938202356668, -287.9745691729268628, -347.0648312298804967 ) ) ;
#68606 = FACE_OUTER_BOUND ( 'NONE', #92870, .T. ) ;
#68607 = CARTESIAN_POINT ( 'NONE',  ( -15.33505475997019474, -296.3627373208905738, -340.8573922075017890 ) ) ;
#68608 = CARTESIAN_POINT ( 'NONE',  ( 19.45150595521237946, -277.6767957354051077, -321.4995663681362998 ) ) ;
#68609 = CARTESIAN_POINT ( 'NONE',  ( -109.1521241605427264, -278.3935030675257281, -257.1191208857741231 ) ) ;
#68610 = CARTESIAN_POINT ( 'NONE',  ( -16.62865441239325293, -292.4792808192214579, -196.1993371135274344 ) ) ;
#68611 = AXIS2_PLACEMENT_3D ( 'NONE', #50772, #43654, #65936 ) ;
#68612 = CARTESIAN_POINT ( 'NONE',  ( -106.9110606339439045, -282.2480116897767175, -299.9809707674999686 ) ) ;
#68613 = VECTOR ( 'NONE', #53372, 1000.000000000000000 ) ;
#68614 = CARTESIAN_POINT ( 'NONE',  ( -93.69086985602459094, -279.8646018496164629, -319.8562866529097732 ) ) ;
#68615 = CARTESIAN_POINT ( 'NONE',  ( 33.87939142761410238, -292.3859421483160759, -253.2498223541569473 ) ) ;
#68616 = CARTESIAN_POINT ( 'NONE',  ( -74.75941460635843328, -295.5543429864280824, -205.3021768647415399 ) ) ;
#68617 = EDGE_LOOP ( 'NONE', ( #86827, #66401, #26961, #50807, #41203 ) ) ;
#68618 = DIRECTION ( 'NONE',  ( 1.000000000000000000, 0.000000000000000000, 0.000000000000000000 ) ) ;
#68619 = AXIS2_PLACEMENT_3D ( 'NONE', #41189, #32726, #68241 ) ;
#68620 = CARTESIAN_POINT ( 'NONE',  ( 35.59654044235114156, -292.9933352629919341, -265.3183356207289307 ) ) ;
#68621 = CARTESIAN_POINT ( 'NONE',  ( 216.5288609127277084, 293.9636489450776935, -40.00000000000000711 ) ) ;
#68622 = CARTESIAN_POINT ( 'NONE',  ( -82.13390479932374433, -293.1952119285919025, -326.4764044574609443 ) ) ;
#68623 = CARTESIAN_POINT ( 'NONE',  ( -34.04743167588155472, -297.1512035042145499, -193.5969219078835977 ) ) ;
#68624 = CARTESIAN_POINT ( 'NONE',  ( -26.70633511247313052, -287.4997668309037522, -194.5439389313508514 ) ) ;
#68625 = CARTESIAN_POINT ( 'NONE',  ( 28.22683077944572005, -287.8201497505969542, -302.4511126711154247 ) ) ;
#68626 = CARTESIAN_POINT ( 'NONE',  ( -109.1576076481700284, -279.8555616938490971, -286.9452331251816304 ) ) ;
#68627 = CARTESIAN_POINT ( 'NONE',  ( -68.49419641248647395, -299.3972907315938983, -203.2093744295884221 ) ) ;
#68628 = CIRCLE ( 'NONE', #51987, 239.0731808058633590 ) ;
#68629 = CARTESIAN_POINT ( 'NONE',  ( -56.71970302032536182, -276.1023893226414430, -341.2067259695984376 ) ) ;
#68630 = ORIENTED_EDGE ( 'NONE', *, *, #39673, .T. ) ;
#68631 = CARTESIAN_POINT ( 'NONE',  ( -113.5439911062901359, -272.5282768512489042, -258.9426176334921479 ) ) ;
#68632 = CARTESIAN_POINT ( 'NONE',  ( -89.65602300256830404, -291.7171379959017941, -323.3188919055007204 ) ) ;
#68633 = CARTESIAN_POINT ( 'NONE',  ( 28.88952403982315076, -295.6479434352949625, -308.1488594110221015 ) ) ;
#68634 = DIRECTION ( 'NONE',  ( 0.000000000000000000, 0.000000000000000000, 1.000000000000000000 ) ) ;
#68635 = CARTESIAN_POINT ( 'NONE',  ( -107.1013708393497268, -291.4932646068735949, -248.4675950932366959 ) ) ;
#68636 = CARTESIAN_POINT ( 'NONE',  ( -43.18343439339132317, -253.0206516614774728, -430.6442049081568939 ) ) ;
#68637 = ORIENTED_EDGE ( 'NONE', *, *, #37224, .F. ) ;
#68638 = CARTESIAN_POINT ( 'NONE',  ( 25.48217255793715807, -291.1236033665029481, -227.9194496951986650 ) ) ;
#68639 = CARTESIAN_POINT ( 'NONE',  ( -95.55789471610023611, -297.5666407242449623, -219.9166988193663315 ) ) ;
#68640 = CARTESIAN_POINT ( 'NONE',  ( -86.11125958076856080, -297.0200338997015592, -216.0139234138655695 ) ) ;
#68641 = DIRECTION ( 'NONE',  ( 1.000000000000000000, 0.000000000000000000, 0.000000000000000000 ) ) ;
#68642 = DIRECTION ( 'NONE',  ( 0.000000000000000000, 0.000000000000000000, 1.000000000000000000 ) ) ;
#68643 = CARTESIAN_POINT ( 'NONE',  ( -111.6465910024872983, -292.2914005872708572, -252.9976232931603306 ) ) ;
#68644 = CARTESIAN_POINT ( 'NONE',  ( -2.659677404128715672, -294.9805209788416391, -198.2697987213421698 ) ) ;
#68645 = CARTESIAN_POINT ( 'NONE',  ( -110.5072938928216502, -286.3493563833146140, -286.1325278324435999 ) ) ;
#68646 = CARTESIAN_POINT ( 'NONE',  ( -0.8058290590329729719, -272.5383256362744646, -205.0382613768491069 ) ) ;
#68647 = CARTESIAN_POINT ( 'NONE',  ( -16.25573009212761022, -276.2468732228163617, -198.9162276371535540 ) ) ;
#68648 = CARTESIAN_POINT ( 'NONE',  ( 7.564001427921393628, -290.7501676547364582, -210.9911578786071686 ) ) ;
#68649 = CARTESIAN_POINT ( 'NONE',  ( -112.8157320181750407, -280.5041551860678624, -263.1553515476312555 ) ) ;
#68650 = CARTESIAN_POINT ( 'NONE',  ( -24.05509554437135478, -282.2265260481609630, -342.2454612465816126 ) ) ;
#68651 = CARTESIAN_POINT ( 'NONE',  ( -73.93719678362836589, -278.6061805930011133, -337.7723650155444943 ) ) ;
#68652 = CARTESIAN_POINT ( 'NONE',  ( 39.24431913614497347, -280.3059525514516395, -267.0897205644089922 ) ) ;
#68653 = CARTESIAN_POINT ( 'NONE',  ( 195.1625751280944883, 283.5718810751147885, -110.6458996475216310 ) ) ;
#68654 = CARTESIAN_POINT ( 'NONE',  ( 33.49179082183145084, -276.1144101630742966, -240.6360990762123038 ) ) ;
#68655 = APPLICATION_PROTOCOL_DEFINITION ( 'draft international standard', 'automotive_design', 1998, #78364 ) ;
#68656 = CARTESIAN_POINT ( 'NONE',  ( -21.51763337645937924, -275.7716244540266644, -195.7132334690824678 ) ) ;
#68657 = CARTESIAN_POINT ( 'NONE',  ( 31.98288692825981272, -296.4805209788415823, -303.7098442033569654 ) ) ;
#68658 = ORIENTED_EDGE ( 'NONE', *, *, #15525, .F. ) ;
#68659 = ORIENTED_EDGE ( 'NONE', *, *, #92271, .T. ) ;
#68660 = VECTOR ( 'NONE', #10561, 1000.000000000000000 ) ;
#68661 = CARTESIAN_POINT ( 'NONE',  ( 169.8384340989974817, 275.5000000000000568, -24.41176470588234437 ) ) ;
#68662 = CARTESIAN_POINT ( 'NONE',  ( -66.43912295571479376, -290.5219125493131855, -337.7025482309915674 ) ) ;
#68663 = CARTESIAN_POINT ( 'NONE',  ( 35.42161599284018081, -289.5912973851545189, -292.3032460647767721 ) ) ;
#68664 = CARTESIAN_POINT ( 'NONE',  ( -82.61588540025805116, -289.0384784787281092, -327.7557241382404527 ) ) ;
#68665 = CARTESIAN_POINT ( 'NONE',  ( 28.64899394918147024, -286.5423695688986641, -230.7013677973067729 ) ) ;
#68666 = CARTESIAN_POINT ( 'NONE',  ( 151.0524635986548674, 20.99320456764979070, -6.527652849435627402 ) ) ;
#68667 = CARTESIAN_POINT ( 'NONE',  ( 35.82869930591363072, -279.8215298216422298, -260.3609744337043139 ) ) ;
#68668 = CARTESIAN_POINT ( 'NONE',  ( 34.57946447596738437, -289.1732613046047504, -251.9193465711355202 ) ) ;
#68669 = CARTESIAN_POINT ( 'NONE',  ( -53.86376685795306685, -281.7478142474320180, -342.2310316382112205 ) ) ;
#68670 = EDGE_CURVE ( 'NONE', #22603, #39182, #30033, .T. ) ;
#68671 = CARTESIAN_POINT ( 'NONE',  ( -92.59015885009021929, -280.5545822504652733, -221.8770194202433572 ) ) ;
#68672 = CARTESIAN_POINT ( 'NONE',  ( 36.46166604554806412, -288.2257441307552881, -249.0565273307610994 ) ) ;
#68673 = AXIS2_PLACEMENT_3D ( 'NONE', #89403, #2340, #37821 ) ;
#68674 = CARTESIAN_POINT ( 'NONE',  ( -96.93225853203573195, -278.4544643727180073, -312.6552196315389551 ) ) ;
#68675 = CARTESIAN_POINT ( 'NONE',  ( -99.69885131347328411, -289.9394640906909899, -225.8684847145223955 ) ) ;
#68676 = CARTESIAN_POINT ( 'NONE',  ( -68.44478495440118593, -286.4566494713619136, -200.0847118230900890 ) ) ;
#68677 = CARTESIAN_POINT ( 'NONE',  ( 5.140469346994207100, -287.1019880072113324, -206.1510190833839147 ) ) ;
#68678 = CARTESIAN_POINT ( 'NONE',  ( -34.84441460484721631, -283.1866265158773217, -343.3308267492291179 ) ) ;
#68679 = VERTEX_POINT ( 'NONE', #7776 ) ;
#68680 = CARTESIAN_POINT ( 'NONE',  ( 201.2509219215139922, 65.09645894978945080, 2.617322427804800622 ) ) ;
#68681 = CARTESIAN_POINT ( 'NONE',  ( -113.1538831664231850, -292.4014177154692220, -271.2384846505107703 ) ) ;
#68682 = VECTOR ( 'NONE', #66730, 1000.000000000000114 ) ;
#68683 = CARTESIAN_POINT ( 'NONE',  ( 27.64239246561254149, -291.7042667578300552, -229.8831898257906232 ) ) ;
#68684 = CIRCLE ( 'NONE', #38444, 0.4999999999999926170 ) ;
#68685 = CARTESIAN_POINT ( 'NONE',  ( -34.01804562442430324, -273.1537256354559986, -197.2012808496322691 ) ) ;
#68686 = CARTESIAN_POINT ( 'NONE',  ( -81.81951131364591845, -294.9887739415768806, -333.1560331110289894 ) ) ;
#68687 = CARTESIAN_POINT ( 'NONE',  ( -60.45826189183085120, -290.2268603332114481, -200.3337824028981231 ) ) ;
#68688 = CARTESIAN_POINT ( 'NONE',  ( -66.47233124773364921, -293.6788207533389823, -338.4006678459977024 ) ) ;
#68689 = CARTESIAN_POINT ( 'NONE',  ( -110.1817003237764396, -291.6388122862322234, -279.3869074852918288 ) ) ;
#68690 = CYLINDRICAL_SURFACE ( 'NONE', #27883, 1.000000000000000888 ) ;
#68691 = CIRCLE ( 'NONE', #44477, 24.50000000000000355 ) ;
#68692 = CARTESIAN_POINT ( 'NONE',  ( 37.04155763170902560, -291.4088359899499778, -259.1870604028920297 ) ) ;
#68693 = CARTESIAN_POINT ( 'NONE',  ( -66.46688798966675904, -297.4335620590681515, -339.5294755591189073 ) ) ;
#68694 = CARTESIAN_POINT ( 'NONE',  ( 10.27732240190107404, -289.3177175755081976, -326.0684281963970079 ) ) ;
#68695 = CARTESIAN_POINT ( 'NONE',  ( 2.650421355659904332, -278.4989863310857459, -334.2898925820521754 ) ) ;
#68696 = CARTESIAN_POINT ( 'NONE',  ( -5.464077083346287722, -275.4369534850363266, -340.0161671107475740 ) ) ;
#68697 = TOROIDAL_SURFACE ( 'NONE', #27893, 1.000000000000000000, 0.5000000000000000000 ) ;
#68698 = CARTESIAN_POINT ( 'NONE',  ( -3.488617787458530017, -297.6630494814447729, -193.5270647055053246 ) ) ;
#68699 = CARTESIAN_POINT ( 'NONE',  ( 19.95197245330039948, -274.4465989728540194, -317.2362740257074734 ) ) ;
#68700 = CARTESIAN_POINT ( 'NONE',  ( 5.776768445224250037, -278.7215219500786816, -209.6807104091703877 ) ) ;
#68701 = CARTESIAN_POINT ( 'NONE',  ( 26.97713144978790467, -276.2755870676452901, -234.8968034778139611 ) ) ;
#68702 = CARTESIAN_POINT ( 'NONE',  ( -104.2826161255517263, -276.4759916022910033, -306.7665321268673324 ) ) ;
#68703 = CARTESIAN_POINT ( 'NONE',  ( 186.2362647323748206, 276.0000000000000568, 22.80382896336985965 ) ) ;
#68704 = CARTESIAN_POINT ( 'NONE',  ( -85.38338918329472449, -274.0190211939736287, -215.1947441740319391 ) ) ;
#68705 = DIRECTION ( 'NONE',  ( 0.000000000000000000, 0.000000000000000000, -1.000000000000000000 ) ) ;
#68707 = CARTESIAN_POINT ( 'NONE',  ( 11.54809790458018703, -274.5861260988357913, -216.0824656522480609 ) ) ;
#68706 = CARTESIAN_POINT ( 'NONE',  ( -0.1156751476317717242, -286.5799725893410823, -335.9382387648072950 ) ) ;
#68708 = CARTESIAN_POINT ( 'NONE',  ( 36.69122204383213415, -287.2846441276786322, -249.0027959762152818 ) ) ;
#68709 = CARTESIAN_POINT ( 'NONE',  ( -37.28078186119692106, -300.0328001623263958, -195.0051416838755074 ) ) ;
#68710 = CARTESIAN_POINT ( 'NONE',  ( -78.99072894804898226, -293.6145419364606823, -332.5959562351066552 ) ) ;
#68711 = CARTESIAN_POINT ( 'NONE',  ( 37.38892614052306129, -280.9739934559451626, -288.2915573491141572 ) ) ;
#68712 = CARTESIAN_POINT ( 'NONE',  ( 153.3309649087729838, 129.0860594806759423, -12.69538652463440442 ) ) ;
#68713 = CARTESIAN_POINT ( 'NONE',  ( -15.64921055647543113, -278.3325399754585305, -198.5133485269475102 ) ) ;
#68714 = CARTESIAN_POINT ( 'NONE',  ( 186.6539576904058890, 293.9636489450775230, 11.60392986742922439 ) ) ;
#68715 = CARTESIAN_POINT ( 'NONE',  ( -109.8136088346350192, -289.1936160389217889, -282.0571966196503126 ) ) ;
#68716 = CARTESIAN_POINT ( 'NONE',  ( 191.4749582765727212, -21.37379927922774314, 10.00000000000000000 ) ) ;
#68717 = CARTESIAN_POINT ( 'NONE',  ( 195.4781563537916327, 39.36132622696000283, 15.49999999999999645 ) ) ;
#68718 = CARTESIAN_POINT ( 'NONE',  ( -87.24119644184246170, -289.3570090168245201, -214.2998010148533581 ) ) ;
#68719 = CARTESIAN_POINT ( 'NONE',  ( -35.39119581315596008, -275.5971646020306025, -196.6809751414244829 ) ) ;
#68720 = CARTESIAN_POINT ( 'NONE',  ( 35.05668491798139996, -283.2894315467105457, -294.9608900034124304 ) ) ;
#68722 = CARTESIAN_POINT ( 'NONE',  ( -110.2282293906098403, -284.6167374029307098, -265.4652042273821166 ) ) ;
#68721 = CARTESIAN_POINT ( 'NONE',  ( -109.6517776936459114, -270.9144871198463989, -248.2606236157619719 ) ) ;
#68723 = CARTESIAN_POINT ( 'NONE',  ( -16.49095269897191685, -275.7520711298907372, -199.7344720970027652 ) ) ;
#68724 = CARTESIAN_POINT ( 'NONE',  ( -6.470121702911462158, -275.2711590382823488, -204.0320340672124360 ) ) ;
#68725 = CARTESIAN_POINT ( 'NONE',  ( -35.91111981277754239, -285.0343997516923196, -345.3602532887544498 ) ) ;
#68726 = CARTESIAN_POINT ( 'NONE',  ( -100.9792975836874263, -271.9702727400850790, -233.8656324821017165 ) ) ;
#68727 = ORIENTED_EDGE ( 'NONE', *, *, #50389, .T. ) ;
#68728 = DIRECTION ( 'NONE',  ( 1.233581138472395244E-14, 0.000000000000000000, 1.000000000000000000 ) ) ;
#68729 = CARTESIAN_POINT ( 'NONE',  ( 38.06234131800047749, -293.1896170895284399, -254.7006362196658245 ) ) ;
#68730 = CARTESIAN_POINT ( 'NONE',  ( -105.6075976347626550, -286.1346545762723395, -300.5540647970166219 ) ) ;
#68731 = DIRECTION ( 'NONE',  ( -0.9693563597868444237, -0.2456588035076248677, 4.923761215728623624E-16 ) ) ;
#68732 = CARTESIAN_POINT ( 'NONE',  ( -37.37352853689063181, -274.5523547857346784, -350.3611179825600175 ) ) ;
#68733 = CARTESIAN_POINT ( 'NONE',  ( -56.89283428102781670, -276.4951048376808558, -344.7256258353416456 ) ) ;
#68734 = CARTESIAN_POINT ( 'NONE',  ( -109.6650790623762930, -289.2591196847549213, -246.2009382901833874 ) ) ;
#68735 = CARTESIAN_POINT ( 'NONE',  ( -23.92040942575637885, -284.3977116968617338, -342.8219812576328422 ) ) ;
#68736 =( BOUNDED_CURVE ( )  B_SPLINE_CURVE ( 3, ( #17668, #9611, #46521, #75422 ),
 .UNSPECIFIED., .F., .F. ) 
 B_SPLINE_CURVE_WITH_KNOTS ( ( 4, 4 ),
 ( 4.712388980384689674, 6.283185307179586232 ),
 .UNSPECIFIED. ) 
 CURVE ( )  GEOMETRIC_REPRESENTATION_ITEM ( )  RATIONAL_B_SPLINE_CURVE ( ( 1.000000000000000000, 0.8047378541243649375, 0.8047378541243649375, 1.000000000000000000 ) ) 
 REPRESENTATION_ITEM ( '' )  );
#68737 = CARTESIAN_POINT ( 'NONE',  ( -68.44311413856341630, -279.2266082079889316, -337.5366208791062377 ) ) ;
#68738 = CARTESIAN_POINT ( 'NONE',  ( -91.49826719089604410, -286.7245100815020464, -216.4568274653686331 ) ) ;
#68739 = CARTESIAN_POINT ( 'NONE',  ( -39.79139435073248876, -282.0215683023473616, -195.3882684419180862 ) ) ;
#68740 = CARTESIAN_POINT ( 'NONE',  ( 20.03445056607907304, -275.0216763594859231, -218.9312568692113530 ) ) ;
#68741 = CARTESIAN_POINT ( 'NONE',  ( -74.09871668599650718, -277.3600304950582540, -338.0364611039502165 ) ) ;
#68742 =( BOUNDED_CURVE ( )  B_SPLINE_CURVE ( 3, ( #69797, #91066, #56555, #70746 ),
 .UNSPECIFIED., .F., .F. ) 
 B_SPLINE_CURVE_WITH_KNOTS ( ( 4, 4 ),
 ( 1.570796326794894560, 2.004620063563923527 ),
 .UNSPECIFIED. ) 
 CURVE ( )  GEOMETRIC_REPRESENTATION_ITEM ( )  RATIONAL_B_SPLINE_CURVE ( ( 1.000000000000000000, 0.9843778111405746545, 0.9843778111405746545, 1.000000000000000000 ) ) 
 REPRESENTATION_ITEM ( '' )  );
#68743 = CARTESIAN_POINT ( 'NONE',  ( -94.16610388149210564, -297.8018816038778027, -318.4672511339338143 ) ) ;
#68744 = CIRCLE ( 'NONE', #70325, 6.338655513825452559 ) ;
#68745 = CARTESIAN_POINT ( 'NONE',  ( 185.2519943799831879, 3.000000000000000444, -9.000000000000001776 ) ) ;
#68746 = CARTESIAN_POINT ( 'NONE',  ( 204.5044540939250055, -142.7221692137691775, 10.75739200365177695 ) ) ;
#68747 = CARTESIAN_POINT ( 'NONE',  ( -82.21955959476886733, -295.5871815227393995, -209.2526581300645319 ) ) ;
#68748 = CARTESIAN_POINT ( 'NONE',  ( -109.5538390098064951, -277.9133885610037282, -281.4694679879060573 ) ) ;
#68749 = CARTESIAN_POINT ( 'NONE',  ( 17.79308768683785047, -276.0245515724481038, -217.1045054658737854 ) ) ;
#68750 = CARTESIAN_POINT ( 'NONE',  ( -33.20411764481407602, -287.8649705596163813, -196.4130114733624737 ) ) ;
#68751 = CARTESIAN_POINT ( 'NONE',  ( -39.07253318013764698, -296.5936188479102498, -346.6481547039148836 ) ) ;
#68752 = CARTESIAN_POINT ( 'NONE',  ( -101.2882926045836598, -297.1986598968338171, -312.6333417410305628 ) ) ;
#68753 = CARTESIAN_POINT ( 'NONE',  ( -96.58092134334746959, -293.1802604321854346, -224.6364736401502284 ) ) ;
#68754 = CARTESIAN_POINT ( 'NONE',  ( -71.76283344156870214, -277.5960702501733977, -203.8996020374821967 ) ) ;
#68755 = CARTESIAN_POINT ( 'NONE',  ( 26.35606817054642192, -282.9511249409263769, -231.7397465992683863 ) ) ;
#68756 = CARTESIAN_POINT ( 'NONE',  ( -109.5662562372726399, -294.8658824183827392, -252.2832526988492248 ) ) ;
#68757 = CARTESIAN_POINT ( 'NONE',  ( -89.56923641862556451, -285.6388907345217376, -325.3200966539636738 ) ) ;
#68758 = AXIS2_PLACEMENT_3D ( 'NONE', #85075, #35368, #63808 ) ;
#68759 = CARTESIAN_POINT ( 'NONE',  ( 17.12947347674059628, -285.7727784315820827, -221.2799912083861500 ) ) ;
#68760 = CARTESIAN_POINT ( 'NONE',  ( -107.9785293115594556, -267.5055723263413370, -306.7646458841903723 ) ) ;
#68761 = ORIENTED_EDGE ( 'NONE', *, *, #87140, .T. ) ;
#68762 = CARTESIAN_POINT ( 'NONE',  ( -2.172475781232041658, -286.1976899962005518, -206.3105313853950236 ) ) ;
#68763 = ORIENTED_EDGE ( 'NONE', *, *, #26148, .T. ) ;
#68764 = CARTESIAN_POINT ( 'NONE',  ( -27.39849985068416416, -284.0084369012947718, -346.4578404129265436 ) ) ;
#68765 = CARTESIAN_POINT ( 'NONE',  ( -24.59691416342607084, -274.5524353766472245, -198.4091818242210650 ) ) ;
#68766 = CARTESIAN_POINT ( 'NONE',  ( -7.483662960881081183, -285.2298117827686497, -199.7603914629277426 ) ) ;
#68767 = CARTESIAN_POINT ( 'NONE',  ( 39.47492157886362207, -282.4878643230741204, -269.9196205137719744 ) ) ;
#68768 = EDGE_CURVE ( 'NONE', #79604, #72125, #80753, .T. ) ;
#68769 = DIRECTION ( 'NONE',  ( -0.000000000000000000, 1.000000000000000000, -0.000000000000000000 ) ) ;
#68770 = CARTESIAN_POINT ( 'NONE',  ( -84.15696897388352227, -280.9421669263935541, -210.0361406744585508 ) ) ;
#68771 = CARTESIAN_POINT ( 'NONE',  ( 39.61932352314976669, -281.8440618636216755, -267.0540507914810178 ) ) ;
#68772 = CARTESIAN_POINT ( 'NONE',  ( -6.998514795304330072, -286.1237833571631768, -333.4427485647536855 ) ) ;
#68773 = CARTESIAN_POINT ( 'NONE',  ( 186.1196728968302807, 263.2780867284629380, -153.3933332796401317 ) ) ;
#68774 = ORIENTED_EDGE ( 'NONE', *, *, #85141, .F. ) ;
#68775 = CARTESIAN_POINT ( 'NONE',  ( 35.68787887162498862, -277.7632188463565512, -286.7507020004812262 ) ) ;
#68776 = CARTESIAN_POINT ( 'NONE',  ( 196.5064352957230938, 285.3209794444068734, -111.6193314779800971 ) ) ;
#68777 = CARTESIAN_POINT ( 'NONE',  ( 1.271917777350735523, -278.5902660704379059, -206.4198583178948070 ) ) ;
#68778 = CARTESIAN_POINT ( 'NONE',  ( -3.789263988190406884, -294.2488211981072368, -202.1690061756827106 ) ) ;
#68779 = CARTESIAN_POINT ( 'NONE',  ( -34.30525242549934006, -294.3615545954173172, -343.3999614411675338 ) ) ;
#68780 = CARTESIAN_POINT ( 'NONE',  ( -111.5717673097279317, -290.3140031316360705, -250.0769123901437467 ) ) ;
#68781 = DIRECTION ( 'NONE',  ( 0.000000000000000000, 0.000000000000000000, 1.000000000000000000 ) ) ;
#68783 = CARTESIAN_POINT ( 'NONE',  ( -0.6107764770033399238, -286.9556833610751028, -334.4299289185682937 ) ) ;
#68782 = CARTESIAN_POINT ( 'NONE',  ( -111.7363272031165877, -294.9064189675772809, -287.8546757928123156 ) ) ;
#68784 = CARTESIAN_POINT ( 'NONE',  ( 34.84338867194817624, -295.1871566078384035, -252.9812277668234231 ) ) ;
#68785 = CARTESIAN_POINT ( 'NONE',  ( -88.04676812577316980, -286.6396566742880623, -217.1611221501266300 ) ) ;
#68786 = CARTESIAN_POINT ( 'NONE',  ( 39.00438816635619332, -294.5999787890484640, -278.8568824204251086 ) ) ;
#68787 = CARTESIAN_POINT ( 'NONE',  ( -88.93330826803268963, -284.2932877703015606, -322.1650367118525082 ) ) ;
#68788 = CARTESIAN_POINT ( 'NONE',  ( -66.78607382019364991, -294.2243742026189466, -341.0932623691219874 ) ) ;
#68789 = CARTESIAN_POINT ( 'NONE',  ( -114.0895197921789475, -291.3082059912559316, -274.0935430447972294 ) ) ;
#68790 = CARTESIAN_POINT ( 'NONE',  ( -53.38261371696017932, -292.3442006903745778, -195.0589653445444753 ) ) ;
#68791 = CARTESIAN_POINT ( 'NONE',  ( -56.06354280048936545, -289.4666261606691364, -340.9721086161489438 ) ) ;
#68792 = ORIENTED_EDGE ( 'NONE', *, *, #22499, .T. ) ;
#68793 = DIRECTION ( 'NONE',  ( 0.000000000000000000, 0.000000000000000000, 1.000000000000000000 ) ) ;
#68794 = CARTESIAN_POINT ( 'NONE',  ( -98.11605028801338335, -299.0243104460866448, -225.0980612733765156 ) ) ;
#68795 = CARTESIAN_POINT ( 'NONE',  ( -81.01136527582367819, -272.2688100568652203, -207.3606178859388649 ) ) ;
#68796 = EDGE_CURVE ( 'NONE', #24735, #48324, #75398, .T. ) ;
#68797 = CARTESIAN_POINT ( 'NONE',  ( 18.15063361211283421, -279.9322721941948657, -222.5505533467530199 ) ) ;
#68798 = ORIENTED_EDGE ( 'NONE', *, *, #41200, .F. ) ;
#68799 = ORIENTED_EDGE ( 'NONE', *, *, #49105, .F. ) ;
#68800 = CARTESIAN_POINT ( 'NONE',  ( 29.03968615844400247, -275.5665286336129043, -309.2589130072233274 ) ) ;
#68801 = CARTESIAN_POINT ( 'NONE',  ( -104.3409500289874359, -295.4434811899757278, -239.5494696656958240 ) ) ;
#68802 = CARTESIAN_POINT ( 'NONE',  ( -67.27943376017204002, -279.3093880613304805, -338.2919474162719098 ) ) ;
#68803 = CARTESIAN_POINT ( 'NONE',  ( 36.87832963287976185, -273.6722593704744781, -268.8602316538309651 ) ) ;
#68804 = CARTESIAN_POINT ( 'NONE',  ( -96.42905717839009583, -298.3643847634436952, -226.7989390556653007 ) ) ;
#68805 = CARTESIAN_POINT ( 'NONE',  ( -109.6656366116340280, -297.4744831311123221, -282.3391931841145492 ) ) ;
#68806 = DIRECTION ( 'NONE',  ( 0.000000000000000000, 0.000000000000000000, 1.000000000000000000 ) ) ;
#68807 = CARTESIAN_POINT ( 'NONE',  ( -112.6026582454786791, -298.3040396182838663, -258.3523573068501378 ) ) ;
#68808 = CARTESIAN_POINT ( 'NONE',  ( -102.7882370907312577, -271.0692105648158758, -232.9046508698549758 ) ) ;
#68809 = CARTESIAN_POINT ( 'NONE',  ( 34.94004018409767554, -294.3517587600364891, -281.6104475441847512 ) ) ;
#68810 = CARTESIAN_POINT ( 'NONE',  ( -5.772527946748679639, -291.0503147052444319, -203.8734514726233726 ) ) ;
#68811 = CARTESIAN_POINT ( 'NONE',  ( 94.75641758632609424, -301.7060295618178429, -195.3160783195277475 ) ) ;
#68812 = CARTESIAN_POINT ( 'NONE',  ( -5.145730870924443145, -274.9570345914210066, -200.4830351017815815 ) ) ;
#68813 = CARTESIAN_POINT ( 'NONE',  ( -107.9406309504387309, -272.9663396913570068, -251.5987125653890075 ) ) ;
#68814 = CARTESIAN_POINT ( 'NONE',  ( 33.76701217245756936, -283.2088181013708095, -245.2663396428328326 ) ) ;
#68815 = CARTESIAN_POINT ( 'NONE',  ( -31.68953967179505327, -281.6670732206436583, -346.6720817301573447 ) ) ;
#68816 = CARTESIAN_POINT ( 'NONE',  ( -25.79347455145516577, -276.2573182259811801, -346.3871087513002749 ) ) ;
#68817 = CARTESIAN_POINT ( 'NONE',  ( 199.6150009768959990, 275.5000000000000568, -2.367926910627516257 ) ) ;
#68818 = CARTESIAN_POINT ( 'NONE',  ( -96.05743635781752232, -283.1384598110784623, -314.0081573595506939 ) ) ;
#68819 = AXIS2_PLACEMENT_3D ( 'NONE', #92229, #25962, #71419 ) ;
#68820 = CARTESIAN_POINT ( 'NONE',  ( 36.98587463082740356, -279.4041693611255255, -258.8227859101094737 ) ) ;
#68821 = CARTESIAN_POINT ( 'NONE',  ( 35.68852752380548310, -274.2506524425070893, -279.8199299924288539 ) ) ;
#68822 = CARTESIAN_POINT ( 'NONE',  ( -105.7063685277205565, -280.9582691590790660, -239.3937158058713806 ) ) ;
#68823 = CARTESIAN_POINT ( 'NONE',  ( 186.6539576904058890, 276.0000000000000568, -11.60392986742922439 ) ) ;
#68824 = CARTESIAN_POINT ( 'NONE',  ( 195.5396684847816573, 20.94006894122355433, 14.59130073475925116 ) ) ;
#68825 = CARTESIAN_POINT ( 'NONE',  ( -104.8902391374355432, -271.4130410592724729, -234.9819204281583040 ) ) ;
#68826 = AXIS2_PLACEMENT_3D ( 'NONE', #29418, #16587, #87151 ) ;
#68827 = CARTESIAN_POINT ( 'NONE',  ( -110.3873860473396604, -280.3244698023506203, -288.1450483035851562 ) ) ;
#68828 = CARTESIAN_POINT ( 'NONE',  ( 115.2448031289451222, -299.5541904835127980, -195.3611179825600175 ) ) ;
#68829 = CARTESIAN_POINT ( 'NONE',  ( -80.71459139261448001, -285.5551912867497890, -332.2964514654198069 ) ) ;
#68830 = CARTESIAN_POINT ( 'NONE',  ( 209.2651480440030980, 38.13450996287912886, 14.02415587114431617 ) ) ;
#68831 = CARTESIAN_POINT ( 'NONE',  ( -42.20800475863909895, -287.1133227628986333, -345.2158272255558131 ) ) ;
#68832 = CIRCLE ( 'NONE', #71895, 1.999999999999996003 ) ;
#68833 = CARTESIAN_POINT ( 'NONE',  ( 156.1711712139736505, 21.00000000000000000, 14.59590564729795226 ) ) ;
#68834 = CARTESIAN_POINT ( 'NONE',  ( -107.8364880520261835, -295.6159085010800140, -249.9254780138570027 ) ) ;
#68835 = CARTESIAN_POINT ( 'NONE',  ( -23.57903063128033949, -287.0141106076861206, -343.3619879842859746 ) ) ;
#68836 = CARTESIAN_POINT ( 'NONE',  ( 158.5846220834698670, 17.78059845260474248, -9.675371801486436496 ) ) ;
#68837 = CARTESIAN_POINT ( 'NONE',  ( -87.41722264350329397, -295.3534229690173447, -214.5270540879756709 ) ) ;
#68838 = CARTESIAN_POINT ( 'NONE',  ( -40.76580597458836053, -284.4898354643546554, -194.0795885639085441 ) ) ;
#68839 = CARTESIAN_POINT ( 'NONE',  ( -8.958294350829858033, -282.0298461185421957, -202.2375340144853624 ) ) ;
#68840 = CARTESIAN_POINT ( 'NONE',  ( 12.99255351634633548, -280.6007779521450516, -327.3559727052530661 ) ) ;
#68841 = CARTESIAN_POINT ( 'NONE',  ( -29.17312194119513791, -288.9457509618566178, -342.9026531910508879 ) ) ;
#68842 = CARTESIAN_POINT ( 'NONE',  ( -108.5472971228495709, -280.2213261818041019, -251.7336861317283194 ) ) ;
#68843 = CARTESIAN_POINT ( 'NONE',  ( -81.39323883506125412, -280.2387028243218765, -211.8846254143956855 ) ) ;
#68844 = CARTESIAN_POINT ( 'NONE',  ( 19.35243163830423896, -290.2184173490053354, -320.0210953710667923 ) ) ;
#68845 = VERTEX_POINT ( 'NONE', #66489 ) ;
#68846 = CARTESIAN_POINT ( 'NONE',  ( -44.04275839310808749, -273.9697827263126442, -193.5999494752568921 ) ) ;
#68847 = CARTESIAN_POINT ( 'NONE',  ( -110.0349201090081408, -292.7515248190919124, -253.3482171182604930 ) ) ;
#68848 = CARTESIAN_POINT ( 'NONE',  ( -111.2586520408596868, -298.6233781216987495, -305.9938812882205070 ) ) ;
#68849 = ORIENTED_EDGE ( 'NONE', *, *, #2914, .T. ) ;
#68850 = CARTESIAN_POINT ( 'NONE',  ( 35.11150258591253248, -273.8093906609569217, -290.4230913517876616 ) ) ;
#68851 = CARTESIAN_POINT ( 'NONE',  ( 144.7857639756989272, -299.5541904835127980, -189.7068768330456123 ) ) ;
#68852 = CARTESIAN_POINT ( 'NONE',  ( -94.98976197696771351, -294.2718370863009341, -320.1922466267114373 ) ) ;
#68853 = CARTESIAN_POINT ( 'NONE',  ( -67.09140211203794024, -273.0001545457404291, -203.5728015461282325 ) ) ;
#68854 = CARTESIAN_POINT ( 'NONE',  ( -72.67443622358190680, -291.0492125653405537, -335.0318649508368480 ) ) ;
#68855 = CARTESIAN_POINT ( 'NONE',  ( -51.18576187134640776, -284.9915413161372157, -343.1204637525321459 ) ) ;
#68856 = CARTESIAN_POINT ( 'NONE',  ( -92.40020871325489793, -292.7089727706038502, -217.3031190158896493 ) ) ;
#68857 = CARTESIAN_POINT ( 'NONE',  ( 3.861746285214376240, -293.9092649499620507, -205.8345868115563633 ) ) ;
#68858 = CARTESIAN_POINT ( 'NONE',  ( 33.95026548985166670, -293.1776144409390099, -254.6044039904427052 ) ) ;
#68859 = CARTESIAN_POINT ( 'NONE',  ( -95.69373833104647531, -287.2010402676939975, -223.2234507385051074 ) ) ;
#68860 = CARTESIAN_POINT ( 'NONE',  ( 15.75506794078392403, -282.4916337534894524, -326.1261000513601971 ) ) ;
#68861 = CARTESIAN_POINT ( 'NONE',  ( -70.20412056124072819, -293.5615406150545255, -338.4148729281706096 ) ) ;
#68862 = CARTESIAN_POINT ( 'NONE',  ( -95.33613207595536210, -283.7004270802664792, -321.0133229450572117 ) ) ;
#68863 = CARTESIAN_POINT ( 'NONE',  ( 28.06590198351766219, -277.0502787984133874, -234.2855206176445790 ) ) ;
#68864 = CARTESIAN_POINT ( 'NONE',  ( 17.40634833298267736, -290.6948066931273047, -313.9805196606274080 ) ) ;
#68865 = CARTESIAN_POINT ( 'NONE',  ( -105.2489764546544819, -276.2515413668471638, -304.0784449347737564 ) ) ;
#68866 = DIRECTION ( 'NONE',  ( 0.000000000000000000, 0.000000000000000000, -1.000000000000000000 ) ) ;
#68867 = CARTESIAN_POINT ( 'NONE',  ( -40.24307391747935014, -282.5972550986023748, -343.3650252200162640 ) ) ;
#68868 = CARTESIAN_POINT ( 'NONE',  ( -39.59105578060906794, -281.2295985340695097, -193.7782378419589975 ) ) ;
#68869 = CARTESIAN_POINT ( 'NONE',  ( 36.91375762869408561, -286.8553261888745283, -289.8276843707673152 ) ) ;
#68870 = CARTESIAN_POINT ( 'NONE',  ( -32.10769235822609602, -293.8791896603459577, -196.5202846107300445 ) ) ;
#68871 = CARTESIAN_POINT ( 'NONE',  ( 22.03063201690669359, -277.7993008343123620, -318.1454180215478686 ) ) ;
#68872 = CARTESIAN_POINT ( 'NONE',  ( 34.74201150433786012, -277.1947289564130301, -296.1540006689463667 ) ) ;
#68873 = CARTESIAN_POINT ( 'NONE',  ( -72.84386188793519068, -277.3697397097414523, -334.1610509284795398 ) ) ;
#68874 = CARTESIAN_POINT ( 'NONE',  ( -111.5231057501210472, -274.6391852789947166, -262.0565492657142386 ) ) ;
#68875 = CARTESIAN_POINT ( 'NONE',  ( -111.4236459266276853, -282.6881124386372335, -259.7831345562686352 ) ) ;
#68876 = CARTESIAN_POINT ( 'NONE',  ( -56.17950392809218130, -291.4827602418790207, -195.6678482789587292 ) ) ;
#68877 = CARTESIAN_POINT ( 'NONE',  ( -9.832929372396007395, -290.2988956171479344, -341.4224150921079399 ) ) ;
#68878 = CARTESIAN_POINT ( 'NONE',  ( 15.10623187868024075, -291.7338887116835053, -219.0688635841866869 ) ) ;
#68879 = ORIENTED_EDGE ( 'NONE', *, *, #11367, .F. ) ;
#68880 = CARTESIAN_POINT ( 'NONE',  ( 31.66172632871591830, -291.7015746722387917, -237.4183817063719459 ) ) ;
#68881 = CARTESIAN_POINT ( 'NONE',  ( -2.425592560932005259, -292.1942915473235303, -206.2146103394824195 ) ) ;
#68882 = ORIENTED_EDGE ( 'NONE', *, *, #18976, .T. ) ;
#68883 = CARTESIAN_POINT ( 'NONE',  ( -7.029398635054750599, -289.7433279682696821, -340.8214298497816230 ) ) ;
#68884 = CARTESIAN_POINT ( 'NONE',  ( -103.4655885512649292, -279.6255503964544005, -239.0728292689274497 ) ) ;
#68885 = CARTESIAN_POINT ( 'NONE',  ( -107.4847219664850400, -295.8711797101441903, -239.2226317391341297 ) ) ;
#68886 = CARTESIAN_POINT ( 'NONE',  ( -15.45042789957055973, -286.9795465448964933, -196.5895546472412718 ) ) ;
#68887 = ADVANCED_FACE ( 'NONE', ( #8698 ), #45136, .F. ) ;
#68888 = CARTESIAN_POINT ( 'NONE',  ( -12.71449119069791855, -286.6970519834939068, -197.4279645375964094 ) ) ;
#68889 = CARTESIAN_POINT ( 'NONE',  ( -104.1309284958072112, -284.4883085933072948, -299.8786798860649014 ) ) ;
#68890 = CARTESIAN_POINT ( 'NONE',  ( -104.4934034522946718, -256.0290196201358413, -326.6823371243384031 ) ) ;
#68891 = CARTESIAN_POINT ( 'NONE',  ( 166.3698261927351894, 232.4625470284710218, -191.7400226694176695 ) ) ;
#68892 = CARTESIAN_POINT ( 'NONE',  ( -111.6100336445428240, -270.6909421912098423, -270.3374203212270004 ) ) ;
#68893 = CARTESIAN_POINT ( 'NONE',  ( 13.61643884026687168, -273.9857543381705796, -217.8647390635576073 ) ) ;
#68894 = CARTESIAN_POINT ( 'NONE',  ( 34.67974540479879408, -274.2927788890602869, -256.6812986239779093 ) ) ;
#68895 = CARTESIAN_POINT ( 'NONE',  ( -78.16449755504908126, -297.0263985776559252, -205.1458888302250330 ) ) ;
#68896 = CARTESIAN_POINT ( 'NONE',  ( 180.6035871466845322, 251.0332377899103165, -164.5909838749037135 ) ) ;
#68897 = CARTESIAN_POINT ( 'NONE',  ( 34.73072401280766996, -274.5648047631371469, -296.1855194985085404 ) ) ;
#68898 = CARTESIAN_POINT ( 'NONE',  ( -83.84442522790524777, -275.1635020853752849, -212.7809949437168768 ) ) ;
#68899 = EDGE_LOOP ( 'NONE', ( #86134, #13344, #48209, #21718 ) ) ;
#68900 = CARTESIAN_POINT ( 'NONE',  ( -95.80102097273827155, -274.3038306074657839, -220.7021960780265886 ) ) ;
#68901 = CIRCLE ( 'NONE', #40135, 5.568361562975243650 ) ;
#68902 = CARTESIAN_POINT ( 'NONE',  ( -108.4088176238139454, -290.8210112048931251, -287.3155643822057073 ) ) ;
#68903 = CARTESIAN_POINT ( 'NONE',  ( -102.9723425791615483, -296.8320857822657786, -310.3208175766178556 ) ) ;
#68904 = CARTESIAN_POINT ( 'NONE',  ( -100.7035475187257703, -297.6214020476631390, -226.6939116994128938 ) ) ;
#68905 = CARTESIAN_POINT ( 'NONE',  ( -9.228919109890636463, -294.8407892609643568, -337.7443874408109536 ) ) ;
#68906 = EDGE_LOOP ( 'NONE', ( #26942, #44661 ) ) ;
#68907 = CARTESIAN_POINT ( 'NONE',  ( -97.63923743152092527, -279.8540450261616570, -315.9182779660990832 ) ) ;
#68908 = EDGE_CURVE ( 'NONE', #5915, #93421, #59626, .T. ) ;
#68909 = ORIENTED_EDGE ( 'NONE', *, *, #86488, .F. ) ;
#68910 = CARTESIAN_POINT ( 'NONE',  ( -35.33134803361723186, -279.5843755276557658, -193.4357990271597316 ) ) ;
#68911 = B_SPLINE_CURVE_WITH_KNOTS ( 'NONE', 3,
 ( #80092, #37009, #44090, #7204, #1481, #36079, #43636, #35625, #64997, #100, #15234, #78706, #28979, #59255, #65922, #20941, #57864, #86720, #72534, #13848, #7653, #28516, #29454, #58342, #87184, #64540, #93366, #51204, #72994, #1034, #87640 ),
 .UNSPECIFIED., .F., .F.,
 ( 4, 2, 2, 2, 2, 2, 2, 2, 2, 2, 2, 1, 2, 2, 2, 4 ),
 ( 0.000000000000000000, 0.006842209725270028201, 0.01026331458790513164, 0.01368441945054023508, 0.02052662917581044369, 0.02223718160712799194, 0.02394773403844554713, 0.02736883890108088302, 0.03421104862635143684, 0.03592160105766905448, 0.03763215348898667212, 0.04105325835162196985, 0.04447436321425726757, 0.04618491564557489909, 0.04789546807689253061, 0.05473767780216309137 ),
 .UNSPECIFIED. ) ;
#68912 = CARTESIAN_POINT ( 'NONE',  ( -48.63232638649421347, -278.1405619872154489, -342.7723992473208909 ) ) ;
#68913 = CARTESIAN_POINT ( 'NONE',  ( 38.61729267791743325, -277.2863043842763204, -268.3104051183530601 ) ) ;
#68914 = CARTESIAN_POINT ( 'NONE',  ( -112.7395859938250169, -276.5569796260549538, -271.5565909009673646 ) ) ;
#68915 = CARTESIAN_POINT ( 'NONE',  ( -106.3665758327925630, -273.3627330007209366, -246.4121101625442236 ) ) ;
#68916 = CARTESIAN_POINT ( 'NONE',  ( -108.6056013527174997, -271.2798114442667270, -251.3995940395351454 ) ) ;
#68917 = CARTESIAN_POINT ( 'NONE',  ( -107.6188887331644253, -278.9804637243246361, -250.5634092380568063 ) ) ;
#68918 = CARTESIAN_POINT ( 'NONE',  ( -9.756862339182497124, -287.3840636236464547, -341.7219965988486479 ) ) ;
#68919 = CARTESIAN_POINT ( 'NONE',  ( -62.90011178328097685, -275.7195489672476469, -199.8503511327572539 ) ) ;
#68920 = CARTESIAN_POINT ( 'NONE',  ( 188.7149167944524493, -12.49482340714361506, -3.999999999999998224 ) ) ;
#68921 = CARTESIAN_POINT ( 'NONE',  ( -100.4484019759146634, -289.2409949684019921, -307.4764043590747633 ) ) ;
#68922 = EDGE_CURVE ( 'NONE', #47563, #34997, #52026, .T. ) ;
#68923 = CARTESIAN_POINT ( 'NONE',  ( -111.3955503567632803, -283.6407571029802170, -291.0816404924456151 ) ) ;
#68924 = CARTESIAN_POINT ( 'NONE',  ( -1.963742169635317669, -280.8167700189771381, -335.3861727691576107 ) ) ;
#68926 = CARTESIAN_POINT ( 'NONE',  ( -70.60435852157448267, -283.6899729326881925, -203.7517825457707659 ) ) ;
#68925 = CARTESIAN_POINT ( 'NONE',  ( 22.60393719647837329, -279.5354195512760498, -227.6774503367744842 ) ) ;
#68927 = CARTESIAN_POINT ( 'NONE',  ( 35.28611634801455921, -289.7933428701097114, -289.1253899940311385 ) ) ;
#68928 = CARTESIAN_POINT ( 'NONE',  ( -105.6316608028370325, -279.3994312439810415, -297.2611509760015451 ) ) ;
#68929 = CARTESIAN_POINT ( 'NONE',  ( -114.0438014563954710, -273.4268578562636662, -284.1485097187775182 ) ) ;
#68930 = CARTESIAN_POINT ( 'NONE',  ( -71.29035959423477209, -293.6041527609718287, -203.4702246659599894 ) ) ;
#68931 = CARTESIAN_POINT ( 'NONE',  ( -25.53070151702314661, -278.4405457324816098, -195.2979823992891113 ) ) ;
#68932 = CARTESIAN_POINT ( 'NONE',  ( -69.28848268271894995, -278.1352935113894773, -336.1267475058205605 ) ) ;
#68933 = CARTESIAN_POINT ( 'NONE',  ( -11.31240767397753899, -284.7141020944063143, -340.9324098505744587 ) ) ;
#68934 = CARTESIAN_POINT ( 'NONE',  ( 184.7149167944524493, 8.542400036368780647, 10.00000000000000178 ) ) ;
#68935 = CARTESIAN_POINT ( 'NONE',  ( -40.25822760372736298, -291.0086644611014322, -345.8776510268894526 ) ) ;
#68936 = CARTESIAN_POINT ( 'NONE',  ( -90.62632059579011923, -295.2973389989725774, -217.5088008853391557 ) ) ;
#68937 = CARTESIAN_POINT ( 'NONE',  ( 24.57922159140330365, -286.1437314727256762, -224.8643238726434106 ) ) ;
#68938 = CARTESIAN_POINT ( 'NONE',  ( -65.61480225624852380, -290.0760341272024903, -202.1780208905026655 ) ) ;
#68939 = DIRECTION ( 'NONE',  ( 0.000000000000000000, 0.000000000000000000, 1.000000000000000000 ) ) ;
#68940 = CARTESIAN_POINT ( 'NONE',  ( -18.90932575960783169, -275.4946553913699745, -341.5052748176499335 ) ) ;
#68941 = CARTESIAN_POINT ( 'NONE',  ( -38.38298836310534767, -293.2049259984099194, -344.5890184130745979 ) ) ;
#68942 = CARTESIAN_POINT ( 'NONE',  ( 195.5424455875674425, 40.24675177650068036, 14.87863167422141153 ) ) ;
#68943 = LINE ( 'NONE', #54249, #21704 ) ;
#68944 = CARTESIAN_POINT ( 'NONE',  ( -58.72567299283868181, -290.2603453682210670, -197.1119988365325071 ) ) ;
#68945 = CARTESIAN_POINT ( 'NONE',  ( -110.4071043827411245, -286.2878204282607726, -259.9742456721976396 ) ) ;
#68946 = CARTESIAN_POINT ( 'NONE',  ( -77.61855095521517001, -287.8243273861113494, -334.8565760528361466 ) ) ;
#68947 = CARTESIAN_POINT ( 'NONE',  ( -72.67272803051490371, -286.9999027482505198, -205.7937574203843667 ) ) ;
#68948 = CARTESIAN_POINT ( 'NONE',  ( 183.0442525570908288, 264.6571197653884155, -7.500000000000000000 ) ) ;
#68949 = CARTESIAN_POINT ( 'NONE',  ( -67.62384642560651571, -286.4471729718327992, -203.7608676596886426 ) ) ;
#68950 = CARTESIAN_POINT ( 'NONE',  ( 35.51295101858538317, -295.7783054081259024, -289.6122637093188246 ) ) ;
#68951 = CARTESIAN_POINT ( 'NONE',  ( -110.4406884240068223, -276.3874328452529880, -289.5392829052302091 ) ) ;
#68952 = CARTESIAN_POINT ( 'NONE',  ( 37.61334982015772255, -275.6654163587709263, -252.7685477816147284 ) ) ;
#68953 = CARTESIAN_POINT ( 'NONE',  ( -7.731537073715645469, -290.5170120279115054, -200.8304994624267010 ) ) ;
#68954 = CARTESIAN_POINT ( 'NONE',  ( -114.2320067192800934, -278.5007682141953183, -274.4697372532468762 ) ) ;
#68955 = CARTESIAN_POINT ( 'NONE',  ( -110.1917356009836766, -298.3221409579185206, -286.6313097050213514 ) ) ;
#68956 = CARTESIAN_POINT ( 'NONE',  ( -48.18343439339133027, -279.1747503396363186, -502.4506777725899838 ) ) ;
#68957 = CARTESIAN_POINT ( 'NONE',  ( 223.4306832106270804, -134.2391364535880882, -21.50000000000000000 ) ) ;
#68958 = CARTESIAN_POINT ( 'NONE',  ( -106.4258079636003487, -276.3344332384846780, -297.5319023446353981 ) ) ;
#68959 = CARTESIAN_POINT ( 'NONE',  ( 24.64246932113718813, -278.9792107225019890, -228.0453069640036290 ) ) ;
#68960 = CARTESIAN_POINT ( 'NONE',  ( -36.09237171215954021, -122.5496321078137356, 22.50000000000000000 ) ) ;
#68961 = CARTESIAN_POINT ( 'NONE',  ( -0.3643162538074650736, -273.0144120578602269, -203.5976188485319369 ) ) ;
#68962 = AXIS2_PLACEMENT_3D ( 'NONE', #65298, #80390, #87029 ) ;
#68963 = CARTESIAN_POINT ( 'NONE',  ( -111.0775633625152352, -298.0574923514698185, -271.4929015331194933 ) ) ;
#68964 = CARTESIAN_POINT ( 'NONE',  ( 29.48576758952929211, -280.9638427208157623, -308.0935365075171717 ) ) ;
#68965 = CARTESIAN_POINT ( 'NONE',  ( -110.4478753724393272, -297.5505683042409828, -266.0142123389778703 ) ) ;
#68966 = CARTESIAN_POINT ( 'NONE',  ( -111.7983145776895526, -298.0887743147670790, -252.7681978257350579 ) ) ;
#68967 = CARTESIAN_POINT ( 'NONE',  ( -21.92542755902348972, -273.9219088088029253, -198.9858699847102343 ) ) ;
#68968 = CARTESIAN_POINT ( 'NONE',  ( 35.23739184658464296, -295.3094169996229539, -251.4593704465850124 ) ) ;
#68969 = CARTESIAN_POINT ( 'NONE',  ( 22.99056205213839021, -287.0783802454094484, -222.4964187186883748 ) ) ;
#68970 = CARTESIAN_POINT ( 'NONE',  ( 38.38764741312459705, -273.7380947504636310, -274.0085121470153808 ) ) ;
#68971 = CARTESIAN_POINT ( 'NONE',  ( -8.235099443345465176, -288.5147215272406243, -341.6621696271678843 ) ) ;
#68972 = EDGE_CURVE ( 'NONE', #26019, #90518, #38426, .T. ) ;
#68973 = CARTESIAN_POINT ( 'NONE',  ( 35.68552585476193428, -286.6917875895680368, -276.5129934439735848 ) ) ;
#68974 = CARTESIAN_POINT ( 'NONE',  ( -87.29786058700643991, -289.3554763249453003, -214.4202324127716111 ) ) ;
#68975 = ORIENTED_EDGE ( 'NONE', *, *, #63823, .F. ) ;
#68976 = CARTESIAN_POINT ( 'NONE',  ( -45.58595926748305516, -157.7977398304416283, -369.2266198007532125 ) ) ;
#68977 = CARTESIAN_POINT ( 'NONE',  ( -15.83951863778704983, -288.2741619087357208, -340.2398024371093470 ) ) ;
#68978 = CARTESIAN_POINT ( 'NONE',  ( 200.6103193995254230, 249.5000000000000568, -2.464576988612307229 ) ) ;
#68979 = CARTESIAN_POINT ( 'NONE',  ( -94.21674153619659364, -284.7906799391855088, -321.9368889303878518 ) ) ;
#68980 = CARTESIAN_POINT ( 'NONE',  ( 37.19636038565180058, -292.3805872585965062, -252.0063434334399233 ) ) ;
#68981 = CARTESIAN_POINT ( 'NONE',  ( 23.10017023616907750, -282.5265307403540760, -223.9369996643913794 ) ) ;
#68982 = CARTESIAN_POINT ( 'NONE',  ( 38.30453210848756385, -282.7189687946499816, -258.5748521250762337 ) ) ;
#68983 = CARTESIAN_POINT ( 'NONE',  ( -90.74290821453503497, -283.6697172377529341, -320.1337106357008224 ) ) ;
#68984 = CARTESIAN_POINT ( 'NONE',  ( -70.10265834386611061, -279.4838224160689037, -337.8417703598986463 ) ) ;
#68985 = CARTESIAN_POINT ( 'NONE',  ( -105.2536086688994601, -297.0223986164335201, -233.9578916741046157 ) ) ;
#68986 = CARTESIAN_POINT ( 'NONE',  ( -36.74880309919144850, -275.3749310985004399, -196.8578584263821369 ) ) ;
#68987 = CARTESIAN_POINT ( 'NONE',  ( -105.5609628390411103, -288.1718896738771036, -300.7870317829269311 ) ) ;
#68988 = CARTESIAN_POINT ( 'NONE',  ( -92.30538224948728043, -272.0383219201071938, -221.7182957665462482 ) ) ;
#68989 = VERTEX_POINT ( 'NONE', #59859 ) ;
#68990 = CARTESIAN_POINT ( 'NONE',  ( -112.3417001280813707, -270.0523547857346784, -270.3292895737545223 ) ) ;
#68991 = CARTESIAN_POINT ( 'NONE',  ( -109.8218912173550592, -286.2521355777659551, -287.3854109486860580 ) ) ;
#68992 = CARTESIAN_POINT ( 'NONE',  ( 24.64458364532417178, -295.2338065494631110, -315.5406699309430110 ) ) ;
#68993 = CARTESIAN_POINT ( 'NONE',  ( -95.19202472406374227, -284.5749892476611649, -315.0719572128637083 ) ) ;
#68994 = CARTESIAN_POINT ( 'NONE',  ( 31.63857023217360620, -275.0460832957413686, -304.1651247615131410 ) ) ;
#68995 = CARTESIAN_POINT ( 'NONE',  ( -105.9169724211796932, -291.6534497624328424, -235.4479266698207311 ) ) ;
#68996 = CARTESIAN_POINT ( 'NONE',  ( -112.3794791970542803, -282.5539312781099284, -281.2032826568294013 ) ) ;
#68997 = CARTESIAN_POINT ( 'NONE',  ( 17.47156745347409768, -293.1422438658657939, -216.2374740188380713 ) ) ;
#68998 = CARTESIAN_POINT ( 'NONE',  ( -109.8099774705498390, -290.7671582998805775, -279.3297447321289155 ) ) ;
#68999 = CARTESIAN_POINT ( 'NONE',  ( 196.4324178900849347, 72.07371985372441259, 11.29105239310641018 ) ) ;
#69000 = PLANE ( 'NONE',  #31188 ) ;
#69001 = CARTESIAN_POINT ( 'NONE',  ( -46.92665465413691095, -155.5347905584845876, -361.4716131824436047 ) ) ;
#69002 = CARTESIAN_POINT ( 'NONE',  ( 23.71210760700578746, -283.6869792227523135, -316.1338207159045055 ) ) ;
#69003 = CARTESIAN_POINT ( 'NONE',  ( -19.11405058567864046, -274.3380690714489560, -350.3683826091709648 ) ) ;
#69004 = VERTEX_POINT ( 'NONE', #696 ) ;
#69005 = CARTESIAN_POINT ( 'NONE',  ( 35.82923101673086563, -280.4133757932644926, -265.8621282895097693 ) ) ;
#69006 = CARTESIAN_POINT ( 'NONE',  ( 29.07556193523780053, -275.7255690293050066, -309.2775873942426870 ) ) ;
#69007 = CARTESIAN_POINT ( 'NONE',  ( -60.32020819313539306, -281.7538362510173329, -199.0883761885025081 ) ) ;
#69008 = CARTESIAN_POINT ( 'NONE',  ( 203.3621511278661558, 290.5486715743153923, -82.72705405358787800 ) ) ;
#69009 = CARTESIAN_POINT ( 'NONE',  ( -87.94501165638187956, -282.3179127923633018, -327.6848262233436913 ) ) ;
#69010 = CARTESIAN_POINT ( 'NONE',  ( -108.9773741398122979, -282.3002752627718905, -291.3872042961274929 ) ) ;
#69011 = CARTESIAN_POINT ( 'NONE',  ( -30.61915173512961630, -299.8953510805454812, -194.3724624115683923 ) ) ;
#69012 = CARTESIAN_POINT ( 'NONE',  ( -96.45451462719987035, -296.4438331992726603, -313.3203735610517242 ) ) ;
#69013 = ORIENTED_EDGE ( 'NONE', *, *, #70809, .T. ) ;
#69014 = CARTESIAN_POINT ( 'NONE',  ( 35.20341932327453094, -292.0817637824853250, -258.5158738245784775 ) ) ;
#69015 = CARTESIAN_POINT ( 'NONE',  ( 24.29093874842557454, -276.8161051338233847, -316.3473182172350562 ) ) ;
#69016 = CARTESIAN_POINT ( 'NONE',  ( 23.79349837878535112, -274.9993523650677503, -230.4676660947376092 ) ) ;
#69017 = CARTESIAN_POINT ( 'NONE',  ( 27.38054430966980846, -275.0149838859649094, -311.6000957578334010 ) ) ;
#69018 = DIRECTION ( 'NONE',  ( -0.01818181818181330636, 0.000000000000000000, 0.9998346970812744816 ) ) ;
#69019 = CARTESIAN_POINT ( 'NONE',  ( -91.93800927802118395, -271.2728727457489413, -218.9203180104351816 ) ) ;
#69020 = FACE_OUTER_BOUND ( 'NONE', #13957, .T. ) ;
#69021 = CARTESIAN_POINT ( 'NONE',  ( -43.43856716719556488, -259.1383543305317971, -498.2227791763972391 ) ) ;
#69022 = CARTESIAN_POINT ( 'NONE',  ( 34.24522837432861166, -282.8393326364432028, -286.1578816472051017 ) ) ;
#69023 = CARTESIAN_POINT ( 'NONE',  ( 1.594404928357462392, -284.2992462796009363, -335.6141158939761340 ) ) ;
#69024 = CARTESIAN_POINT ( 'NONE',  ( -93.32782825662420123, -284.5673319346022367, -223.3563722043860196 ) ) ;
#69025 = CARTESIAN_POINT ( 'NONE',  ( -69.61951093316086769, -275.8841165099086652, -336.7421432443401272 ) ) ;
#69026 = CARTESIAN_POINT ( 'NONE',  ( 32.52502979169417330, -283.7429237958347699, -295.6031913031487761 ) ) ;
#69027 = CARTESIAN_POINT ( 'NONE',  ( -48.73394337978491819, -275.6795843013470630, -343.2204453836848188 ) ) ;
#69028 = CARTESIAN_POINT ( 'NONE',  ( 26.90081100285147642, -276.1502029206625934, -234.9406850904321402 ) ) ;
#69029 = CARTESIAN_POINT ( 'NONE',  ( 194.9193168125297575, 41.63678119477545181, 13.72372309788986300 ) ) ;
#69030 = CARTESIAN_POINT ( 'NONE',  ( -113.9172619976245073, -279.2676864613799239, -277.3266344729814818 ) ) ;
#69031 = ADVANCED_FACE ( 'NONE', ( #52714 ), #73589, .T. ) ;
#69032 = ORIENTED_EDGE ( 'NONE', *, *, #55137, .T. ) ;
#69033 = ORIENTED_EDGE ( 'NONE', *, *, #73101, .T. ) ;
#69034 = CARTESIAN_POINT ( 'NONE',  ( 197.0984808611917458, 19.93437704977205982, 12.12215979493358908 ) ) ;
#69035 = CARTESIAN_POINT ( 'NONE',  ( -99.98873105979056675, -286.9846712174409049, -227.6578967912818143 ) ) ;
#69036 = CARTESIAN_POINT ( 'NONE',  ( -84.59016397018206135, -294.9194389820477795, -326.2862533417253985 ) ) ;
#69037 = EDGE_CURVE ( 'NONE', #84462, #85293, #18782, .T. ) ;
#69038 = CARTESIAN_POINT ( 'NONE',  ( -99.94323740639396192, -290.4930371838918859, -225.7028565169545402 ) ) ;
#69039 = CARTESIAN_POINT ( 'NONE',  ( 36.00340951498611020, -285.6580138479193351, -260.0627904844827185 ) ) ;
#69041 = CARTESIAN_POINT ( 'NONE',  ( -88.61667236855386420, -289.5611182563358170, -216.9156809169514588 ) ) ;
#69040 = CARTESIAN_POINT ( 'NONE',  ( 0.4870118026387388888, -285.1412635069577846, -207.1798879602125112 ) ) ;
#69042 = CARTESIAN_POINT ( 'NONE',  ( -110.3911967564691992, -285.8574363530156575, -262.7239055372378971 ) ) ;
#69043 = CARTESIAN_POINT ( 'NONE',  ( 37.55865725566398083, -273.4907655324512348, -265.5929878854221329 ) ) ;
#69044 = CARTESIAN_POINT ( 'NONE',  ( -15.62177554798462786, -284.7283674343338475, -197.2673661383413730 ) ) ;
#69045 = CARTESIAN_POINT ( 'NONE',  ( -77.16271645649362654, -299.5185044682058901, -206.8057302778058215 ) ) ;
#69046 = CARTESIAN_POINT ( 'NONE',  ( 28.53733591518565049, -285.0705969524191801, -234.0593931626272592 ) ) ;
#69047 = CARTESIAN_POINT ( 'NONE',  ( 30.23400950511711827, -282.1159319646882864, -242.1311354273028087 ) ) ;
#69048 = CARTESIAN_POINT ( 'NONE',  ( -90.28862254023624700, -291.7987423674472893, -323.7883355087533914 ) ) ;
#69049 = DIRECTION ( 'NONE',  ( -0.000000000000000000, 1.000000000000000000, -0.000000000000000000 ) ) ;
#69050 = DIRECTION ( 'NONE',  ( 0.000000000000000000, 1.000000000000000000, 0.000000000000000000 ) ) ;
#69051 = CARTESIAN_POINT ( 'NONE',  ( -36.26987921769980261, -296.9589985929893032, -345.9263780219752675 ) ) ;
#69052 = CARTESIAN_POINT ( 'NONE',  ( -8.454100406568541004, -278.4301387991229717, -201.1476277317395898 ) ) ;
#69053 = CARTESIAN_POINT ( 'NONE',  ( -70.81810795460187080, -290.8188877708287805, -201.1983466351589982 ) ) ;
#69054 = CARTESIAN_POINT ( 'NONE',  ( -93.70644615886274664, -294.2821684150115971, -318.0195078357724583 ) ) ;
#69055 = CARTESIAN_POINT ( 'NONE',  ( 19.22634219515002485, -279.5758764286661631, -223.4235660725706509 ) ) ;
#69056 = CARTESIAN_POINT ( 'NONE',  ( -18.89152418481160467, -272.3712197867750433, -198.1903506020499606 ) ) ;
#69057 = CARTESIAN_POINT ( 'NONE',  ( 34.25965969912002151, -295.0850742414888259, -286.9843176487187861 ) ) ;
#69058 = CARTESIAN_POINT ( 'NONE',  ( -37.37352853689063892, -288.5519495502701943, -195.3611179825600175 ) ) ;
#69059 = CARTESIAN_POINT ( 'NONE',  ( -59.92426353831178432, -296.2447403286202530, -197.4175861963979628 ) ) ;
#69060 = CARTESIAN_POINT ( 'NONE',  ( 38.69760079047769352, -291.7916543487301055, -270.3330041864758755 ) ) ;
#69061 = CARTESIAN_POINT ( 'NONE',  ( -34.85540876630292217, -293.5092700483970134, -196.8138999951133599 ) ) ;
#69062 = CARTESIAN_POINT ( 'NONE',  ( 209.7513585654922679, 305.7026273589066818, 13.99999999999999112 ) ) ;
#69063 = CARTESIAN_POINT ( 'NONE',  ( -41.61246328981560794, -292.7999642431800567, -197.2744426717202941 ) ) ;
#69064 = CARTESIAN_POINT ( 'NONE',  ( 160.5350683151633291, 275.5000000000000568, 20.22542485937379908 ) ) ;
#69066 = CARTESIAN_POINT ( 'NONE',  ( -61.01316628223349880, -295.3680104789256688, -339.4701896549527760 ) ) ;
#69065 = CARTESIAN_POINT ( 'NONE',  ( -80.63759168149073275, -281.6557728833422516, -332.1001550752932303 ) ) ;
#69067 = CARTESIAN_POINT ( 'NONE',  ( -33.05874685161818860, -282.9996357027131353, -347.2550458299313050 ) ) ;
#69068 = CARTESIAN_POINT ( 'NONE',  ( -114.3338800259359829, -284.1878073109184584, -272.8443154304382574 ) ) ;
#69069 = EDGE_CURVE ( 'NONE', #4348, #66913, #33922, .T. ) ;
#69070 = CARTESIAN_POINT ( 'NONE',  ( -0.1006523332996065029, -286.5557158187147593, -335.3294033923898496 ) ) ;
#69071 = DIRECTION ( 'NONE',  ( 0.000000000000000000, -0.000000000000000000, 1.000000000000000000 ) ) ;
#69072 = CARTESIAN_POINT ( 'NONE',  ( 23.68882309526330232, -280.6472268829167547, -316.1648622569413192 ) ) ;
#69073 = CARTESIAN_POINT ( 'NONE',  ( 22.15658761977326208, -287.1245137316765295, -318.7702737150486314 ) ) ;
#69074 = LINE ( 'NONE', #74296, #3728 ) ;
#69075 = CARTESIAN_POINT ( 'NONE',  ( 8.743457688748675238, -296.0087700457601159, -328.0687969812492497 ) ) ;
#69076 = CARTESIAN_POINT ( 'NONE',  ( -39.92471464559405092, -278.5092423588239967, -346.7411867980971465 ) ) ;
#69077 = CARTESIAN_POINT ( 'NONE',  ( -9.235287070782970176, -280.0967488616905143, -202.9658879445917989 ) ) ;
#69078 = CARTESIAN_POINT ( 'NONE',  ( -36.38050047534928666, -292.2305704265120880, -193.3540852250272621 ) ) ;
#69079 = CARTESIAN_POINT ( 'NONE',  ( -31.76738481394369984, -281.0621908106563183, -345.7282432126794447 ) ) ;
#69080 = CARTESIAN_POINT ( 'NONE',  ( 23.12049151693259219, -293.1851431141279249, -311.7744914200487756 ) ) ;
#69081 = CARTESIAN_POINT ( 'NONE',  ( -104.7054917506405332, -294.9866993951073937, -237.3896117407235806 ) ) ;
#69082 = ORIENTED_EDGE ( 'NONE', *, *, #41751, .T. ) ;
#69083 = CARTESIAN_POINT ( 'NONE',  ( 132.9888089158688445, -299.5541904835127980, -188.7117359724263679 ) ) ;
#69084 = CARTESIAN_POINT ( 'NONE',  ( 12.39217848628290497, -293.8448432859474906, -323.9517551571413492 ) ) ;
#69085 = CARTESIAN_POINT ( 'NONE',  ( 208.4306832106271088, 0.04196010845015910040, -7.500000000000013323 ) ) ;
#69086 = CARTESIAN_POINT ( 'NONE',  ( 27.33386217378598815, -285.4809262143061801, -301.5434626090942629 ) ) ;
#69087 = CARTESIAN_POINT ( 'NONE',  ( -96.80459177145193905, -272.4042928292710144, -221.6751666727004988 ) ) ;
#69088 = CARTESIAN_POINT ( 'NONE',  ( 22.78181160526299109, -279.0665462617046728, -224.2371088011632878 ) ) ;
#69089 = EDGE_CURVE ( 'NONE', #51410, #30930, #47000, .T. ) ;
#69090 = EDGE_CURVE ( 'NONE', #17873, #59473, #71733, .T. ) ;
#69091 = CARTESIAN_POINT ( 'NONE',  ( -18.32092974086830495, -287.6073113321486403, -196.2016579321515053 ) ) ;
#69092 = CARTESIAN_POINT ( 'NONE',  ( -63.82287437146379006, -289.2404807025203013, -338.4428526538401343 ) ) ;
#69093 = CARTESIAN_POINT ( 'NONE',  ( -51.39431815137975690, -278.7552430099216281, -342.7021967504224449 ) ) ;
#69094 = CARTESIAN_POINT ( 'NONE',  ( -69.72080305854845506, -299.3799733593133396, -203.8061203483416080 ) ) ;
#69095 = CARTESIAN_POINT ( 'NONE',  ( -93.92188349220010934, -276.6877070892334700, -317.1334981513923026 ) ) ;
#69096 = EDGE_LOOP ( 'NONE', ( #85442, #40514, #19877, #84931 ) ) ;
#69097 = CARTESIAN_POINT ( 'NONE',  ( -51.79248209061327657, -297.5389691031875827, -194.6964827588738842 ) ) ;
#69098 = CARTESIAN_POINT ( 'NONE',  ( -108.7840730191190204, -292.7441415099378332, -249.4040483788558049 ) ) ;
#69099 = CARTESIAN_POINT ( 'NONE',  ( 34.73641292525844193, -295.4689581511520942, -295.2451178575328754 ) ) ;
#69100 = CARTESIAN_POINT ( 'NONE',  ( -23.68628624284178130, -55.96374926131388605, 21.50000000000000000 ) ) ;
#69101 = CARTESIAN_POINT ( 'NONE',  ( -71.21263066397611396, -290.1630777622050346, -335.1568366519673532 ) ) ;
#69102 = CARTESIAN_POINT ( 'NONE',  ( -43.48177207501702668, -254.5922926149944487, -445.2556498803733120 ) ) ;
#69103 = VERTEX_POINT ( 'NONE', #31888 ) ;
#69104 = CARTESIAN_POINT ( 'NONE',  ( -109.7576627626421413, -297.5305448026135764, -244.4914225431175794 ) ) ;
#69105 = CARTESIAN_POINT ( 'NONE',  ( -93.77518860890138797, -289.3887018914161899, -219.8085032185672958 ) ) ;
#69106 = CARTESIAN_POINT ( 'NONE',  ( -85.20658848613682324, -297.7446641055990995, -210.0726717104436716 ) ) ;
#69107 = CARTESIAN_POINT ( 'NONE',  ( 197.2964169323986425, 25.88250311104176049, 12.12231587770837393 ) ) ;
#69108 = CARTESIAN_POINT ( 'NONE',  ( 195.6164516548605548, 25.75475877429676785, 14.47166412665907842 ) ) ;
#69109 = CARTESIAN_POINT ( 'NONE',  ( -96.93434827407746468, -292.7164318225183024, -222.7016588705756419 ) ) ;
#69110 = CARTESIAN_POINT ( 'NONE',  ( -55.56934967048406548, -291.7662352645559167, -350.3683826091709648 ) ) ;
#69111 = CARTESIAN_POINT ( 'NONE',  ( -107.8938622612846956, -286.2266261901499433, -295.4636370617670877 ) ) ;
#69112 = CARTESIAN_POINT ( 'NONE',  ( 22.97358053910587472, -272.9466195794827286, -226.0655725294749629 ) ) ;
#69113 = CARTESIAN_POINT ( 'NONE',  ( -99.05035829400321745, -275.0408417615836925, -228.6355270060332145 ) ) ;
#69114 = CARTESIAN_POINT ( 'NONE',  ( -106.4590179936268157, -288.2675733135411065, -298.1421274133592192 ) ) ;
#69115 = CARTESIAN_POINT ( 'NONE',  ( -107.5035164782560742, -280.0434765697297053, -298.9552608214577845 ) ) ;
#69117 = CARTESIAN_POINT ( 'NONE',  ( 17.14431727601325761, -280.2044743842694174, -221.6254372569278246 ) ) ;
#69116 = CARTESIAN_POINT ( 'NONE',  ( -35.66279932563350030, -280.0737646465173043, -197.3680239662895701 ) ) ;
#69118 = CARTESIAN_POINT ( 'NONE',  ( 35.77210784752028871, -276.9239420079633192, -293.5098456583690449 ) ) ;
#69119 = CARTESIAN_POINT ( 'NONE',  ( 12.74419818758856060, -279.5279127641941272, -212.4006874507052203 ) ) ;
#69120 = CARTESIAN_POINT ( 'NONE',  ( 187.5249191740372225, 269.5786286523873514, -137.8896985354353149 ) ) ;
#69121 = CARTESIAN_POINT ( 'NONE',  ( 2.286242977736494986, -275.5106964986985645, -204.6158037921495350 ) ) ;
#69122 = PRODUCT_CONTEXT ( 'NONE', #89796, 'mechanical' ) ;
#69123 = CARTESIAN_POINT ( 'NONE',  ( 0.8316525005456222308, -276.0717705733681555, -204.2740200279934299 ) ) ;
#69124 = CARTESIAN_POINT ( 'NONE',  ( -37.37352853689063892, -300.5519495502701943, -195.3611179825600175 ) ) ;
#69125 = ORIENTED_EDGE ( 'NONE', *, *, #38392, .T. ) ;
#69126 = CYLINDRICAL_SURFACE ( 'NONE', #57473, 0.5000000000000004441 ) ;
#69127 = CARTESIAN_POINT ( 'NONE',  ( 31.69510081755798936, -288.9587866717197926, -295.0217381787643376 ) ) ;
#69128 = CARTESIAN_POINT ( 'NONE',  ( 30.78892748424178905, -289.7517901133387568, -304.1279118552374143 ) ) ;
#69129 = CARTESIAN_POINT ( 'NONE',  ( -92.49408472459907671, -289.2169206684125697, -318.4170538630988290 ) ) ;
#69130 = CARTESIAN_POINT ( 'NONE',  ( -0.9930908772130121465, -286.0291765328881866, -202.5503112560963359 ) ) ;
#69131 = CARTESIAN_POINT ( 'NONE',  ( 199.5806965732583933, 26.46139589673911985, 10.63455718553152352 ) ) ;
#69132 = CARTESIAN_POINT ( 'NONE',  ( 19.09309330472423838, -280.6204841067794860, -317.9365322202862671 ) ) ;
#69133 = CARTESIAN_POINT ( 'NONE',  ( -2.770378220405110170, -290.4508535341478819, -336.1119664927302324 ) ) ;
#69134 = CARTESIAN_POINT ( 'NONE',  ( -81.05280504165224897, -282.1375520136339219, -329.7546028229263015 ) ) ;
#69135 = CARTESIAN_POINT ( 'NONE',  ( -106.9169831515794158, -280.1816977288369799, -246.5293538906025503 ) ) ;
#69136 = CARTESIAN_POINT ( 'NONE',  ( -78.66164416873338894, -278.1174831519164172, -330.6775999518185358 ) ) ;
#69137 = CARTESIAN_POINT ( 'NONE',  ( -96.99060916388398823, -288.6992586151886826, -318.4444385517433602 ) ) ;
#69138 = CARTESIAN_POINT ( 'NONE',  ( -114.1656263199322439, -285.3954601322072904, -267.1314136815969960 ) ) ;
#69139 = CARTESIAN_POINT ( 'NONE',  ( -87.71438949609948565, -285.8630994426134748, -212.1345925866928610 ) ) ;
#69140 = CARTESIAN_POINT ( 'NONE',  ( -2.426796353345956891, -282.7432800014123586, -334.4842952976615038 ) ) ;
#69141 = VERTEX_POINT ( 'NONE', #70577 ) ;
#69142 = DIRECTION ( 'NONE',  ( 1.000000000000000000, -0.000000000000000000, 0.000000000000000000 ) ) ;
#69143 = CARTESIAN_POINT ( 'NONE',  ( -100.6648485274051126, -292.9693778453632831, -228.6678392213815698 ) ) ;
#69144 = CARTESIAN_POINT ( 'NONE',  ( -16.74318851087497961, -290.9976653230809802, -196.6793726809117970 ) ) ;
#69145 = CARTESIAN_POINT ( 'NONE',  ( -1.597347459022061766, -273.5970631480266775, -206.4268879460287280 ) ) ;
#69146 = CARTESIAN_POINT ( 'NONE',  ( -47.62616119627649880, -294.5282284634277516, -346.5683528550601977 ) ) ;
#69147 = CARTESIAN_POINT ( 'NONE',  ( -91.25332714646035015, -289.7478700355291039, -220.1006087151738200 ) ) ;
#69148 = CARTESIAN_POINT ( 'NONE',  ( 6.647455419184660208, -292.6850485722981148, -329.9474766471125236 ) ) ;
#69149 = CARTESIAN_POINT ( 'NONE',  ( -66.47258166540430580, -290.6472966164407126, -337.7839770994312403 ) ) ;
#69150 = DIRECTION ( 'NONE',  ( -0.000000000000000000, -1.000000000000000000, -0.000000000000000000 ) ) ;
#69151 = CARTESIAN_POINT ( 'NONE',  ( -108.5405455545936064, -292.8588280645182067, -246.6246022097248272 ) ) ;
#69152 = CARTESIAN_POINT ( 'NONE',  ( 19.93051215466206116, -290.8794933480363056, -221.6595997707165111 ) ) ;
#69153 = CARTESIAN_POINT ( 'NONE',  ( 32.25513783405078527, -295.9180969805728978, -298.4493555469398416 ) ) ;
#69154 = CARTESIAN_POINT ( 'NONE',  ( 23.72365130486163309, -287.9331878888522169, -229.8412257977494164 ) ) ;
#69155 = CARTESIAN_POINT ( 'NONE',  ( -0.8642176097822394931, -276.5138609750960086, -204.4085972454281830 ) ) ;
#69156 = CARTESIAN_POINT ( 'NONE',  ( -67.56613687916350841, -276.2348973475908451, -340.7492714063686208 ) ) ;
#69157 = ADVANCED_FACE ( 'NONE', ( #3002 ), #61710, .F. ) ;
#69158 = CARTESIAN_POINT ( 'NONE',  ( -36.17713848653617958, -297.2635566339611728, -193.5227470404294081 ) ) ;
#69159 = CARTESIAN_POINT ( 'NONE',  ( 26.23471270372015596, -274.3058924017101958, -308.2558899628895688 ) ) ;
#69160 = CARTESIAN_POINT ( 'NONE',  ( 1.165382885659398182, -278.6499945637035580, -206.5949340252136892 ) ) ;
#69161 = CARTESIAN_POINT ( 'NONE',  ( -48.95330406819405766, -275.1061581843280806, -197.8369035123738513 ) ) ;
#69162 = CARTESIAN_POINT ( 'NONE',  ( -1.858511850691574985, -274.9899250483807691, -337.7954101990465006 ) ) ;
#69163 = CYLINDRICAL_SURFACE ( 'NONE', #45939, 5.999999999999998224 ) ;
#69164 = CARTESIAN_POINT ( 'NONE',  ( -103.3006124605445564, -273.6292065093160772, -238.8442248656458275 ) ) ;
#69165 = DIRECTION ( 'NONE',  ( -0.9531768234073174639, 0.3024135303175699563, -3.864692125754213305E-13 ) ) ;
#69167 = CARTESIAN_POINT ( 'NONE',  ( 25.27692151142132104, -274.8681822947537512, -232.7410999281489694 ) ) ;
#69166 = CARTESIAN_POINT ( 'NONE',  ( 13.47550346692731260, -286.3655769213731901, -326.0736839936324145 ) ) ;
#69168 = CARTESIAN_POINT ( 'NONE',  ( 39.64005161437589209, -287.5311880329594487, -268.6848427477963810 ) ) ;
#69169 = CARTESIAN_POINT ( 'NONE',  ( -46.02760227429062923, -288.8260273098534867, -346.9014801462115543 ) ) ;
#69170 = CARTESIAN_POINT ( 'NONE',  ( -35.89361067862525090, -300.0500808513247648, -195.0054237258406999 ) ) ;
#69171 = CARTESIAN_POINT ( 'NONE',  ( -35.63367922416287570, -293.0305454694981790, -345.1877711499467978 ) ) ;
#69172 = CARTESIAN_POINT ( 'NONE',  ( 36.44751926472988401, -280.4794686023626582, -248.8824091577034778 ) ) ;
#69173 = DIRECTION ( 'NONE',  ( -1.000000000000000000, -0.000000000000000000, -0.000000000000000000 ) ) ;
#69174 = CARTESIAN_POINT ( 'NONE',  ( -99.57556123191122310, -277.1183276717264903, -228.4820149166808676 ) ) ;
#69175 = DIRECTION ( 'NONE',  ( -0.000000000000000000, -1.000000000000000000, -0.000000000000000000 ) ) ;
#69176 = CARTESIAN_POINT ( 'NONE',  ( -87.00930905645846281, -288.5567837569653307, -324.4695016943931591 ) ) ;
#69177 = CARTESIAN_POINT ( 'NONE',  ( 157.4851178187871312, 17.34719063663031946, 6.999999999999999112 ) ) ;
#69178 = CARTESIAN_POINT ( 'NONE',  ( 175.2296996224750103, 215.0000000000000568, 0.000000000000000000 ) ) ;
#69179 = CARTESIAN_POINT ( 'NONE',  ( -110.0410055481184060, -288.7894100584843500, -251.8749775035765026 ) ) ;
#69180 = CARTESIAN_POINT ( 'NONE',  ( -3.806295163463269127, -276.0229930234823996, -204.7261916807048578 ) ) ;
#69181 = CARTESIAN_POINT ( 'NONE',  ( 37.09930863393419997, -282.7595183661034071, -253.0658691171516068 ) ) ;
#69183 = CARTESIAN_POINT ( 'NONE',  ( -108.7200628095166763, -284.3495196044772797, -285.7217736511791486 ) ) ;
#69182 = CARTESIAN_POINT ( 'NONE',  ( -108.7331577904153335, -270.9499913748800282, -245.6108862693309334 ) ) ;
#69184 = CARTESIAN_POINT ( 'NONE',  ( -64.80540891476478293, -275.1116061424378927, -202.0751348932619464 ) ) ;
#69185 = CARTESIAN_POINT ( 'NONE',  ( -16.60466231704504025, -275.1297316148242658, -200.1472167058889227 ) ) ;
#69186 = CARTESIAN_POINT ( 'NONE',  ( 8.019941878355446363, -284.4322384319294770, -330.0881811967416866 ) ) ;
#69187 = CARTESIAN_POINT ( 'NONE',  ( -36.46788982174913940, -297.1221009679233021, -197.1259658601755973 ) ) ;
#69188 = ORIENTED_EDGE ( 'NONE', *, *, #30297, .T. ) ;
#69189 = DIRECTION ( 'NONE',  ( -0.000000000000000000, -0.000000000000000000, -1.000000000000000000 ) ) ;
#69190 = CARTESIAN_POINT ( 'NONE',  ( 13.39423242910156553, -294.1987229847631511, -328.3530086978565805 ) ) ;
#69191 = CARTESIAN_POINT ( 'NONE',  ( -65.74186254280407127, -287.6588843635568651, -201.2750983082859761 ) ) ;
#69192 = DIRECTION ( 'NONE',  ( 0.000000000000000000, 1.000000000000000000, 0.000000000000000000 ) ) ;
#69193 = CARTESIAN_POINT ( 'NONE',  ( -55.56934967048407970, -277.3380690714490129, -190.3538533559490702 ) ) ;
#69194 = CARTESIAN_POINT ( 'NONE',  ( -104.8386282014230630, -277.2731590543393736, -307.0806430435176253 ) ) ;
#69195 = ADVANCED_FACE ( 'NONE', ( #39425 ), #3468, .T. ) ;
#69196 = CARTESIAN_POINT ( 'NONE',  ( -101.6373126356855181, -288.4092470070361856, -311.3546454658352332 ) ) ;
#69197 = CARTESIAN_POINT ( 'NONE',  ( -29.35040928699174501, -284.4693565499903798, -343.6708692461893975 ) ) ;
#69198 = CARTESIAN_POINT ( 'NONE',  ( -104.0345266862015734, -279.8826139311257748, -302.5738828140925420 ) ) ;
#69199 = CARTESIAN_POINT ( 'NONE',  ( -80.61953699863192924, -286.9034660038551579, -207.3239533732535733 ) ) ;
#69200 = CARTESIAN_POINT ( 'NONE',  ( -8.501176363250989354, -282.4298136080363975, -201.1279984562739003 ) ) ;
#69201 = CARTESIAN_POINT ( 'NONE',  ( -1.303373629501783704, -274.6834726146394701, -202.3152582429418942 ) ) ;
#69202 = CARTESIAN_POINT ( 'NONE',  ( -72.84257142225602877, -277.3425458995909594, -338.7036210802558003 ) ) ;
#69203 = CARTESIAN_POINT ( 'NONE',  ( -56.14386852559702135, -297.2162425734469480, -342.4408625498203378 ) ) ;
#69204 = FACE_OUTER_BOUND ( 'NONE', #36117, .T. ) ;
#69205 = CARTESIAN_POINT ( 'NONE',  ( 185.7024372569428294, 214.9312412210030061, 22.95886720168237005 ) ) ;
#69206 = CARTESIAN_POINT ( 'NONE',  ( -40.36682480728010347, -296.1542282064546043, -194.6054403054197621 ) ) ;
#69207 = CARTESIAN_POINT ( 'NONE',  ( 9.698888311416199670, -275.8916021848230002, -326.2643511692858738 ) ) ;
#69208 = CARTESIAN_POINT ( 'NONE',  ( -80.46262503497078455, -298.5626496516304655, -206.8774031763040284 ) ) ;
#69209 = CARTESIAN_POINT ( 'NONE',  ( 34.00013390127604396, -289.0554681077743453, -250.6553641942012121 ) ) ;
#69210 = CARTESIAN_POINT ( 'NONE',  ( -112.4600240174401904, -298.2415588462148435, -256.9467536749043575 ) ) ;
#69211 = CARTESIAN_POINT ( 'NONE',  ( -113.2569836957410843, -297.6236061545674829, -280.9900518570369741 ) ) ;
#69212 = CARTESIAN_POINT ( 'NONE',  ( -78.27884800997664172, -293.5002010137922639, -207.7178553907379523 ) ) ;
#69213 = CARTESIAN_POINT ( 'NONE',  ( -97.87405260181819244, -277.1527077894652393, -226.3626778668180464 ) ) ;
#69214 = CARTESIAN_POINT ( 'NONE',  ( -110.5526814306512620, -280.6465741234623010, -256.8901708507413559 ) ) ;
#69215 = CARTESIAN_POINT ( 'NONE',  ( -71.09913707219612888, -295.6829560375836650, -204.0012508289246398 ) ) ;
#69216 = CARTESIAN_POINT ( 'NONE',  ( -67.36966247387626083, -285.3022068839415510, -339.9213577737837682 ) ) ;
#69217 = CARTESIAN_POINT ( 'NONE',  ( 13.36324082226746413, -285.7018724636245111, -217.3454837400828126 ) ) ;
#69218 = CARTESIAN_POINT ( 'NONE',  ( 123.2264321157264391, 148.5360561407864850, -263.2575006249301168 ) ) ;
#69219 = ORIENTED_EDGE ( 'NONE', *, *, #28532, .T. ) ;
#69220 = CARTESIAN_POINT ( 'NONE',  ( 35.14469227722530320, -287.3351994146748893, -279.1821384915217550 ) ) ;
#69221 = ORIENTED_EDGE ( 'NONE', *, *, #12664, .T. ) ;
#69222 = CARTESIAN_POINT ( 'NONE',  ( -1.765278710261730666, -283.6715999781039272, -338.3008762224394559 ) ) ;
#69223 = CARTESIAN_POINT ( 'NONE',  ( -97.86309523353898498, -273.4542249049417819, -229.4144698171547816 ) ) ;
#69224 = CARTESIAN_POINT ( 'NONE',  ( 23.55516425774165157, -285.7240790668212753, -223.8683178387225610 ) ) ;
#69225 = CARTESIAN_POINT ( 'NONE',  ( -1.256671603243712410, -281.4602309328722072, -202.6064802828197742 ) ) ;
#69226 = LINE ( 'NONE', #11460, #83945 ) ;
#69227 = CARTESIAN_POINT ( 'NONE',  ( -19.93338039395358052, -281.7919569134650715, -196.0124422787080505 ) ) ;
#69228 = CARTESIAN_POINT ( 'NONE',  ( -2.403531427808004661, -280.8348773736983617, -201.7528916542626121 ) ) ;
#69229 = CARTESIAN_POINT ( 'NONE',  ( -82.08285599513421005, -282.9094976428776249, -214.2051214447836571 ) ) ;
#69230 = CARTESIAN_POINT ( 'NONE',  ( 103.8745525416007496, 116.1007460503243607, -283.0288680581506355 ) ) ;
#69231 = ORIENTED_EDGE ( 'NONE', *, *, #87554, .T. ) ;
#69232 = CARTESIAN_POINT ( 'NONE',  ( -54.65992989471284602, -275.8292287715964903, -197.5592818716456520 ) ) ;
#69233 = CARTESIAN_POINT ( 'NONE',  ( -110.6039295111287544, -266.3419550533109259, -306.8688986251918323 ) ) ;
#69234 = CARTESIAN_POINT ( 'NONE',  ( 28.28952166637291654, -280.0467606568328733, -305.9193733629799112 ) ) ;
#69235 = CARTESIAN_POINT ( 'NONE',  ( 37.81759593152978027, -295.4540113672994721, -281.5438828316768536 ) ) ;
#69236 = CARTESIAN_POINT ( 'NONE',  ( -26.20004334799273948, -294.2551394079507645, -342.6089978970040306 ) ) ;
#69237 = CARTESIAN_POINT ( 'NONE',  ( -22.19975866122103980, -291.7486162255135582, -194.8730986231747124 ) ) ;
#69238 = DIRECTION ( 'NONE',  ( 0.000000000000000000, 0.000000000000000000, 1.000000000000000000 ) ) ;
#69240 = CARTESIAN_POINT ( 'NONE',  ( 18.41671371781579580, -286.6342838432111648, -318.7846799880942399 ) ) ;
#69239 = CARTESIAN_POINT ( 'NONE',  ( -92.28602029857157163, -294.3938677875706844, -323.4622288322950112 ) ) ;
#69241 = CARTESIAN_POINT ( 'NONE',  ( 35.15096508368568351, -295.2043822410277016, -254.3124578910395712 ) ) ;
#69242 = CARTESIAN_POINT ( 'NONE',  ( 36.12217363706486850, -286.2820244621223083, -273.7994906670598994 ) ) ;
#69243 = CARTESIAN_POINT ( 'NONE',  ( -95.35659980119862666, -286.4989386854391000, -225.2239969332456440 ) ) ;
#69244 = ORIENTED_EDGE ( 'NONE', *, *, #82386, .T. ) ;
#69245 = CARTESIAN_POINT ( 'NONE',  ( 35.22624047049254870, -294.1750489317341248, -245.1660271171927548 ) ) ;
#69246 = CARTESIAN_POINT ( 'NONE',  ( 32.29188160470507540, -282.3394509740934382, -292.6427317032751603 ) ) ;
#69247 = CARTESIAN_POINT ( 'NONE',  ( -113.7235956879930399, -295.4284451834167839, -263.8886521477987799 ) ) ;
#69248 = CARTESIAN_POINT ( 'NONE',  ( -113.0147736945237966, -291.5220680507783300, -257.0290229574998762 ) ) ;
#69249 = CARTESIAN_POINT ( 'NONE',  ( -73.41041876034066149, -292.0791478858488972, -202.3861351202400272 ) ) ;
#69250 = CARTESIAN_POINT ( 'NONE',  ( -10.72212113880805617, -288.8618850755676135, -338.3888442385951976 ) ) ;
#69251 = ORIENTED_EDGE ( 'NONE', *, *, #19481, .T. ) ;
#69252 = LINE ( 'NONE', #84837, #45790 ) ;
#69253 = CARTESIAN_POINT ( 'NONE',  ( -92.76940719763844356, -297.6967338247578141, -322.0336289705962258 ) ) ;
#69254 = CARTESIAN_POINT ( 'NONE',  ( 52.88111462291031017, -297.8442732174480057, -193.8739110169187541 ) ) ;
#69255 = CARTESIAN_POINT ( 'NONE',  ( 25.34387178002038610, -280.0901798291656633, -232.3955815017435782 ) ) ;
#69256 = VERTEX_POINT ( 'NONE', #38967 ) ;
#69257 = CARTESIAN_POINT ( 'NONE',  ( 30.48585073910440713, -275.5308438472565626, -306.7909476733175893 ) ) ;
#69258 = CARTESIAN_POINT ( 'NONE',  ( -58.08154585589248597, -296.2591376933737592, -199.6464338632072781 ) ) ;
#69259 = CARTESIAN_POINT ( 'NONE',  ( -29.56079077309719239, -278.8131378396576565, -344.2391887151030119 ) ) ;
#69260 = CARTESIAN_POINT ( 'NONE',  ( 10.29556459549709224, -272.8566925253235809, -213.3591157503087459 ) ) ;
#69261 = CARTESIAN_POINT ( 'NONE',  ( -58.50816103026473769, -296.5370856815455340, -340.6399301298143882 ) ) ;
#69262 = CARTESIAN_POINT ( 'NONE',  ( -55.38298001842601792, -298.8943441392891600, -199.2541089461053332 ) ) ;
#69263 = CARTESIAN_POINT ( 'NONE',  ( 197.2116943569230045, 250.0000000000000568, -12.92446933126075592 ) ) ;
#69264 = CARTESIAN_POINT ( 'NONE',  ( -108.6813058152199432, -297.8082822354275550, -297.2886207814248110 ) ) ;
#69265 = CARTESIAN_POINT ( 'NONE',  ( -110.2208797385357286, -270.8196446865079565, -251.0035832070425386 ) ) ;
#69266 = CARTESIAN_POINT ( 'NONE',  ( -38.90806881155080532, -292.6834012793393640, -197.2759679337297314 ) ) ;
#69267 = CARTESIAN_POINT ( 'NONE',  ( -107.5584459396347370, -289.4169141798775513, -248.2963610346981227 ) ) ;
#69268 = CARTESIAN_POINT ( 'NONE',  ( 208.7500163748177897, 30.13141828311449189, 14.27675564571656253 ) ) ;
#69269 = CARTESIAN_POINT ( 'NONE',  ( -21.37368610867320484, -274.7440150958080380, -195.0979169389452466 ) ) ;
#69270 = CARTESIAN_POINT ( 'NONE',  ( -81.07270386167502352, -273.6062286352672004, -211.8460037010188728 ) ) ;
#69271 = CARTESIAN_POINT ( 'NONE',  ( 24.90734321336867296, -282.9586211390911785, -227.8029091420009706 ) ) ;
#69272 = CARTESIAN_POINT ( 'NONE',  ( -16.29369088238053465, -281.4705758751784401, -343.9706484194546192 ) ) ;
#69273 = CARTESIAN_POINT ( 'NONE',  ( -17.39234758856538221, -276.1498424671655698, -344.6264269736359438 ) ) ;
#69274 = CARTESIAN_POINT ( 'NONE',  ( -110.4704261979584032, -283.7781257015364531, -268.1722484470649874 ) ) ;
#69275 = CARTESIAN_POINT ( 'NONE',  ( 1.133315503967222249, -280.5395511377577122, -334.9343446210174307 ) ) ;
#69276 = CARTESIAN_POINT ( 'NONE',  ( 33.80727929939043719, -274.3730551417065726, -289.1546712620323092 ) ) ;
#69277 = CARTESIAN_POINT ( 'NONE',  ( -93.76812529164524790, -281.2391512508279448, -220.8778602240109592 ) ) ;
#69278 = CARTESIAN_POINT ( 'NONE',  ( -48.18343439339133027, -291.0521521680024080, -502.6442049081569508 ) ) ;
#69279 = DIRECTION ( 'NONE',  ( 0.000000000000000000, 0.000000000000000000, 1.000000000000000000 ) ) ;
#69280 = CARTESIAN_POINT ( 'NONE',  ( -34.07830763726472867, -296.3323406979883998, -194.3754068573094003 ) ) ;
#69281 = CARTESIAN_POINT ( 'NONE',  ( -105.8933992100000410, -280.1474408776773544, -301.3209834162412903 ) ) ;
#69282 = DIRECTION ( 'NONE',  ( -0.000000000000000000, -1.000000000000000000, -0.000000000000000000 ) ) ;
#69283 = CARTESIAN_POINT ( 'NONE',  ( -64.70742701758980786, -285.3268371164436985, -340.8053827262196478 ) ) ;
#69284 = VERTEX_POINT ( 'NONE', #18146 ) ;
#69285 = CARTESIAN_POINT ( 'NONE',  ( 156.3984609948128366, 15.95758591462681864, -7.138650918358526276 ) ) ;
#69286 = CARTESIAN_POINT ( 'NONE',  ( 25.19340208255916380, -286.1122329376198650, -311.8584847024332021 ) ) ;
#69287 = CARTESIAN_POINT ( 'NONE',  ( 156.8041522122653930, 275.5000000000000568, 16.89672165344857646 ) ) ;
#69288 = CARTESIAN_POINT ( 'NONE',  ( -72.32728988598383069, -294.3208725906686709, -334.8978575460146772 ) ) ;
#69289 = CARTESIAN_POINT ( 'NONE',  ( -64.29103499604589445, -287.5470180804531992, -339.5870223161121544 ) ) ;
#69290 = CARTESIAN_POINT ( 'NONE',  ( 157.2528655986806427, 19.19772955881777676, -10.67418916507680748 ) ) ;
#69291 = CARTESIAN_POINT ( 'NONE',  ( -93.32116580629005398, -295.2467577490175472, -220.4481930762391642 ) ) ;
#69292 = CARTESIAN_POINT ( 'NONE',  ( -75.74092574302582648, -284.0296335504341982, -204.3593413916691190 ) ) ;
#69293 = CARTESIAN_POINT ( 'NONE',  ( -4.004221230905659290, -282.0994657437091178, -204.5059574697724543 ) ) ;
#69294 = CARTESIAN_POINT ( 'NONE',  ( 33.38950778090992344, -279.4336669247442728, -242.4492455671945663 ) ) ;
#69295 = CARTESIAN_POINT ( 'NONE',  ( -45.36244843969432594, -289.1566037294502394, -342.9191471490262302 ) ) ;
#69296 = CARTESIAN_POINT ( 'NONE',  ( -68.79144662499599860, -281.0556376148206823, -203.8307612698487503 ) ) ;
#69297 = CARTESIAN_POINT ( 'NONE',  ( -74.59680201176173853, -280.3459612062362680, -207.3373447454603138 ) ) ;
#69298 = ADVANCED_FACE ( 'NONE', ( #75903 ), #41462, .F. ) ;
#69299 = CARTESIAN_POINT ( 'NONE',  ( 35.55971737992850734, -289.7759980750545310, -289.4344011550113578 ) ) ;
#69300 = VERTEX_POINT ( 'NONE', #31431 ) ;
#69301 = CARTESIAN_POINT ( 'NONE',  ( -76.43272161342319748, -273.5448347711234192, -203.9602894325051921 ) ) ;
#69302 = CARTESIAN_POINT ( 'NONE',  ( -95.36732255047787987, -291.8824715678344432, -317.3172033120404762 ) ) ;
#69303 = CARTESIAN_POINT ( 'NONE',  ( 123.4306832106270946, -178.2391364535880882, 0.000000000000000000 ) ) ;
#69304 = CARTESIAN_POINT ( 'NONE',  ( 40.65961533371913106, -290.2662352645559167, -288.1317622949166548 ) ) ;
#69305 = ORIENTED_EDGE ( 'NONE', *, *, #13732, .F. ) ;
#69306 = CARTESIAN_POINT ( 'NONE',  ( 11.49372615785818574, -274.3764101298928608, -327.5024302101932108 ) ) ;
#69307 = CARTESIAN_POINT ( 'NONE',  ( 152.4536156746142410, 275.5000000000000568, 12.00000000000000000 ) ) ;
#69308 = CARTESIAN_POINT ( 'NONE',  ( -2.353145382731069546, -292.9968452683397118, -338.0533734794150291 ) ) ;
#69309 = CARTESIAN_POINT ( 'NONE',  ( -95.33409194151947474, -296.6846996281569773, -225.9012151161579709 ) ) ;
#69310 = CARTESIAN_POINT ( 'NONE',  ( -18.27563170611723820, -290.3222400462855717, -341.5984242092235377 ) ) ;
#69311 = CARTESIAN_POINT ( 'NONE',  ( -83.40815489732948151, -285.4532926610873460, -328.3566151343581510 ) ) ;
#69312 = CARTESIAN_POINT ( 'NONE',  ( -102.7211617983520000, -292.4987175454272119, -230.7099522497011606 ) ) ;
#69313 = CARTESIAN_POINT ( 'NONE',  ( -61.54852897498791719, -293.0594195068215413, -197.7289585370036207 ) ) ;
#69314 = CARTESIAN_POINT ( 'NONE',  ( -68.39850958073731135, -287.6443072045177587, -202.0934445279293925 ) ) ;
#69315 = CARTESIAN_POINT ( 'NONE',  ( -84.56860703283433622, -279.5889427892554977, -209.4773675643675404 ) ) ;
#69316 = CARTESIAN_POINT ( 'NONE',  ( -108.9882106666822068, -294.3240086637433137, -294.3630288440068057 ) ) ;
#69317 = CARTESIAN_POINT ( 'NONE',  ( -66.57821600046094090, -283.2579563819441546, -341.6089067039796419 ) ) ;
#69318 = CARTESIAN_POINT ( 'NONE',  ( -2.352044767130743175, -276.3807553175748808, -204.8890666943467807 ) ) ;
#69319 = ADVANCED_FACE ( 'NONE', ( #46540 ), #61261, .T. ) ;
#69320 = CARTESIAN_POINT ( 'NONE',  ( -92.05005921254146983, -280.4090924074130839, -314.0302885647153062 ) ) ;
#69321 = CARTESIAN_POINT ( 'NONE',  ( -84.12262183171560537, -275.8266463380884375, -330.0252037396156766 ) ) ;
#69322 = LINE ( 'NONE', #4921, #42426 ) ;
#69323 = CARTESIAN_POINT ( 'NONE',  ( 17.64704285392907934, -281.7456241592662991, -318.4675269843156116 ) ) ;
#69324 = CARTESIAN_POINT ( 'NONE',  ( -112.6723356732494921, -279.5815358763037466, -284.3364924590230203 ) ) ;
#69325 = CARTESIAN_POINT ( 'NONE',  ( -33.72638223235642130, -285.1553578358346499, -193.6815920980390331 ) ) ;
#69326 = CARTESIAN_POINT ( 'NONE',  ( -37.57534318073167867, -293.8093657382221409, -196.3355339494858924 ) ) ;
#69327 = CARTESIAN_POINT ( 'NONE',  ( 37.42977496804506643, -276.9666831397738065, -255.6755151940899395 ) ) ;
#69328 = CARTESIAN_POINT ( 'NONE',  ( 15.67317711600109043, -276.0990007206884229, -215.2002526639491293 ) ) ;
#69329 = CARTESIAN_POINT ( 'NONE',  ( 32.89727594926724663, -275.6489238994626021, -290.2936939179304545 ) ) ;
#69330 = CARTESIAN_POINT ( 'NONE',  ( -64.20388122450974322, -297.4034475819129852, -340.2619259435887216 ) ) ;
#69331 = CARTESIAN_POINT ( 'NONE',  ( -112.2251689236907310, -282.5450820954114874, -270.8976449407572886 ) ) ;
#69332 = CARTESIAN_POINT ( 'NONE',  ( -25.02064184023286231, -291.8719041091303552, -194.3746993663606588 ) ) ;
#69333 = CARTESIAN_POINT ( 'NONE',  ( 38.55586450579806268, -289.0594273390983631, -263.0139173236334500 ) ) ;
#69334 = CARTESIAN_POINT ( 'NONE',  ( 16.97643238134160626, -291.7693628098492127, -221.0548846136896373 ) ) ;
#69335 = ORIENTED_EDGE ( 'NONE', *, *, #72851, .T. ) ;
#69336 = CARTESIAN_POINT ( 'NONE',  ( 30.38513866485025261, -291.6656358304941818, -234.8680488545314518 ) ) ;
#69337 = CARTESIAN_POINT ( 'NONE',  ( -67.80614379073990960, -291.3076832542452053, -203.9847011862297563 ) ) ;
#69338 = EDGE_LOOP ( 'NONE', ( #16152, #11572, #85318, #60045 ) ) ;
#69339 = CARTESIAN_POINT ( 'NONE',  ( -59.92308945573012835, -290.4177618427382868, -343.6521362938286757 ) ) ;
#69340 = CARTESIAN_POINT ( 'NONE',  ( -109.6433618957493366, -279.0249137139012419, -259.7848067016466871 ) ) ;
#69341 = CARTESIAN_POINT ( 'NONE',  ( -102.8586806540441074, -294.9498851330534421, -310.2236037553919914 ) ) ;
#69342 = CARTESIAN_POINT ( 'NONE',  ( -93.85047565060217778, -285.9152642450737289, -218.1287687468918080 ) ) ;
#69343 = CARTESIAN_POINT ( 'NONE',  ( 12.06075724195058285, -287.0504729443960059, -211.2564775508933508 ) ) ;
#69345 = CARTESIAN_POINT ( 'NONE',  ( -108.9505344823494539, -285.0739155887426932, -256.0690807143886900 ) ) ;
#69344 = AXIS2_PLACEMENT_3D ( 'NONE', #65405, #57359, #29399 ) ;
#69346 = CARTESIAN_POINT ( 'NONE',  ( -84.39908107231754286, -219.2962774960428760, -352.3863144506401568 ) ) ;
#69347 = CARTESIAN_POINT ( 'NONE',  ( -49.37733225207519183, -154.2223004629079810, -363.8550686714801827 ) ) ;
#69348 = CARTESIAN_POINT ( 'NONE',  ( -83.36829938135619500, -218.4018712402734650, -348.9267425600256161 ) ) ;
#69349 = CARTESIAN_POINT ( 'NONE',  ( 35.18192278478999668, -274.6224313375963675, -260.7213126656877193 ) ) ;
#69350 = CARTESIAN_POINT ( 'NONE',  ( 31.54753624136908030, -274.8068624756293730, -295.5784400796692921 ) ) ;
#69351 = CARTESIAN_POINT ( 'NONE',  ( -68.14705418104928469, -297.1661347181519659, -199.8021905112523484 ) ) ;
#69352 = CARTESIAN_POINT ( 'NONE',  ( -11.27636105762056218, -93.00928234723599530, -356.9605620023007759 ) ) ;
#69353 = CARTESIAN_POINT ( 'NONE',  ( 24.93528355352991355, -273.6443032015265544, -225.8991278562868104 ) ) ;
#69354 = CARTESIAN_POINT ( 'NONE',  ( -89.97836760152866020, -275.0560971070458436, -218.3288659641350193 ) ) ;
#69355 = CARTESIAN_POINT ( 'NONE',  ( 53.23043170612119468, -300.1013752903952536, -193.5822955068719580 ) ) ;
#69356 = CARTESIAN_POINT ( 'NONE',  ( 33.14294324827755389, -288.3006089749009675, -289.7817941462497515 ) ) ;
#69357 = CARTESIAN_POINT ( 'NONE',  ( -47.59987637687407158, -295.9822399706359874, -346.5118148947088343 ) ) ;
#69358 = CARTESIAN_POINT ( 'NONE',  ( -43.29125860421211058, -298.4714041380003664, -193.5998693973546665 ) ) ;
#69359 = CARTESIAN_POINT ( 'NONE',  ( -36.99341668510393788, -295.2143193158671579, -343.3727113808294007 ) ) ;
#69360 = ORIENTED_EDGE ( 'NONE', *, *, #87626, .T. ) ;
#69361 = CARTESIAN_POINT ( 'NONE',  ( 12.98676805008828516, -276.6682520112348698, -213.9320191820249306 ) ) ;
#69362 = ORIENTED_EDGE ( 'NONE', *, *, #7047, .F. ) ;
#69363 = CARTESIAN_POINT ( 'NONE',  ( -62.02194941492411573, -279.2474761315834257, -197.4323570711135574 ) ) ;
#69364 = UNCERTAINTY_MEASURE_WITH_UNIT (LENGTH_MEASURE( 1.000000000000000082E-05 ), #13813, 'distance_accuracy_value', 'NONE');
#69365 = CARTESIAN_POINT ( 'NONE',  ( -59.25401880934609977, -278.2841331671683065, -340.2414352233124646 ) ) ;
#69366 = CARTESIAN_POINT ( 'NONE',  ( 16.25656700619970607, -278.0645506452200379, -324.2974006643162852 ) ) ;
#69367 = CARTESIAN_POINT ( 'NONE',  ( -112.5673809534716412, -276.6286952785854965, -265.9448135772202590 ) ) ;
#69368 = CARTESIAN_POINT ( 'NONE',  ( -31.34090078994525186, -274.6222994094842988, -197.5337693306901201 ) ) ;
#69369 = CARTESIAN_POINT ( 'NONE',  ( -95.24824955063338905, -294.4916823707704907, -315.7726413329684760 ) ) ;
#69370 = DIRECTION ( 'NONE',  ( -0.3994899938748465162, 0.000000000000000000, -0.9167375550253601402 ) ) ;
#69371 = CARTESIAN_POINT ( 'NONE',  ( -92.72525199358497616, -278.0417474314594983, -317.9180542514714034 ) ) ;
#69372 = CARTESIAN_POINT ( 'NONE',  ( 20.19092575943044565, -286.9238835169735466, -320.8119428413362471 ) ) ;
#69373 = CARTESIAN_POINT ( 'NONE',  ( -91.73956980718394050, -275.2768696529319072, -218.7102821747882331 ) ) ;
#69374 = PLANE ( 'NONE',  #24795 ) ;
#69375 = CARTESIAN_POINT ( 'NONE',  ( -109.7842798137740061, -289.6134650260669900, -280.6821334575872129 ) ) ;
#69376 = CARTESIAN_POINT ( 'NONE',  ( -93.36297077219080620, -283.1806396571025175, -323.0580291428240685 ) ) ;
#69377 = CARTESIAN_POINT ( 'NONE',  ( 34.29878201119488068, -280.0346712132531479, -289.0022723677582803 ) ) ;
#69379 = CARTESIAN_POINT ( 'NONE',  ( -110.8390699916720337, -282.7858038708150161, -258.4716102760308445 ) ) ;
#69378 = CARTESIAN_POINT ( 'NONE',  ( 36.27727800054010743, -280.1036604844420594, -268.5873393084081613 ) ) ;
#69380 = CARTESIAN_POINT ( 'NONE',  ( -101.0618137784083927, -287.0846222468462656, -230.7079353797111025 ) ) ;
#69381 = CARTESIAN_POINT ( 'NONE',  ( -108.0047395983793024, -280.0186916642916231, -250.4684590381736768 ) ) ;
#69382 = CARTESIAN_POINT ( 'NONE',  ( 154.0637704119390321, 19.72112694978656222, -13.30738029212319695 ) ) ;
#69383 = CARTESIAN_POINT ( 'NONE',  ( -41.95701226949705642, -293.9941322649137305, -195.5032557114952851 ) ) ;
#69384 = CARTESIAN_POINT ( 'NONE',  ( -79.68042081936802390, -275.8552945232693787, -333.5228601610585315 ) ) ;
#69385 = CARTESIAN_POINT ( 'NONE',  ( -29.69452379241713658, -277.6043300044238435, -343.1129437645186613 ) ) ;
#69386 = CARTESIAN_POINT ( 'NONE',  ( -108.4811609076313772, -286.2390008513100952, -294.6346744947704792 ) ) ;
#69387 = FACE_OUTER_BOUND ( 'NONE', #13266, .T. ) ;
#69388 = CARTESIAN_POINT ( 'NONE',  ( -94.35537848841242692, -291.7892380602669391, -319.9469494255017139 ) ) ;
#69389 = CARTESIAN_POINT ( 'NONE',  ( -63.94642986785227379, -293.3988062045393690, -340.5384513318622908 ) ) ;
#69390 = CARTESIAN_POINT ( 'NONE',  ( 39.44242436935382301, -286.8002474509322610, -274.4246113523318513 ) ) ;
#69391 = CARTESIAN_POINT ( 'NONE',  ( -63.06063917047178791, -290.1114013042531496, -201.1875927756718738 ) ) ;
#69392 = CARTESIAN_POINT ( 'NONE',  ( 196.0143093133015384, 73.40565171261609123, 11.99999999999998757 ) ) ;
#69393 = CARTESIAN_POINT ( 'NONE',  ( 15.94398068009744307, -274.9617416160315884, -320.9761325423675657 ) ) ;
#69394 = CARTESIAN_POINT ( 'NONE',  ( -8.777125805074488696, -292.8140207091449270, -338.8945153180375200 ) ) ;
#69395 = CARTESIAN_POINT ( 'NONE',  ( 113.5000000000000568, -212.3147208684173108, -422.1836331355066818 ) ) ;
#69396 = CARTESIAN_POINT ( 'NONE',  ( 197.0547923074542780, 42.37849028824485487, 12.19783058971606593 ) ) ;
#69397 = CARTESIAN_POINT ( 'NONE',  ( -92.29917155378441862, -289.7640534626253839, -217.3484180542841955 ) ) ;
#69398 = CARTESIAN_POINT ( 'NONE',  ( -108.8084139374457351, -286.3926812883466368, -251.9505440025732241 ) ) ;
#69399 = CARTESIAN_POINT ( 'NONE',  ( 30.76904521955583149, -286.2320741222289371, -304.1679973948490669 ) ) ;
#69400 = CARTESIAN_POINT ( 'NONE',  ( -108.6037636650999048, -286.2178534755499300, -252.0010194256967964 ) ) ;
#69401 = CARTESIAN_POINT ( 'NONE',  ( 121.3395553409046670, -299.5541904835127980, -198.1000099699160444 ) ) ;
#69402 = CARTESIAN_POINT ( 'NONE',  ( -91.64793505991495692, -286.0562151238987099, -221.2618291277825904 ) ) ;
#69403 = ADVANCED_FACE ( 'NONE', ( #67879 ), #18611, .T. ) ;
#69404 = CARTESIAN_POINT ( 'NONE',  ( 31.91506390335319310, -295.9200497360366171, -300.1899273375339021 ) ) ;
#69405 = CIRCLE ( 'NONE', #8902, 11.68950434577434372 ) ;
#69406 = CARTESIAN_POINT ( 'NONE',  ( -42.72837979928182506, -275.1994756122139734, -345.7288689153223231 ) ) ;
#69407 = CARTESIAN_POINT ( 'NONE',  ( -9.215591531353517496, -277.0275857541622031, -342.0177039096741964 ) ) ;
#69408 = CARTESIAN_POINT ( 'NONE',  ( -11.62001420522589257, -290.4642371877069422, -199.2588891646350362 ) ) ;
#69409 = CARTESIAN_POINT ( 'NONE',  ( -114.0791115065781725, -278.4649831994051965, -277.3310780118933394 ) ) ;
#69410 = CARTESIAN_POINT ( 'NONE',  ( -94.32199081411876307, -297.8616100733190137, -318.6001317323788271 ) ) ;
#69411 = CARTESIAN_POINT ( 'NONE',  ( -48.18343439339304268, -249.1487204936213971, -480.0094059802160018 ) ) ;
#69412 = FACE_OUTER_BOUND ( 'NONE', #62608, .T. ) ;
#69413 = CARTESIAN_POINT ( 'NONE',  ( -52.17219592184963517, -284.5431086975402195, -198.3798713199116435 ) ) ;
#69414 = CARTESIAN_POINT ( 'NONE',  ( -85.93132192577222384, -275.8729011566883855, -326.5533265629862854 ) ) ;
#69415 = CARTESIAN_POINT ( 'NONE',  ( 24.27236515191030009, -280.1322721924374264, -313.1470853277362494 ) ) ;
#69416 = CARTESIAN_POINT ( 'NONE',  ( 196.8803347170859865, 24.42324672360809856, 12.49999999999999289 ) ) ;
#69417 = CARTESIAN_POINT ( 'NONE',  ( 31.93183840629263415, -273.6175164064592877, -238.2370238571341474 ) ) ;
#69418 = CARTESIAN_POINT ( 'NONE',  ( -99.26584843626726240, -277.3638847558975158, -309.3053025640978149 ) ) ;
#69419 = CARTESIAN_POINT ( 'NONE',  ( 36.31369746165925250, -295.0413854402277707, -267.9967668029023002 ) ) ;
#69420 = CARTESIAN_POINT ( 'NONE',  ( -5.061536280651216302, -279.3875655840416812, -200.7947214030889427 ) ) ;
#69421 = CARTESIAN_POINT ( 'NONE',  ( 1.705393863920346975, -295.4575749099768132, -332.3786931559660047 ) ) ;
#69422 = CARTESIAN_POINT ( 'NONE',  ( -100.3540685539231134, -298.4440960540918013, -226.9475399014949346 ) ) ;
#69423 = CARTESIAN_POINT ( 'NONE',  ( -63.07747839314306759, -297.5408842529122921, -201.9946117079880139 ) ) ;
#69424 = CARTESIAN_POINT ( 'NONE',  ( -98.40413833343902184, -293.1454919977227291, -226.7257971800193275 ) ) ;
#69425 = CARTESIAN_POINT ( 'NONE',  ( -33.72945163228306598, -286.2631108636859949, -193.4458940972773746 ) ) ;
#69426 = CARTESIAN_POINT ( 'NONE',  ( 35.68857311150232903, -273.9491126216996690, -290.5808188123639297 ) ) ;
#69427 = CARTESIAN_POINT ( 'NONE',  ( -23.31402084651426421, -288.7110001825039944, -346.1266860558930603 ) ) ;
#69428 = CARTESIAN_POINT ( 'NONE',  ( -103.6278531975442689, -280.9898281879271735, -235.9266545479738966 ) ) ;
#69429 = EDGE_CURVE ( 'NONE', #77857, #17873, #39896, .T. ) ;
#69430 = CARTESIAN_POINT ( 'NONE',  ( 34.51269112357425684, -286.7978729038478036, -284.5805697825753100 ) ) ;
#69431 = CARTESIAN_POINT ( 'NONE',  ( -80.75151250047828455, -289.4629772906923790, -209.2007645179615736 ) ) ;
#69432 = ORIENTED_EDGE ( 'NONE', *, *, #27196, .F. ) ;
#69433 = CARTESIAN_POINT ( 'NONE',  ( -102.0362518552990423, -259.7623939308359695, -328.6249738900723969 ) ) ;
#69434 = CARTESIAN_POINT ( 'NONE',  ( -61.28108940861380205, -288.8792550081258810, -339.3893302039106175 ) ) ;
#69435 = FACE_OUTER_BOUND ( 'NONE', #38123, .T. ) ;
#69436 = CARTESIAN_POINT ( 'NONE',  ( -76.62714499559241688, -284.5052501248687236, -336.3732853822853031 ) ) ;
#69437 = CARTESIAN_POINT ( 'NONE',  ( -40.61036776083165023, -291.0707700265456310, -193.6528912313968078 ) ) ;
#69438 = CARTESIAN_POINT ( 'NONE',  ( 28.58414392714239582, -282.6501001470448955, -232.1482471207737035 ) ) ;
#69439 = CARTESIAN_POINT ( 'NONE',  ( 39.14689015336591638, -282.8257966658646865, -267.0618306769619039 ) ) ;
#69440 = CARTESIAN_POINT ( 'NONE',  ( 32.95887426622155658, -281.6454265011823281, -290.0290930778809297 ) ) ;
#69441 = CARTESIAN_POINT ( 'NONE',  ( 23.89960802109775528, -276.9638032042099098, -227.0433675002260827 ) ) ;
#69442 = CARTESIAN_POINT ( 'NONE',  ( -98.27445923397482375, -295.9237694725378560, -317.4376393891290604 ) ) ;
#69443 = CARTESIAN_POINT ( 'NONE',  ( -96.26414359644908814, -287.9406642249805373, -316.2074531922903589 ) ) ;
#69444 = CARTESIAN_POINT ( 'NONE',  ( -39.16228013766123439, -296.9491326165413057, -197.0621530590104840 ) ) ;
#69445 = ORIENTED_EDGE ( 'NONE', *, *, #9361, .F. ) ;
#69446 = ORIENTED_EDGE ( 'NONE', *, *, #21097, .T. ) ;
#69447 = CARTESIAN_POINT ( 'NONE',  ( -111.8311986425008655, -286.4647658536589461, -270.9445170679634316 ) ) ;
#69448 = CARTESIAN_POINT ( 'NONE',  ( 19.31066272960425323, -295.3380893840782164, -322.1298996623218045 ) ) ;
#69449 = CARTESIAN_POINT ( 'NONE',  ( -65.34708510383936186, -284.0795494377312025, -337.8994789742364446 ) ) ;
#69450 = CARTESIAN_POINT ( 'NONE',  ( -11.95534101051359954, -275.7885212533428216, -342.8623874599227292 ) ) ;
#69451 = CARTESIAN_POINT ( 'NONE',  ( -99.12764888475417990, -291.8131947163757332, -224.5590464796171375 ) ) ;
#69452 = CARTESIAN_POINT ( 'NONE',  ( -99.96200840901717299, -283.2644397458983008, -227.6187168763532327 ) ) ;
#69453 = CARTESIAN_POINT ( 'NONE',  ( 11.10218649761893062, -293.0349503802119102, -210.4683474772775185 ) ) ;
#69454 = CARTESIAN_POINT ( 'NONE',  ( -104.0653111308672720, -290.4846908128180303, -300.1515639711514609 ) ) ;
#69455 = PLANE ( 'NONE',  #74693 ) ;
#69456 = CARTESIAN_POINT ( 'NONE',  ( 159.4851178187871312, 15.00000000000000000, -9.000000000000001776 ) ) ;
#69457 = CARTESIAN_POINT ( 'NONE',  ( 196.8450047754690786, 281.6590421831631375, -110.2675066226584306 ) ) ;
#69458 = CARTESIAN_POINT ( 'NONE',  ( -85.64836685764284141, -285.2269756160812335, -329.4303460151899117 ) ) ;
#69459 = CARTESIAN_POINT ( 'NONE',  ( -106.6662871844225293, -281.6237833571634610, -303.7098442033569086 ) ) ;
#69460 = ORIENTED_EDGE ( 'NONE', *, *, #56503, .F. ) ;
#69461 = CARTESIAN_POINT ( 'NONE',  ( 34.23927659396760248, -280.6803394542382080, -286.1848295005096929 ) ) ;
#69462 = CARTESIAN_POINT ( 'NONE',  ( 10.50959377909168957, -276.0788510585550739, -330.7284183860144822 ) ) ;
#69463 = CARTESIAN_POINT ( 'NONE',  ( -93.60320318817002772, -281.2394580563473028, -220.9992240685792240 ) ) ;
#69464 = CARTESIAN_POINT ( 'NONE',  ( 191.1870090034608722, 268.7882272122546965, -138.6016306282632229 ) ) ;
#69465 = CARTESIAN_POINT ( 'NONE',  ( 12.62070560280848319, -279.3077516454175111, -212.5479334572429764 ) ) ;
#69466 = CARTESIAN_POINT ( 'NONE',  ( -110.5369872706778125, -282.7611163219394825, -255.7222400936766746 ) ) ;
#69467 = CARTESIAN_POINT ( 'NONE',  ( -35.87538550795238734, -299.8304042988154947, -194.3740123294689965 ) ) ;
#69468 = CARTESIAN_POINT ( 'NONE',  ( -108.0275227610104167, -296.8001298739014260, -288.8903634243297915 ) ) ;
#69469 = EDGE_LOOP ( 'NONE', ( #62189, #64863, #20706, #51989 ) ) ;
#69470 = CARTESIAN_POINT ( 'NONE',  ( -101.5464035355524288, -289.7239590354090524, -234.4935303490441356 ) ) ;
#69471 = CARTESIAN_POINT ( 'NONE',  ( -25.77710018954696025, -277.5599348301415716, -346.3846197080057436 ) ) ;
#69472 = CARTESIAN_POINT ( 'NONE',  ( -27.29017932440858019, -274.1833156033798673, -198.0055382361872205 ) ) ;
#69473 = CARTESIAN_POINT ( 'NONE',  ( 28.82229840856515324, -274.9792990288836450, -309.1402077959008921 ) ) ;
#69474 = CARTESIAN_POINT ( 'NONE',  ( 215.9306832106270804, -324.2391364535881735, 9.184850993605165694E-16 ) ) ;
#69475 = CARTESIAN_POINT ( 'NONE',  ( -109.1535629427707761, -270.8328122144964709, -248.5502976032099696 ) ) ;
#69476 = CARTESIAN_POINT ( 'NONE',  ( 222.8344101925596306, 2.184664232470858947E-16, -8.757359312880716118 ) ) ;
#69477 = CONICAL_SURFACE ( 'NONE', #28665, 5.024999999999987921, 0.7853981633974482790 ) ;
#69478 = CARTESIAN_POINT ( 'NONE',  ( -43.51792863845375336, -250.6687662136113488, -486.1009916026080759 ) ) ;
#69479 = CARTESIAN_POINT ( 'NONE',  ( -38.87782810695519942, -284.1515094091836886, -343.6666792295779373 ) ) ;
#69480 = CARTESIAN_POINT ( 'NONE',  ( -8.403753812197678030, -284.4387593180005638, -340.6776451799821643 ) ) ;
#69481 = CONICAL_SURFACE ( 'NONE', #40715, 4.000000000000003553, 1.029744258676654534 ) ;
#69482 = CARTESIAN_POINT ( 'NONE',  ( -107.4503514271510767, -284.1764063920904846, -249.4812855012324064 ) ) ;
#69483 = CARTESIAN_POINT ( 'NONE',  ( 8.056652841658774378, -274.8199126588855847, -328.6106691162278253 ) ) ;
#69484 = CARTESIAN_POINT ( 'NONE',  ( 8.576272517067319967, -284.2763221306306605, -328.7569247596914579 ) ) ;
#69485 = CARTESIAN_POINT ( 'NONE',  ( -93.26530470542337525, -276.3552181164891408, -318.3533903285371593 ) ) ;
#69486 = CARTESIAN_POINT ( 'NONE',  ( 114.7448031289451222, -299.5541904835127980, -198.3007743052732792 ) ) ;
#69487 = CARTESIAN_POINT ( 'NONE',  ( 197.1033433601519107, 72.78980819445995110, -12.11496968317325873 ) ) ;
#69488 = CARTESIAN_POINT ( 'NONE',  ( -111.9316427951227411, -279.5869213807203550, -251.8544833326130004 ) ) ;
#69489 = VERTEX_POINT ( 'NONE', #92318 ) ;
#69490 = ORIENTED_EDGE ( 'NONE', *, *, #24839, .F. ) ;
#69491 = CARTESIAN_POINT ( 'NONE',  ( 197.3663942936549347, 19.61288093082368533, 11.77299963048777620 ) ) ;
#69492 = CARTESIAN_POINT ( 'NONE',  ( -101.4855418731528403, -286.9491505258046686, -230.0390018973986628 ) ) ;
#69493 = EDGE_CURVE ( 'NONE', #53411, #84479, #61817, .T. ) ;
#69494 = CARTESIAN_POINT ( 'NONE',  ( 1.647256885009238392, -293.7137714050210775, -332.3280024614030594 ) ) ;
#69495 = CARTESIAN_POINT ( 'NONE',  ( -93.52400366868117487, -289.1831090167933098, -322.9436931885342119 ) ) ;
#69496 = CARTESIAN_POINT ( 'NONE',  ( 13.85648495682666770, -285.0215122446341525, -216.8420967159271129 ) ) ;
#69498 = CARTESIAN_POINT ( 'NONE',  ( -105.6294734056318845, -289.1712406661733326, -241.6839482297548329 ) ) ;
#69497 = CARTESIAN_POINT ( 'NONE',  ( 19.12547874439903950, -285.4622756829367063, -223.1521526243907658 ) ) ;
#69499 = CARTESIAN_POINT ( 'NONE',  ( -109.8156424661205222, -285.9105290961912260, -258.6771736978408853 ) ) ;
#69500 = CARTESIAN_POINT ( 'NONE',  ( 30.04677536129861082, -273.9873451767913934, -303.4003539869329416 ) ) ;
#69501 = CARTESIAN_POINT ( 'NONE',  ( 29.44036529408687386, -285.4705646659645595, -233.5555854469791939 ) ) ;
#69502 = CARTESIAN_POINT ( 'NONE',  ( -99.11814275560450938, -299.1289719495663348, -227.8100562063340817 ) ) ;
#69503 = CARTESIAN_POINT ( 'NONE',  ( 23.24112150529521870, -284.9465970999091837, -225.8667346073227122 ) ) ;
#69504 = CARTESIAN_POINT ( 'NONE',  ( -7.915870426184912212, -281.3886525869224897, -203.2837836643297749 ) ) ;
#69505 = CARTESIAN_POINT ( 'NONE',  ( -34.70500001451793537, -291.0192456441765216, -345.4815296015473223 ) ) ;
#69506 = CARTESIAN_POINT ( 'NONE',  ( 189.9243309297870610, 275.0000000000000568, 20.22542485937349355 ) ) ;
#69507 = CARTESIAN_POINT ( 'NONE',  ( 195.5238343228637916, 40.22264805511078833, 13.82193646908953610 ) ) ;
#69508 = CARTESIAN_POINT ( 'NONE',  ( -85.45914795579160739, -297.6316861945697383, -328.6193827157596274 ) ) ;
#69509 = CARTESIAN_POINT ( 'NONE',  ( -101.1564221430063242, -277.0820326420379160, -230.8580107957405403 ) ) ;
#69510 = CARTESIAN_POINT ( 'NONE',  ( -30.70101279077371004, -291.3311158970092265, -193.7574409809942324 ) ) ;
#69511 = CARTESIAN_POINT ( 'NONE',  ( -80.17599929689119165, -295.8611025512300898, -210.2640030096187616 ) ) ;
#69512 = CARTESIAN_POINT ( 'NONE',  ( 17.96500432436192796, -280.9229303009006458, -318.7595882219055738 ) ) ;
#69513 = CARTESIAN_POINT ( 'NONE',  ( -38.07243738793426502, -272.1227723196129773, -195.9247006543479301 ) ) ;
#69514 = CARTESIAN_POINT ( 'NONE',  ( 18.84284627870105311, -294.1987148133409278, -222.9845391241362904 ) ) ;
#69515 = CARTESIAN_POINT ( 'NONE',  ( 10.64812456238589888, -296.9090924074130271, -330.4860931364851808 ) ) ;
#69516 = CARTESIAN_POINT ( 'NONE',  ( -108.7951894671945041, -294.6885344560242288, -297.2891440076819549 ) ) ;
#69517 = CARTESIAN_POINT ( 'NONE',  ( 6.017152072562857335, -292.7131223114755585, -332.8270126763905523 ) ) ;
#69518 = CARTESIAN_POINT ( 'NONE',  ( -98.59111584620231383, -291.4154237662127684, -311.1747844643946905 ) ) ;
#69519 = CARTESIAN_POINT ( 'NONE',  ( 209.9972545312790544, 27.55378999303206200, 10.50000000000000000 ) ) ;
#69520 = CARTESIAN_POINT ( 'NONE',  ( -94.42330362243954767, -292.0005106644792932, -224.5777691534463258 ) ) ;
#69521 = B_SPLINE_CURVE_WITH_KNOTS ( 'NONE', 3,
 ( #54594, #17231, #62187, #25711 ),
 .UNSPECIFIED., .F., .F.,
 ( 4, 4 ),
 ( 0.000000000000000000, 9.632970524402617444E-05 ),
 .UNSPECIFIED. ) ;
#69522 = CARTESIAN_POINT ( 'NONE',  ( 139.6925840978351516, 15.36528803885690664, -21.50000000000000000 ) ) ;
#69524 = CARTESIAN_POINT ( 'NONE',  ( 33.11670124815748295, -293.8049571239789088, -289.5035058035148268 ) ) ;
#69523 = CARTESIAN_POINT ( 'NONE',  ( -1.187225902346443318, -280.5950860486489660, -336.4912467594318173 ) ) ;
#69525 = CARTESIAN_POINT ( 'NONE',  ( 27.85135275202823735, -281.0145239857965862, -229.2872291557859512 ) ) ;
#69526 = CARTESIAN_POINT ( 'NONE',  ( -114.3196013377307025, -284.2236682712230618, -269.9776902938024250 ) ) ;
#69527 = CARTESIAN_POINT ( 'NONE',  ( -48.35535419701226800, -287.1923465995993183, -344.4318521171526868 ) ) ;
#69528 = CARTESIAN_POINT ( 'NONE',  ( -108.9589582432861903, -282.4373116804489996, -289.9497373114602397 ) ) ;
#69529 = CARTESIAN_POINT ( 'NONE',  ( -31.11089127851601788, -278.6092638056593955, -194.2570459774840970 ) ) ;
#69530 = CARTESIAN_POINT ( 'NONE',  ( -37.96607899856367396, -284.9648356159121931, -193.6727703522207662 ) ) ;
#69531 = CARTESIAN_POINT ( 'NONE',  ( 196.1569681665548330, 42.06793861907576826, 13.67794394913816447 ) ) ;
#69532 = CARTESIAN_POINT ( 'NONE',  ( 30.23063850712377487, -295.5471272745234046, -300.0329811615882249 ) ) ;
#69533 = CARTESIAN_POINT ( 'NONE',  ( -28.64989671812455896, -278.3693854571712905, -346.3290974306423209 ) ) ;
#69534 = CARTESIAN_POINT ( 'NONE',  ( -110.1794365029900860, -278.2870790740148550, -265.1889185968924494 ) ) ;
#69535 = CARTESIAN_POINT ( 'NONE',  ( -112.3177557784249530, -290.9381777740092048, -252.8228431628078283 ) ) ;
#69536 = CARTESIAN_POINT ( 'NONE',  ( -19.28663378117657601, -280.9016039972770500, -343.7862150809997956 ) ) ;
#69537 = CARTESIAN_POINT ( 'NONE',  ( 31.75808359013602455, -292.9344627656906823, -294.7745538413889790 ) ) ;
#69538 = B_SPLINE_CURVE_WITH_KNOTS ( 'NONE', 3,
 ( #33681, #40289, #55937, #69205, #77719, #70626 ),
 .UNSPECIFIED., .F., .F.,
 ( 4, 2, 4 ),
 ( 0.0002823611672359634833, 0.0005641097415182887501, 0.0008458583158006138542 ),
 .UNSPECIFIED. ) ;
#69539 = CARTESIAN_POINT ( 'NONE',  ( -110.3645422528903737, -294.3316239379112744, -287.5242054714675533 ) ) ;
#69540 = ORIENTED_EDGE ( 'NONE', *, *, #93458, .T. ) ;
#69541 = CARTESIAN_POINT ( 'NONE',  ( 175.2296996224750103, 133.0000000000000000, -24.00000000000001066 ) ) ;
#69542 = CARTESIAN_POINT ( 'NONE',  ( -34.30490732508198448, -294.5205949036196671, -343.3595174942433914 ) ) ;
#69543 = DIRECTION ( 'NONE',  ( 0.000000000000000000, 0.000000000000000000, -1.000000000000000000 ) ) ;
#69544 = VECTOR ( 'NONE', #20023, 1000.000000000000114 ) ;
#69545 = CARTESIAN_POINT ( 'NONE',  ( -105.5937364680635966, -293.8380690714490129, -285.9065529553535612 ) ) ;
#69546 = CARTESIAN_POINT ( 'NONE',  ( -70.61617690632397171, -296.6827749010979005, -201.1828742247705293 ) ) ;
#69547 = CARTESIAN_POINT ( 'NONE',  ( 25.27339112443712565, -279.1189327153433624, -227.6121128796392838 ) ) ;
#69548 = CARTESIAN_POINT ( 'NONE',  ( -49.28437614253680010, -287.2182936830355402, -194.7387449098748391 ) ) ;
#69549 = CARTESIAN_POINT ( 'NONE',  ( 32.31297602119136769, -287.6770031641011656, -292.3748472534764460 ) ) ;
#69550 = CARTESIAN_POINT ( 'NONE',  ( -26.90436270166161137, -278.4371500327605986, -343.3115788357914084 ) ) ;
#69551 = CARTESIAN_POINT ( 'NONE',  ( -107.5424911924934008, -294.2399679148196014, -295.8844054648898236 ) ) ;
#69552 = CARTESIAN_POINT ( 'NONE',  ( -110.2782175177796660, -298.4759665512610809, -257.7818316049368832 ) ) ;
#69553 = EDGE_CURVE ( 'NONE', #31710, #5311, #79078, .T. ) ;
#69554 = CARTESIAN_POINT ( 'NONE',  ( -103.4955181729308720, -276.9178740636837688, -302.2718954800412803 ) ) ;
#69555 = ORIENTED_EDGE ( 'NONE', *, *, #43643, .T. ) ;
#69556 = CARTESIAN_POINT ( 'NONE',  ( -36.53663737784922461, -297.7286944007803413, -193.3823058181700105 ) ) ;
#69557 = CARTESIAN_POINT ( 'NONE',  ( -96.90614746118225753, -291.8574368116718460, -315.0297871423659899 ) ) ;
#69558 = CARTESIAN_POINT ( 'NONE',  ( 33.70942227791663726, -294.7981239755835077, -242.6803627348150201 ) ) ;
#69559 = CARTESIAN_POINT ( 'NONE',  ( -113.5925053212108367, -274.1217662500657752, -270.3811029296526272 ) ) ;
#69560 = ADVANCED_FACE ( 'NONE', ( #75442 ), #67424, .F. ) ;
#69561 = CARTESIAN_POINT ( 'NONE',  ( -106.1256812250172317, -290.8743708587069818, -295.1130191723560756 ) ) ;
#69562 = CARTESIAN_POINT ( 'NONE',  ( -43.52494566250408070, -249.8916412613903901, -454.3875622718719569 ) ) ;
#69563 = ORIENTED_EDGE ( 'NONE', *, *, #82280, .T. ) ;
#69564 = CARTESIAN_POINT ( 'NONE',  ( -107.6831522978168181, -297.6019857336125938, -239.1586606603594021 ) ) ;
#69565 = CARTESIAN_POINT ( 'NONE',  ( -111.4270734077455387, -288.8941166746070053, -254.4361121468469662 ) ) ;
#69566 = CARTESIAN_POINT ( 'NONE',  ( -48.97098675466904893, -298.2412898071205518, -194.2121049031047733 ) ) ;
#69567 = DIRECTION ( 'NONE',  ( 0.000000000000000000, 0.000000000000000000, 1.000000000000000000 ) ) ;
#69568 = CARTESIAN_POINT ( 'NONE',  ( 195.0811277873548306, 27.06158795357637104, 15.19607843539318104 ) ) ;
#69569 = CARTESIAN_POINT ( 'NONE',  ( -4.612731704203378413, -290.1489117453890003, -339.3067565660630294 ) ) ;
#69570 = CARTESIAN_POINT ( 'NONE',  ( -2.659677404128715672, -276.9805209788415823, -198.2697987213421698 ) ) ;
#69571 = CARTESIAN_POINT ( 'NONE',  ( -75.68071226403637297, -287.5393609505711083, -206.0948859875217920 ) ) ;
#69572 = CARTESIAN_POINT ( 'NONE',  ( -10.18625753643228471, -284.9743684092888429, -198.8821429856936902 ) ) ;
#69573 = CARTESIAN_POINT ( 'NONE',  ( -29.77990311428824199, -272.1479549997527556, -195.9108147473772306 ) ) ;
#69574 = CARTESIAN_POINT ( 'NONE',  ( -32.62371850801106632, -276.0322066089227633, -196.0580029286489321 ) ) ;
#69575 = CARTESIAN_POINT ( 'NONE',  ( -110.1132355926697670, -288.8347416479156777, -254.6889187880003647 ) ) ;
#69576 = CARTESIAN_POINT ( 'NONE',  ( -31.52113279118070466, -278.8399530403050903, -345.9537895888056482 ) ) ;
#69577 = PRODUCT_DEFINITION ( 'UNKNOWN', '', #8384, #206 ) ;
#69578 = ORIENTED_EDGE ( 'NONE', *, *, #11260, .T. ) ;
#69580 = CARTESIAN_POINT ( 'NONE',  ( 34.80282127787744173, -281.0560806271518572, -282.1535180532416121 ) ) ;
#69579 = CARTESIAN_POINT ( 'NONE',  ( -16.92171599363927825, -280.3233262224409259, -200.2752831230883714 ) ) ;
#69581 = CARTESIAN_POINT ( 'NONE',  ( 12.51413602631390809, -277.4557462844888960, -328.6353671004637249 ) ) ;
#69582 = CARTESIAN_POINT ( 'NONE',  ( 36.94993633285494639, -280.1122101018423223, -251.6859614396394420 ) ) ;
#69583 = CARTESIAN_POINT ( 'NONE',  ( 183.2096664736218941, 262.1940599670854226, -151.6038608880942604 ) ) ;
#69584 = CARTESIAN_POINT ( 'NONE',  ( 22.46525358159449937, -277.1405311111119545, -318.5062170397638965 ) ) ;
#69585 = CARTESIAN_POINT ( 'NONE',  ( 18.83135759094050599, -300.1677098511511872, -193.9370241457030772 ) ) ;
#69586 = CARTESIAN_POINT ( 'NONE',  ( -69.91165696735023971, -294.1233781216987495, -202.8022627189028810 ) ) ;
#69587 = ORIENTED_EDGE ( 'NONE', *, *, #89784, .F. ) ;
#69588 = CARTESIAN_POINT ( 'NONE',  ( 200.2296996224750103, 68.12454877777268791, 0.000000000000000000 ) ) ;
#69589 = CARTESIAN_POINT ( 'NONE',  ( 10.32664862597122202, -289.4561147116154984, -326.1234433550667973 ) ) ;
#69590 = CARTESIAN_POINT ( 'NONE',  ( 37.02706177743279170, -289.1138289212092332, -254.7013684694493065 ) ) ;
#69591 = CARTESIAN_POINT ( 'NONE',  ( -94.18878076761573936, -289.2515921764393170, -316.3209057467874459 ) ) ;
#69592 = CARTESIAN_POINT ( 'NONE',  ( 16.26081180745041621, -286.2964823327575914, -215.1678428729391328 ) ) ;
#69593 = CARTESIAN_POINT ( 'NONE',  ( 46.30223402071163008, 11.84457614133316739, -331.9951998377467248 ) ) ;
#69594 = CARTESIAN_POINT ( 'NONE',  ( 34.09278559577506229, -280.1946581799574574, -288.9466275635909938 ) ) ;
#69595 = CARTESIAN_POINT ( 'NONE',  ( -12.85852211518442978, -290.5909469464642712, -340.4427808746546589 ) ) ;
#69596 = CARTESIAN_POINT ( 'NONE',  ( 16.31754883453841742, -280.7530912225772681, -320.9460301366980275 ) ) ;
#69597 = CARTESIAN_POINT ( 'NONE',  ( -54.62490118411572126, -281.1406908207898141, -198.8765383312015729 ) ) ;
#69598 = CARTESIAN_POINT ( 'NONE',  ( -87.13289349890753499, -278.2610595509717655, -323.8291037706811721 ) ) ;
#69599 = CARTESIAN_POINT ( 'NONE',  ( -112.4815312297281480, -289.1589320936956824, -285.3278223799621287 ) ) ;
#69600 = CARTESIAN_POINT ( 'NONE',  ( -80.85519803970743169, -286.2811265091950190, -206.9665304403151254 ) ) ;
#69601 = CARTESIAN_POINT ( 'NONE',  ( -113.8420065473951439, -284.9418712398101547, -278.5605094777939144 ) ) ;
#69602 = CARTESIAN_POINT ( 'NONE',  ( -13.52736033071201227, -282.9009932185252865, -339.4210794726359381 ) ) ;
#69603 = ORIENTED_EDGE ( 'NONE', *, *, #73898, .F. ) ;
#69604 = DIRECTION ( 'NONE',  ( 1.000000000000000000, 0.000000000000000000, -0.000000000000000000 ) ) ;
#69605 = CARTESIAN_POINT ( 'NONE',  ( -111.0553320826483628, -292.1892972883025550, -287.9267245971706188 ) ) ;
#69606 = CARTESIAN_POINT ( 'NONE',  ( 23.59268187554334517, -291.6162989534926737, -224.0761843295774725 ) ) ;
#69607 = CARTESIAN_POINT ( 'NONE',  ( -21.87267913420982879, -273.3140358340575062, -198.7781742259252553 ) ) ;
#69608 = CARTESIAN_POINT ( 'NONE',  ( -107.0774262175834508, -295.4854319956171480, -302.7685444931653365 ) ) ;
#69609 = AXIS2_PLACEMENT_3D ( 'NONE', #5159, #48210, #71429 ) ;
#69610 = CARTESIAN_POINT ( 'NONE',  ( -94.81962833724782058, -289.6779324196597258, -224.2217100824878173 ) ) ;
#69611 = CARTESIAN_POINT ( 'NONE',  ( -45.22058505916535864, -293.3930169018261154, -344.0050752340478653 ) ) ;
#69612 = CARTESIAN_POINT ( 'NONE',  ( -34.54759563645244214, -290.2214813549700807, -343.7548400750943642 ) ) ;
#69613 = DIRECTION ( 'NONE',  ( 0.000000000000000000, 0.000000000000000000, -1.000000000000000000 ) ) ;
#69614 = CARTESIAN_POINT ( 'NONE',  ( -96.56424898580104355, -291.9213121697696351, -316.3794877895917352 ) ) ;
#69615 = CARTESIAN_POINT ( 'NONE',  ( 37.67065740580651578, -291.6233253230812466, -275.9293257105272232 ) ) ;
#69616 = VECTOR ( 'NONE', #48551, 1000.000000000000000 ) ;
#69617 = CARTESIAN_POINT ( 'NONE',  ( -17.64850385707197233, -296.7984314159474479, -342.7827073950271028 ) ) ;
#69618 = CARTESIAN_POINT ( 'NONE',  ( 4.851173008370035511, -287.5787675610760061, -210.4394824881779584 ) ) ;
#69619 = CARTESIAN_POINT ( 'NONE',  ( -6.525455917431348674, -296.6485726010029680, -338.9204902271051196 ) ) ;
#69620 = CARTESIAN_POINT ( 'NONE',  ( 6.262250606421436494, -276.6203681421435476, -208.8389617503153488 ) ) ;
#69621 = CARTESIAN_POINT ( 'NONE',  ( 18.60268395288361987, -275.0645187968849541, -322.6892615419374124 ) ) ;
#69622 = CARTESIAN_POINT ( 'NONE',  ( -114.2397671894841977, -271.9008437961486493, -270.3528422294329516 ) ) ;
#69623 = CARTESIAN_POINT ( 'NONE',  ( 3.677337364212458048, -274.7316543228658361, -331.9680378466097181 ) ) ;
#69624 = CARTESIAN_POINT ( 'NONE',  ( -79.85767418267377593, -277.5519731276427251, -209.2570580049286662 ) ) ;
#69625 = CARTESIAN_POINT ( 'NONE',  ( -110.5861565558097936, -273.8288976279920348, -264.8991047990763263 ) ) ;
#69626 = CARTESIAN_POINT ( 'NONE',  ( -24.24262633470192441, -272.7908489176789999, -195.0277482228061672 ) ) ;
#69627 = CARTESIAN_POINT ( 'NONE',  ( -110.3870821411951795, -297.8552413666325833, -279.6984704839471192 ) ) ;
#69628 = CARTESIAN_POINT ( 'NONE',  ( 156.4851178187871312, 0.000000000000000000, 7.000000000000000000 ) ) ;
#69629 = CARTESIAN_POINT ( 'NONE',  ( -84.18605128844980356, -298.1918057863896365, -214.0970248975252730 ) ) ;
#69630 = DIRECTION ( 'NONE',  ( -0.3024135303175699008, -0.9531768234073173529, 0.000000000000000000 ) ) ;
#69632 = CARTESIAN_POINT ( 'NONE',  ( -99.27935614528134067, -272.9187307297765983, -231.7252955946296993 ) ) ;
#69631 = CARTESIAN_POINT ( 'NONE',  ( 20.21603067845342139, -286.2418557052944266, -318.9976724483742601 ) ) ;
#69633 = CARTESIAN_POINT ( 'NONE',  ( 31.42179433457710402, -287.1062884127480856, -235.7117048665498373 ) ) ;
#69634 = CARTESIAN_POINT ( 'NONE',  ( -87.37391542011741308, -289.3942230992265650, -328.9334576981514147 ) ) ;
#69635 = CARTESIAN_POINT ( 'NONE',  ( -110.6986872199104681, -298.3110318210101468, -287.6551597561391986 ) ) ;
#69636 = CARTESIAN_POINT ( 'NONE',  ( 0.1387545234021022866, -292.5521961343963540, -335.1909533157337933 ) ) ;
#69637 = CARTESIAN_POINT ( 'NONE',  ( 28.16198690622840672, -281.2763932557025441, -310.6294015380410656 ) ) ;
#69638 = CARTESIAN_POINT ( 'NONE',  ( 153.1745786719506270, 129.2309077672098283, -12.62609896151546351 ) ) ;
#69639 = CARTESIAN_POINT ( 'NONE',  ( -110.2517982017299261, -276.3255934586799754, -287.9965871591145969 ) ) ;
#69640 = CARTESIAN_POINT ( 'NONE',  ( -113.5000000000000568, -296.0521521680024080, -400.5374811273811702 ) ) ;
#69641 = CARTESIAN_POINT ( 'NONE',  ( -70.16373953786280993, -288.2894920572687738, -336.0244581608257022 ) ) ;
#69642 = DIRECTION ( 'NONE',  ( -0.000000000000000000, -0.000000000000000000, -1.000000000000000000 ) ) ;
#69643 = CARTESIAN_POINT ( 'NONE',  ( 164.2231345125756263, 250.0000000000000568, 22.80382896337009058 ) ) ;
#69644 = CARTESIAN_POINT ( 'NONE',  ( -86.00146978956946953, -287.7258796923047157, -327.5018115565001153 ) ) ;
#69645 = CARTESIAN_POINT ( 'NONE',  ( -82.44901704040604784, -299.0249896612597809, -211.8859753007576785 ) ) ;
#69646 = CARTESIAN_POINT ( 'NONE',  ( 19.35856810201305933, -283.6789760886103409, -321.6604785047875339 ) ) ;
#69648 = CARTESIAN_POINT ( 'NONE',  ( -45.63946840315497155, -283.1601082332524015, -342.9389832821836421 ) ) ;
#69647 = CARTESIAN_POINT ( 'NONE',  ( -9.833932772768598340, -296.4149801694295547, -195.0151364894189783 ) ) ;
#69649 = CARTESIAN_POINT ( 'NONE',  ( -11.29854073748852983, -275.8233962234209002, -201.4798387571367755 ) ) ;
#69650 = CARTESIAN_POINT ( 'NONE',  ( 20.41383522160819908, -282.8919155608105029, -222.5145006621147559 ) ) ;
#69651 = CARTESIAN_POINT ( 'NONE',  ( -63.15120139018820566, -296.7664372253938723, -201.7707785825902533 ) ) ;
#69652 = ORIENTED_EDGE ( 'NONE', *, *, #48217, .T. ) ;
#69653 = DIRECTION ( 'NONE',  ( 0.000000000000000000, 0.000000000000000000, -1.000000000000000000 ) ) ;
#69654 = CARTESIAN_POINT ( 'NONE',  ( 38.85221289968654901, -293.2420205778114450, -258.8907986452902037 ) ) ;
#69655 = CARTESIAN_POINT ( 'NONE',  ( -92.75890472143657917, -287.2330847048267515, -220.2773359872066123 ) ) ;
#69656 = DIRECTION ( 'NONE',  ( 0.8043439146810466012, 0.5941640067486159138, 0.000000000000000000 ) ) ;
#69657 = CARTESIAN_POINT ( 'NONE',  ( -88.47809603358389552, -276.9094976428775681, -206.1857440867352693 ) ) ;
#69658 = CARTESIAN_POINT ( 'NONE',  ( -39.96769553396496377, -276.2814976625704162, -347.1677955074182478 ) ) ;
#69659 = CARTESIAN_POINT ( 'NONE',  ( -74.05989551024291018, -287.9314525458897265, -337.1458795477659578 ) ) ;
#69660 = CARTESIAN_POINT ( 'NONE',  ( -96.46654373640500069, -285.4610387780812175, -314.3493052856666736 ) ) ;
#69661 = CARTESIAN_POINT ( 'NONE',  ( -10.87097574100657305, -278.4623477457084277, -339.4789504429181761 ) ) ;
#69662 = CARTESIAN_POINT ( 'NONE',  ( -112.9075141173978807, -286.1246398783594032, -258.6796739838415533 ) ) ;
#69663 = CARTESIAN_POINT ( 'NONE',  ( -13.41434335112037068, -281.5294584854959794, -339.8024156860477660 ) ) ;
#69664 = CARTESIAN_POINT ( 'NONE',  ( -11.06568240610275566, -282.3946609979960840, -200.0596991083561136 ) ) ;
#69665 = CARTESIAN_POINT ( 'NONE',  ( 38.21833966048116338, -275.5334665654639821, -255.5394989186387988 ) ) ;
#69666 = CARTESIAN_POINT ( 'NONE',  ( -95.21219350160868089, -277.6981114264448820, -321.1548774538080124 ) ) ;
#69667 = CARTESIAN_POINT ( 'NONE',  ( -9.937575162064501200, -296.6116357512788682, -339.5733144029186974 ) ) ;
#69668 = CARTESIAN_POINT ( 'NONE',  ( 83.14890176555634582, -299.5541904835127980, -195.3611179825600175 ) ) ;
#69669 = LINE ( 'NONE', #54994, #32975 ) ;
#69670 = CARTESIAN_POINT ( 'NONE',  ( -76.46503071634499804, -293.7087191088846794, -335.3041377022019560 ) ) ;
#69671 = CARTESIAN_POINT ( 'NONE',  ( 34.90344917153469595, -274.9151353466790511, -259.3852983307261866 ) ) ;
#69672 = CARTESIAN_POINT ( 'NONE',  ( -54.53927079543026935, -298.9158327376727016, -195.6233358906989395 ) ) ;
#69673 = AXIS2_PLACEMENT_3D ( 'NONE', #13909, #50338, #50815 ) ;
#69674 = CARTESIAN_POINT ( 'NONE',  ( -14.27112801539373166, -288.1154670088683929, -199.9815374597773427 ) ) ;
#69675 = CARTESIAN_POINT ( 'NONE',  ( 36.74410336956815115, -294.8415629840635006, -252.0854107412757230 ) ) ;
#69676 = CARTESIAN_POINT ( 'NONE',  ( -8.523104641325943476, -295.8884375453536677, -341.3926425442357413 ) ) ;
#69677 = CARTESIAN_POINT ( 'NONE',  ( -99.62271437473184221, -291.9902192122026463, -311.8706216163864724 ) ) ;
#69678 = CARTESIAN_POINT ( 'NONE',  ( -52.16623650159320391, -277.8619052757045438, -196.9578252153829112 ) ) ;
#69679 = CARTESIAN_POINT ( 'NONE',  ( -82.17425835166110915, -281.3558445059095448, -210.8711644329430328 ) ) ;
#69680 = CARTESIAN_POINT ( 'NONE',  ( -95.92148516596157037, -293.9968807049316979, -316.2928389022232523 ) ) ;
#69681 = CARTESIAN_POINT ( 'NONE',  ( -47.07385096831357174, -285.0349398392034459, -345.4982640485495722 ) ) ;
#69682 = CARTESIAN_POINT ( 'NONE',  ( -17.07327560764743524, -285.2402436463423214, -199.8565208904225869 ) ) ;
#69683 = CARTESIAN_POINT ( 'NONE',  ( 140.7145785738311190, 179.0119726656982948, -240.7059938076026810 ) ) ;
#69684 = EDGE_LOOP ( 'NONE', ( #59926, #21444, #74825, #65100 ) ) ;
#69685 = CARTESIAN_POINT ( 'NONE',  ( -106.5509906701777254, -284.5299675815555815, -246.9184543612367975 ) ) ;
#69686 = ORIENTED_EDGE ( 'NONE', *, *, #43760, .T. ) ;
#69687 = CARTESIAN_POINT ( 'NONE',  ( 30.80877462431995184, -283.0869971024856682, -305.5322041175897425 ) ) ;
#69688 = CARTESIAN_POINT ( 'NONE',  ( -87.35087383678710182, -273.6650275178095626, -217.0831439453279472 ) ) ;
#69689 = CARTESIAN_POINT ( 'NONE',  ( 21.79348265963942310, -285.6894941389752489, -221.6678034844456704 ) ) ;
#69690 = CARTESIAN_POINT ( 'NONE',  ( -42.42647329689301472, -280.9307424363087193, -193.7649999679019004 ) ) ;
#69691 = FACE_OUTER_BOUND ( 'NONE', #71469, .T. ) ;
#69692 = CARTESIAN_POINT ( 'NONE',  ( -96.29425163230303042, -280.7291436615811335, -221.8918057071531393 ) ) ;
#69693 = CARTESIAN_POINT ( 'NONE',  ( 10.75278474919325333, -281.3482827075806085, -210.2909291872242932 ) ) ;
#69694 = CARTESIAN_POINT ( 'NONE',  ( 27.33386217378598815, -279.4809262143061233, -301.5434626090942629 ) ) ;
#69695 = CARTESIAN_POINT ( 'NONE',  ( -30.22131228085657639, -124.8493855615479333, -364.3862406674347199 ) ) ;
#69696 = ORIENTED_EDGE ( 'NONE', *, *, #42665, .F. ) ;
#69697 = CARTESIAN_POINT ( 'NONE',  ( -86.53402864263458127, -275.3675513896361053, -213.8992736380239990 ) ) ;
#69698 = CARTESIAN_POINT ( 'NONE',  ( 120.9473390240897288, 149.8309046525662893, -263.2900624566332226 ) ) ;
#69699 = CARTESIAN_POINT ( 'NONE',  ( -65.41177754630301422, -277.7034775900432351, -201.1952480933589413 ) ) ;
#69700 = CARTESIAN_POINT ( 'NONE',  ( 38.69757052014190890, -295.3113703493651769, -270.2882595025219530 ) ) ;
#69701 = CARTESIAN_POINT ( 'NONE',  ( -45.10980184938776461, -294.5015661975689341, -343.0996922841786727 ) ) ;
#69702 = CARTESIAN_POINT ( 'NONE',  ( -58.91541727020166519, -291.2879546567882016, -196.5092281506078677 ) ) ;
#69703 = DIRECTION ( 'NONE',  ( -1.000000000000000000, 0.000000000000000000, -0.000000000000000000 ) ) ;
#69705 = CARTESIAN_POINT ( 'NONE',  ( 35.30564598893961659, -286.1215541422685646, -283.3535588046161138 ) ) ;
#69704 = CARTESIAN_POINT ( 'NONE',  ( -109.2898969542203673, -295.4541939790075844, -244.6305279094046909 ) ) ;
#69706 = CARTESIAN_POINT ( 'NONE',  ( 20.28998939379037836, -294.7613150818826284, -223.5494216139058210 ) ) ;
#69707 = CARTESIAN_POINT ( 'NONE',  ( -91.09077897360390352, -285.1513321543326356, -320.4837675685347449 ) ) ;
#69708 = EDGE_LOOP ( 'NONE', ( #56078, #56671, #13267, #90871 ) ) ;
#69709 = CARTESIAN_POINT ( 'NONE',  ( -101.4939421476263703, -292.0503621357454449, -228.1075531587300702 ) ) ;
#69710 = CARTESIAN_POINT ( 'NONE',  ( -26.72764481270809966, -283.4059881267299943, -342.6989074079527882 ) ) ;
#69711 = CARTESIAN_POINT ( 'NONE',  ( -97.96965203886895779, -294.7188887277228559, -317.1826959917278259 ) ) ;
#69712 = CARTESIAN_POINT ( 'NONE',  ( -78.04218483948140772, -290.3868880944109492, -335.5970198268556715 ) ) ;
#69713 = CARTESIAN_POINT ( 'NONE',  ( -70.87655904692489628, -292.1138578350687567, -201.1156116959616895 ) ) ;
#69714 = CARTESIAN_POINT ( 'NONE',  ( 18.66039553679151197, -287.0539705062516305, -223.5146725238399767 ) ) ;
#69715 = ORIENTED_EDGE ( 'NONE', *, *, #70808, .F. ) ;
#69716 = DIRECTION ( 'NONE',  ( -0.000000000000000000, -1.000000000000000000, -0.000000000000000000 ) ) ;
#69717 = CARTESIAN_POINT ( 'NONE',  ( -71.49567081594838669, -297.3588689817902377, -337.9910800560779194 ) ) ;
#69718 = CARTESIAN_POINT ( 'NONE',  ( -96.95151132392916793, -295.8838805124827331, -222.4031292392906494 ) ) ;
#69719 = CARTESIAN_POINT ( 'NONE',  ( -24.82442774050839063, -279.2745142269370717, -198.2034687728357483 ) ) ;
#69720 = ORIENTED_EDGE ( 'NONE', *, *, #42294, .F. ) ;
#69721 = CARTESIAN_POINT ( 'NONE',  ( -15.78858267145959893, -273.8312352855726886, -196.4479173958833371 ) ) ;
#69722 = CARTESIAN_POINT ( 'NONE',  ( -67.08155842100754285, -296.1349592835214253, -202.9214354106515259 ) ) ;
#69723 = CARTESIAN_POINT ( 'NONE',  ( -6.981167555458131169, -278.5098615126699997, -338.1040404523436678 ) ) ;
#69724 = CARTESIAN_POINT ( 'NONE',  ( 20.83809819108577699, -273.0515670545426019, -224.2324558410964528 ) ) ;
#69725 = CARTESIAN_POINT ( 'NONE',  ( 8.488007922102811520, -295.6137809593959673, -327.7567921259814057 ) ) ;
#69726 = CARTESIAN_POINT ( 'NONE',  ( -70.62010500271038893, -298.6822962338720231, -205.0265995652705158 ) ) ;
#69727 = CARTESIAN_POINT ( 'NONE',  ( -23.40286736638519471, -135.2391364535880598, -21.50000000000000000 ) ) ;
#69728 = CARTESIAN_POINT ( 'NONE',  ( -65.26799606271249843, -299.2934514397364865, -199.4064600910867568 ) ) ;
#69729 = CARTESIAN_POINT ( 'NONE',  ( -62.21381125162950099, -295.7292613181587058, -199.4287099186476269 ) ) ;
#69730 = CARTESIAN_POINT ( 'NONE',  ( -75.03927471209844668, -292.1873619957120241, -207.6698719003199471 ) ) ;
#69731 = CARTESIAN_POINT ( 'NONE',  ( -99.34794368747793669, -288.5831111782462699, -309.9919226229670244 ) ) ;
#69732 = CARTESIAN_POINT ( 'NONE',  ( 208.2607500777332064, 30.15285273545742228, 15.07857486252943069 ) ) ;
#69733 = CARTESIAN_POINT ( 'NONE',  ( -29.85111695228361484, -274.6369201365360482, -193.7881588725065285 ) ) ;
#69734 = EDGE_CURVE ( 'NONE', #1176, #39726, #50334, .T. ) ;
#69735 = CARTESIAN_POINT ( 'NONE',  ( -108.1964937790721848, -297.1189531061372691, -252.6552924405738167 ) ) ;
#69736 = EDGE_CURVE ( 'NONE', #34073, #23241, #62447, .T. ) ;
#69737 = CARTESIAN_POINT ( 'NONE',  ( -25.67563479675024496, -282.1799768831593269, -195.9144275247023472 ) ) ;
#69738 = CARTESIAN_POINT ( 'NONE',  ( 28.86823909258136922, -279.7352672738903721, -232.0265093353434622 ) ) ;
#69739 = CARTESIAN_POINT ( 'NONE',  ( -20.15696530941892561, -276.1856649388651590, -345.3690662258242128 ) ) ;
#69740 = CARTESIAN_POINT ( 'NONE',  ( 30.48040363235761774, -281.1159244179107191, -297.7976623725783725 ) ) ;
#69741 = CARTESIAN_POINT ( 'NONE',  ( 30.72124011757808049, -279.9718200221510642, -302.3813783619380615 ) ) ;
#69742 = CARTESIAN_POINT ( 'NONE',  ( -79.17523822138906553, -272.0504809732748868, -209.7572605347168349 ) ) ;
#69743 = CARTESIAN_POINT ( 'NONE',  ( -107.8859270491339544, -280.2204198855991990, -295.9764994671540421 ) ) ;
#69744 = DIRECTION ( 'NONE',  ( 1.000000000000000000, 0.000000000000000000, 0.000000000000000000 ) ) ;
#69745 = DIRECTION ( 'NONE',  ( -0.3024135303179443235, -0.9531768234071985590, 0.000000000000000000 ) ) ;
#69746 = CARTESIAN_POINT ( 'NONE',  ( -111.0392422152190335, -271.1993468556269136, -250.7915491121219134 ) ) ;
#69747 = VECTOR ( 'NONE', #36372, 1000.000000000000000 ) ;
#69748 = CARTESIAN_POINT ( 'NONE',  ( 34.32260354411413061, -277.8442825706679855, -293.0383313444550026 ) ) ;
#69749 = CARTESIAN_POINT ( 'NONE',  ( -63.99428340552925931, -271.7044068883166688, -200.2427601859610888 ) ) ;
#69750 = DIRECTION ( 'NONE',  ( -0.000000000000000000, 1.000000000000000000, -0.000000000000000000 ) ) ;
#69751 = CARTESIAN_POINT ( 'NONE',  ( -96.03801923425133680, -285.8217034560387901, -317.9635441034330938 ) ) ;
#69752 = ORIENTED_EDGE ( 'NONE', *, *, #75074, .F. ) ;
#69753 = CARTESIAN_POINT ( 'NONE',  ( 203.5977283565847813, 62.01285785379745619, 6.999999999999999112 ) ) ;
#69754 = CARTESIAN_POINT ( 'NONE',  ( 36.49117538660233606, -285.7248481210004911, -283.8235244442412863 ) ) ;
#69755 = CARTESIAN_POINT ( 'NONE',  ( 206.0205385567603571, 30.15663536185482485, 14.00000000000000000 ) ) ;
#69756 = CARTESIAN_POINT ( 'NONE',  ( 33.82734164008455480, -292.5826543758534513, -288.3082068760462562 ) ) ;
#69757 = CARTESIAN_POINT ( 'NONE',  ( 29.32684438253895465, -286.1266864253406084, -303.0133866673531884 ) ) ;
#69758 = CARTESIAN_POINT ( 'NONE',  ( 0.9968329295543288948, -56.25428601379442028, -352.6033083298257225 ) ) ;
#69759 = CARTESIAN_POINT ( 'NONE',  ( -89.92166824827005200, -293.7939382230401861, -323.9163461860904931 ) ) ;
#69760 = CARTESIAN_POINT ( 'NONE',  ( -103.4301990598390404, -283.5336362849516263, -232.1113863837517499 ) ) ;
#69761 = CARTESIAN_POINT ( 'NONE',  ( -37.02512560537597608, -281.6563111726727584, -196.5617941490830844 ) ) ;
#69762 = CARTESIAN_POINT ( 'NONE',  ( 38.39067834454567674, -288.6113591915424195, -258.7580135312788343 ) ) ;
#69763 = CARTESIAN_POINT ( 'NONE',  ( 25.08486774103853634, -280.3722526985122840, -313.7071694180844474 ) ) ;
#69764 = CARTESIAN_POINT ( 'NONE',  ( -98.84176588497294347, -290.0081536835057250, -309.6897578255295116 ) ) ;
#69765 = CARTESIAN_POINT ( 'NONE',  ( -41.09927852052798158, -281.4292099863754970, -196.8678834459775260 ) ) ;
#69766 = CARTESIAN_POINT ( 'NONE',  ( -49.17808029720806928, -280.7002758255341064, -198.1634599108560906 ) ) ;
#69767 = CARTESIAN_POINT ( 'NONE',  ( 35.20785125506043300, -289.7934350737350542, -290.7792948705354661 ) ) ;
#69768 = EDGE_CURVE ( 'NONE', #17873, #64817, #24647, .T. ) ;
#69769 = VERTEX_POINT ( 'NONE', #6643 ) ;
#69770 = CARTESIAN_POINT ( 'NONE',  ( -114.3417001280813849, -272.5880137785256352, -267.4936526912260319 ) ) ;
#69771 = CARTESIAN_POINT ( 'NONE',  ( -73.12569881047713238, -291.5089085225822600, -335.8695315084829645 ) ) ;
#69772 = CARTESIAN_POINT ( 'NONE',  ( 157.4851178187871312, 1.000000000000000888, -7.000000000000000888 ) ) ;
#69773 = CARTESIAN_POINT ( 'NONE',  ( -2.602324593224680793, -297.1233781216987495, -342.4248175857292154 ) ) ;
#69774 = VERTEX_POINT ( 'NONE', #15127 ) ;
#69775 = CARTESIAN_POINT ( 'NONE',  ( 15.64437633638226721, -274.3048549049173062, -323.7489116557920283 ) ) ;
#69776 = FACE_OUTER_BOUND ( 'NONE', #12896, .T. ) ;
#69777 = CARTESIAN_POINT ( 'NONE',  ( -58.64738260790357316, -293.7229202153291112, -343.5769557234759759 ) ) ;
#69778 = CARTESIAN_POINT ( 'NONE',  ( -102.5844659797832179, -296.5071070721870683, -237.3643002194833116 ) ) ;
#69779 = CARTESIAN_POINT ( 'NONE',  ( 14.58552900387998719, -289.8249363724557952, -322.6513716293845846 ) ) ;
#69780 = CARTESIAN_POINT ( 'NONE',  ( 10.58165542477711973, -284.1400506273893143, -326.8317791075056675 ) ) ;
#69781 = CARTESIAN_POINT ( 'NONE',  ( -91.17045695381112580, -291.2239468179803907, -324.6671753163211065 ) ) ;
#69782 = CARTESIAN_POINT ( 'NONE',  ( -104.7137327352939735, -291.3955604553779040, -306.6144970512342525 ) ) ;
#69783 = CARTESIAN_POINT ( 'NONE',  ( -72.12786754061581007, -287.5921755839538605, -203.9162294783904770 ) ) ;
#69784 = CARTESIAN_POINT ( 'NONE',  ( -8.863084547796210799, -280.5812610166687477, -198.8211399343347807 ) ) ;
#69785 = CARTESIAN_POINT ( 'NONE',  ( -101.8982269055259593, -294.1095378964258771, -309.6264849986258128 ) ) ;
#69786 = CARTESIAN_POINT ( 'NONE',  ( -41.57126057071925374, -282.9372209981283390, -347.2971932153177477 ) ) ;
#69787 = CARTESIAN_POINT ( 'NONE',  ( 14.33988895547520492, -276.6485737450211673, -217.0706044863480315 ) ) ;
#69788 = CARTESIAN_POINT ( 'NONE',  ( 34.45848030099739390, -284.0519495502702512, -270.3284710469131937 ) ) ;
#69789 = CARTESIAN_POINT ( 'NONE',  ( 37.73100448102987770, -273.9451015590176439, -282.4407652439108460 ) ) ;
#69790 = CARTESIAN_POINT ( 'NONE',  ( 165.0427047786672290, 275.5000000000000568, 23.37680765314704701 ) ) ;
#69791 = CARTESIAN_POINT ( 'NONE',  ( -7.968956325360199600, -279.9552851650930734, -203.4502708190228759 ) ) ;
#69792 = CARTESIAN_POINT ( 'NONE',  ( -113.3701832252194919, -279.6342411833419419, -280.1440915724574552 ) ) ;
#69793 = CARTESIAN_POINT ( 'NONE',  ( -57.68201391988490911, -284.8546305326102015, -196.2850499678423262 ) ) ;
#69794 = CARTESIAN_POINT ( 'NONE',  ( 20.96755605993838856, -294.6782807176982146, -224.7554711247354362 ) ) ;
#69795 = CARTESIAN_POINT ( 'NONE',  ( 36.46896285214925371, -277.3916859713029908, -289.2932717934054949 ) ) ;
#69796 = CARTESIAN_POINT ( 'NONE',  ( -46.83650365200139021, -275.2491525289918286, -194.4457244313477418 ) ) ;
#69797 = CARTESIAN_POINT ( 'NONE',  ( 201.2104617360081704, 60.19600395700749829, 10.00000000000000000 ) ) ;
#69798 = CARTESIAN_POINT ( 'NONE',  ( 9.662428170168167796, -276.2172169285096288, -326.2146042426433041 ) ) ;
#69799 = CARTESIAN_POINT ( 'NONE',  ( -81.20940412451946600, -297.6500928145194393, -330.9882816124076612 ) ) ;
#69800 = CARTESIAN_POINT ( 'NONE',  ( -84.79114728922037614, -283.3965685785242954, -212.4269057746222131 ) ) ;
#69801 = CARTESIAN_POINT ( 'NONE',  ( 39.69046493787777052, -293.2182848010341445, -270.3142089617036845 ) ) ;
#69802 = CARTESIAN_POINT ( 'NONE',  ( 36.47184717657550124, -273.4278304277079314, -259.1660536005069275 ) ) ;
#69803 = CARTESIAN_POINT ( 'NONE',  ( 37.99155650847939825, -289.0063480829616083, -258.8139895386072453 ) ) ;
#69804 = CARTESIAN_POINT ( 'NONE',  ( -37.53702834384171894, -290.9700129800380637, -197.0397683845907579 ) ) ;
#69805 = ORIENTED_EDGE ( 'NONE', *, *, #47697, .F. ) ;
#69806 = CARTESIAN_POINT ( 'NONE',  ( -61.48506261730522482, -290.3194146842748751, -197.8091588838541952 ) ) ;
#69807 = CARTESIAN_POINT ( 'NONE',  ( -110.1440873523407049, -290.1362289151088021, -276.6274992141105713 ) ) ;
#69808 = ORIENTED_EDGE ( 'NONE', *, *, #33448, .F. ) ;
#69809 = CARTESIAN_POINT ( 'NONE',  ( 21.84282116196428092, -287.9738715971319607, -221.5893541155373043 ) ) ;
#69810 = CARTESIAN_POINT ( 'NONE',  ( -107.8395674423771453, -278.6341407871074694, -289.3910468046250912 ) ) ;
#69811 = CARTESIAN_POINT ( 'NONE',  ( -90.50773146999405583, -294.7039969918437805, -325.7050836276022210 ) ) ;
#69812 = CARTESIAN_POINT ( 'NONE',  ( -2.276798263768706754, -287.1552592888003232, -201.9083446490197389 ) ) ;
#69813 = CARTESIAN_POINT ( 'NONE',  ( 26.33748730263272719, -287.3147461526577331, -227.0859209131998568 ) ) ;
#69814 = CARTESIAN_POINT ( 'NONE',  ( -1.237861536918885674, -282.8922144017213895, -333.8323738846017932 ) ) ;
#69815 = CARTESIAN_POINT ( 'NONE',  ( -84.14657331821624098, -219.4986398962294913, -352.5341896374943644 ) ) ;
#69816 = AXIS2_PLACEMENT_3D ( 'NONE', #1245, #75890, #30127 ) ;
#69817 = CARTESIAN_POINT ( 'NONE',  ( 23.98614183410543532, -22.50930313572179031, -343.8471797293080954 ) ) ;
#69818 = CARTESIAN_POINT ( 'NONE',  ( -94.70623550478640595, -238.3196911832316687, -338.6262115470744334 ) ) ;
#69819 = CIRCLE ( 'NONE', #25934, 5.654241149514405151 ) ;
#69820 = CARTESIAN_POINT ( 'NONE',  ( 35.51388148748905138, -274.8372838068893316, -277.0443772284637589 ) ) ;
#69821 = CARTESIAN_POINT ( 'NONE',  ( 33.53755888985122624, -274.7186001613494568, -289.0789361095579579 ) ) ;
#69822 = CARTESIAN_POINT ( 'NONE',  ( -57.36765198758669015, -297.3082056036287781, -196.0193574158977867 ) ) ;
#69823 = CARTESIAN_POINT ( 'NONE',  ( 7.158040960647978679, -59.91464807905658319, -351.6596033274320234 ) ) ;
#69824 = CARTESIAN_POINT ( 'NONE',  ( 21.48249569608899989, -273.5748194817562080, -221.4426934365206705 ) ) ;
#69825 = CARTESIAN_POINT ( 'NONE',  ( -27.17283030142132816, -275.9431733507386184, -196.9980682311274904 ) ) ;
#69826 = ORIENTED_EDGE ( 'NONE', *, *, #9644, .T. ) ;
#69827 = CARTESIAN_POINT ( 'NONE',  ( -112.0739693511602724, -297.2725598971451859, -287.9652485549684116 ) ) ;
#69828 = CARTESIAN_POINT ( 'NONE',  ( 1.349481396886883289, -289.0122455190566484, -332.3367657308255048 ) ) ;
#69829 = CARTESIAN_POINT ( 'NONE',  ( -109.2827416163746364, -297.0111148477424194, -297.5046112250822716 ) ) ;
#69830 = CARTESIAN_POINT ( 'NONE',  ( -113.0796440280699642, -297.2139501283534173, -256.8226262959033761 ) ) ;
#69831 = CARTESIAN_POINT ( 'NONE',  ( 24.84675797149762744, -293.1906821969593011, -232.0343378902414031 ) ) ;
#69832 = EDGE_LOOP ( 'NONE', ( #53142, #85059, #21411, #84841 ) ) ;
#69833 = CARTESIAN_POINT ( 'NONE',  ( 34.69726164150895187, -277.7642890607971253, -293.1580955276006648 ) ) ;
#69834 = EDGE_CURVE ( 'NONE', #41591, #12908, #50656, .T. ) ;
#69835 = VERTEX_POINT ( 'NONE', #87533 ) ;
#69836 = CARTESIAN_POINT ( 'NONE',  ( 17.18392958689692662, -280.3120479773417628, -216.0048937307164181 ) ) ;
#69837 = CARTESIAN_POINT ( 'NONE',  ( -68.12544915272330570, -278.4078514846190728, -336.8261632510392474 ) ) ;
#69838 = CARTESIAN_POINT ( 'NONE',  ( -35.71049021314031080, -278.7921205503171223, -346.3432279159363247 ) ) ;
#69839 = CARTESIAN_POINT ( 'NONE',  ( -93.99130473467940305, -275.8851922394803751, -320.0524562882885675 ) ) ;
#69840 = CARTESIAN_POINT ( 'NONE',  ( -70.52121750823587831, -298.2541073234322653, -205.2087775785396389 ) ) ;
#69841 = CARTESIAN_POINT ( 'NONE',  ( -110.9739623088040190, -295.1125720020813787, -271.4538989148142605 ) ) ;
#69842 = DIRECTION ( 'NONE',  ( 0.6056179655966478226, -0.7957555401921982963, 0.000000000000000000 ) ) ;
#69843 = CARTESIAN_POINT ( 'NONE',  ( -4.975584933748663730, -280.9593298086963955, -200.5616803720582766 ) ) ;
#69844 = EDGE_CURVE ( 'NONE', #65957, #62648, #14498, .T. ) ;
#69845 = CARTESIAN_POINT ( 'NONE',  ( -107.8197076371699978, -278.4675665788223569, -289.3834853975744750 ) ) ;
#69846 = CARTESIAN_POINT ( 'NONE',  ( 32.40837223325540606, -286.6411257774357182, -301.7971749401472152 ) ) ;
#69847 = CARTESIAN_POINT ( 'NONE',  ( -36.58988087788193155, -300.0616984865663426, -195.1941870151826492 ) ) ;
#69848 = DIRECTION ( 'NONE',  ( 8.659560562354797273E-17, -0.7071067811865584529, 0.7071067811865364705 ) ) ;
#69849 = CARTESIAN_POINT ( 'NONE',  ( -108.5098687401455777, -289.5260411048391802, -287.3226481003029562 ) ) ;
#69850 = CARTESIAN_POINT ( 'NONE',  ( -62.63445947834218686, -277.9584268299190626, -200.7494947566690939 ) ) ;
#69852 = CARTESIAN_POINT ( 'NONE',  ( -62.03502070899428844, -281.4554058552522520, -340.6404367515655736 ) ) ;
#69851 = CARTESIAN_POINT ( 'NONE',  ( -16.73950341344101389, -278.8982833906938481, -199.7146431497733090 ) ) ;
#69853 = CARTESIAN_POINT ( 'NONE',  ( 35.13370030931157117, -289.3020423786359743, -250.8717609994892257 ) ) ;
#69854 = CARTESIAN_POINT ( 'NONE',  ( -110.2969430991380051, -279.6458451373547405, -278.8509030828682853 ) ) ;
#69855 = CARTESIAN_POINT ( 'NONE',  ( 196.9534188175200029, 25.84350552936208700, 12.42857142857141817 ) ) ;
#69856 = CARTESIAN_POINT ( 'NONE',  ( 16.04752219468317520, -294.8088544809635323, -217.6136231182229039 ) ) ;
#69857 = CARTESIAN_POINT ( 'NONE',  ( -95.38978219616744525, -276.1224197385801631, -319.4158308149458207 ) ) ;
#69858 = CARTESIAN_POINT ( 'NONE',  ( 7.649648561228860721, -277.0710919898075417, -328.0422134411126081 ) ) ;
#69859 = CARTESIAN_POINT ( 'NONE',  ( -34.52162790334747200, -285.0169364510393279, -345.4748691988879727 ) ) ;
#69860 = DIRECTION ( 'NONE',  ( 0.000000000000000000, 0.000000000000000000, 1.000000000000000000 ) ) ;
#69861 = CARTESIAN_POINT ( 'NONE',  ( -110.9207199349052360, -292.6913679100433114, -253.1726902823849912 ) ) ;
#69862 = CARTESIAN_POINT ( 'NONE',  ( -50.59282230630184074, -293.2210865090200969, -344.2334130830394656 ) ) ;
#69863 = CARTESIAN_POINT ( 'NONE',  ( 1.449007683615202380, -285.7538595798659458, -204.0175376582806734 ) ) ;
#69864 = DIRECTION ( 'NONE',  ( 1.000000000000000000, 0.000000000000000000, 0.000000000000000000 ) ) ;
#69865 = CARTESIAN_POINT ( 'NONE',  ( -56.97736901219635541, -272.4784976865049089, -199.4865550070201436 ) ) ;
#69866 = CARTESIAN_POINT ( 'NONE',  ( -0.6254859487067386814, -290.6850126336611311, -205.8267465246558743 ) ) ;
#69867 = FACE_OUTER_BOUND ( 'NONE', #35128, .T. ) ;
#69868 = CARTESIAN_POINT ( 'NONE',  ( 189.9243309297870610, 215.0000000000000568, 20.22542485937349355 ) ) ;
#69869 = CARTESIAN_POINT ( 'NONE',  ( -98.63600406859396230, -289.6420105566908774, -224.8890871053053786 ) ) ;
#69870 = CARTESIAN_POINT ( 'NONE',  ( -71.56712800353275838, -287.1922081489394714, -204.9771711487841799 ) ) ;
#69871 = CARTESIAN_POINT ( 'NONE',  ( 38.59052326206262507, -285.8430928982788828, -274.3918300862579827 ) ) ;
#69872 = CARTESIAN_POINT ( 'NONE',  ( -105.7550710406451913, -285.6160272760651537, -297.6103601237347789 ) ) ;
#69873 = CARTESIAN_POINT ( 'NONE',  ( -74.94434090351494149, -280.8906705383787994, 27.50000000000000000 ) ) ;
#69874 = CARTESIAN_POINT ( 'NONE',  ( -101.1371230449171890, -285.8451928693472155, -234.4418291461244337 ) ) ;
#69875 = CARTESIAN_POINT ( 'NONE',  ( 18.18621742184801349, -294.8238034799593947, -219.4194142803737861 ) ) ;
#69876 = CARTESIAN_POINT ( 'NONE',  ( 17.83465341282682814, -274.3495558591986310, -321.9836344663979730 ) ) ;
#69877 = CARTESIAN_POINT ( 'NONE',  ( 31.83814585659040830, -276.3204113725470279, -304.2448489721358555 ) ) ;
#69878 = CIRCLE ( 'NONE', #272, 0.5000000000000004441 ) ;
#69879 = CARTESIAN_POINT ( 'NONE',  ( -58.51136796910393656, -289.8603776747629581, -197.8272682355132019 ) ) ;
#69880 = CARTESIAN_POINT ( 'NONE',  ( -69.96237619135595764, -279.6343191865573772, -200.5979545221962042 ) ) ;
#69881 = CARTESIAN_POINT ( 'NONE',  ( -76.49991774877359774, -297.5582207467612079, -333.9704102226644977 ) ) ;
#69882 = CARTESIAN_POINT ( 'NONE',  ( 208.6208076322478746, 32.98517505407394168, 10.00000000000000000 ) ) ;
#69883 = CARTESIAN_POINT ( 'NONE',  ( 129.8975571001389540, -299.5541904835127980, -195.3611179825600175 ) ) ;
#69884 = CARTESIAN_POINT ( 'NONE',  ( -6.796362452137638677, -285.1465249386672554, -203.5025076557707564 ) ) ;
#69885 = CARTESIAN_POINT ( 'NONE',  ( 17.70989211536642927, -278.8397325102552031, -219.4266223947996650 ) ) ;
#69886 = CARTESIAN_POINT ( 'NONE',  ( 150.6539576904058606, 293.9636489450775230, 9.103929867429224387 ) ) ;
#69887 = CARTESIAN_POINT ( 'NONE',  ( 36.96423561809814373, -273.8123132421795276, -252.9451924945206827 ) ) ;
#69888 = CARTESIAN_POINT ( 'NONE',  ( -100.6752867818674986, -277.3996614920042703, -306.9696441423736246 ) ) ;
#69889 = AXIS2_PLACEMENT_3D ( 'NONE', #76746, #91869, #55912 ) ;
#69890 = CARTESIAN_POINT ( 'NONE',  ( -15.36780548047465089, -296.2827437851610171, -340.7557947926619022 ) ) ;
#69891 = CARTESIAN_POINT ( 'NONE',  ( 37.83979153515001315, -280.6626022124785891, -285.5016537083496928 ) ) ;
#69892 = CARTESIAN_POINT ( 'NONE',  ( -5.428173927389670972, -295.5629120734810158, -336.2910976143267021 ) ) ;
#69893 = CARTESIAN_POINT ( 'NONE',  ( -68.01300627710857327, -296.7616748436985858, -340.4508408597426410 ) ) ;
#69894 = CARTESIAN_POINT ( 'NONE',  ( -60.51388748766771641, -297.5765301800841485, -201.0830169799158682 ) ) ;
#69895 = CARTESIAN_POINT ( 'NONE',  ( -91.27168227241885745, -293.2853276991085067, -218.2405109806711039 ) ) ;
#69896 = CARTESIAN_POINT ( 'NONE',  ( -68.50270329652708767, -285.8205997747404581, -199.9337321232605404 ) ) ;
#69897 = CARTESIAN_POINT ( 'NONE',  ( 37.27975156300217918, -273.5241291862529920, -257.1740976037683595 ) ) ;
#69898 = CARTESIAN_POINT ( 'NONE',  ( -41.76267913961567757, -288.9396937276749782, -347.2473194799576390 ) ) ;
#69899 = CARTESIAN_POINT ( 'NONE',  ( -111.9970392151001874, -280.5640829750805665, -267.8781502151322798 ) ) ;
#69900 = CARTESIAN_POINT ( 'NONE',  ( 22.18982810042686182, -286.0156232565913683, -227.6211106795291244 ) ) ;
#69901 = CARTESIAN_POINT ( 'NONE',  ( -110.0492601287574672, -288.7889813451972145, -251.9080641120842756 ) ) ;
#69902 = CARTESIAN_POINT ( 'NONE',  ( -47.20788896421541381, -156.8319029772612225, -362.3615984655540387 ) ) ;
#69903 = CARTESIAN_POINT ( 'NONE',  ( 35.61450233827622469, -286.9969017672466975, -265.5889255935906021 ) ) ;
#69904 = DIRECTION ( 'NONE',  ( -0.8435586647355782786, 0.000000000000000000, -0.5370370370370447510 ) ) ;
#69905 = CARTESIAN_POINT ( 'NONE',  ( -52.85829936820156405, -284.1874453095255717, -345.5955943772180490 ) ) ;
#69906 = CARTESIAN_POINT ( 'NONE',  ( -58.86120577092684414, -290.8391221403008444, -196.6744089417883856 ) ) ;
#69907 = CARTESIAN_POINT ( 'NONE',  ( 38.38533278721116204, -283.0393257420132045, -261.4233548760137751 ) ) ;
#69908 = CARTESIAN_POINT ( 'NONE',  ( 39.21686377178659200, -282.8617261796161415, -269.9163106681361910 ) ) ;
#69909 = CARTESIAN_POINT ( 'NONE',  ( 35.56581522207419965, -281.4339299176273244, -274.0345645865812685 ) ) ;
#69910 = CARTESIAN_POINT ( 'NONE',  ( 36.81545282730818514, -277.4072407561739624, -259.0625264375866550 ) ) ;
#69911 = CARTESIAN_POINT ( 'NONE',  ( -30.59095141396967676, -294.9690163808668331, -347.0646211085511368 ) ) ;
#69912 = CARTESIAN_POINT ( 'NONE',  ( -110.2751125260875114, -288.3665244729839401, -286.3128998105893857 ) ) ;
#69913 = EDGE_CURVE ( 'NONE', #74736, #2640, #52740, .T. ) ;
#69914 = CARTESIAN_POINT ( 'NONE',  ( -44.58600641714774326, -296.8787991150953189, -197.3602239962473277 ) ) ;
#69915 = ORIENTED_EDGE ( 'NONE', *, *, #69844, .T. ) ;
#69916 = ORIENTED_EDGE ( 'NONE', *, *, #48330, .T. ) ;
#69917 = CARTESIAN_POINT ( 'NONE',  ( -108.7430303059190919, -286.7475585476391871, -249.1306703359411472 ) ) ;
#69918 = CARTESIAN_POINT ( 'NONE',  ( 36.40312563877686358, -294.3663138658903904, -249.2611441561102765 ) ) ;
#69919 = CARTESIAN_POINT ( 'NONE',  ( -13.48827728622425681, -283.3856482824953105, -339.5155007035441486 ) ) ;
#69920 = CARTESIAN_POINT ( 'NONE',  ( 29.74774395412104511, -274.1245982420526275, -232.9445877546250472 ) ) ;
#69921 = CARTESIAN_POINT ( 'NONE',  ( -103.1329390377102868, -291.7249831284295851, -230.4485663156505950 ) ) ;
#69922 = CARTESIAN_POINT ( 'NONE',  ( -29.56577140520561997, -284.2892252297237405, -194.9964020195030230 ) ) ;
#69923 = CARTESIAN_POINT ( 'NONE',  ( 1.685719059630385042, -292.8919950087804409, -203.9480751310505013 ) ) ;
#69924 = CARTESIAN_POINT ( 'NONE',  ( 19.53262534828831676, -288.5327328133406581, -316.1584824098508761 ) ) ;
#69925 = DIRECTION ( 'NONE',  ( -0.000000000000000000, -1.000000000000000000, -0.000000000000000000 ) ) ;
#69926 = DIRECTION ( 'NONE',  ( 0.000000000000000000, 0.000000000000000000, -1.000000000000000000 ) ) ;
#69927 = CARTESIAN_POINT ( 'NONE',  ( 196.4392320932925600, 281.7853120024273608, -110.2283348974790869 ) ) ;
#69928 = CARTESIAN_POINT ( 'NONE',  ( -78.76694709226494240, -285.1196251605589396, -334.4443191011737895 ) ) ;
#69929 = CARTESIAN_POINT ( 'NONE',  ( 10.59707575819633618, -285.9094976428776818, -330.5268031993606428 ) ) ;
#69930 = ORIENTED_EDGE ( 'NONE', *, *, #71404, .F. ) ;
#69931 = CARTESIAN_POINT ( 'NONE',  ( 35.34111816847146059, -280.3419028635861991, -260.4210565170488962 ) ) ;
#69932 = CARTESIAN_POINT ( 'NONE',  ( 14.86572119087143129, -276.0071912240183565, -327.0033499816094036 ) ) ;
#69933 = CARTESIAN_POINT ( 'NONE',  ( -110.4020798630876641, -280.7613765721303594, -254.1094854745516329 ) ) ;
#69934 = CARTESIAN_POINT ( 'NONE',  ( -109.3818371394523439, -271.0219980206236414, -295.8620562373184271 ) ) ;
#69935 = CARTESIAN_POINT ( 'NONE',  ( 37.28609729605216927, -280.3344632765735014, -286.8317849141425881 ) ) ;
#69936 = CARTESIAN_POINT ( 'NONE',  ( -52.39657739801258884, -283.8784975105800186, -197.2502605808462590 ) ) ;
#69937 = CARTESIAN_POINT ( 'NONE',  ( -65.19176344665378053, -299.4534384573961461, -199.6058755778817613 ) ) ;
#69938 = CARTESIAN_POINT ( 'NONE',  ( 19.74577498377869844, -294.6882289870004570, -315.9772112643364608 ) ) ;
#69939 = EDGE_LOOP ( 'NONE', ( #89851, #11569, #80625, #89457 ) ) ;
#69940 = CARTESIAN_POINT ( 'NONE',  ( -62.95702436984655748, -290.3963097146722134, -201.4764415882426647 ) ) ;
#69941 = CARTESIAN_POINT ( 'NONE',  ( -42.79065688494367947, -277.7706278094759682, -347.0658874359046990 ) ) ;
#69942 = CARTESIAN_POINT ( 'NONE',  ( -38.08236020527431975, -274.0426155692717884, -197.3648754583721256 ) ) ;
#69943 = CARTESIAN_POINT ( 'NONE',  ( -112.7617452633776907, -271.6506261557143489, -256.1742905084807376 ) ) ;
#69944 = SURFACE_STYLE_FILL_AREA ( #77047 ) ;
#69945 = CARTESIAN_POINT ( 'NONE',  ( 5.292311968802505540, -272.6283614942753388, -208.5950628434527232 ) ) ;
#69946 = EDGE_CURVE ( 'NONE', #19714, #52231, #86619, .T. ) ;
#69947 = AXIS2_PLACEMENT_3D ( 'NONE', #76376, #18140, #12438 ) ;
#69948 = CARTESIAN_POINT ( 'NONE',  ( -43.54160339317392214, -248.0334966641272842, -472.6442049081569508 ) ) ;
#69949 = VECTOR ( 'NONE', #46683, 1000.000000000000000 ) ;
#69950 = CARTESIAN_POINT ( 'NONE',  ( 20.43304003651921619, -283.2651762691130557, -315.4865595157622238 ) ) ;
#69951 = CARTESIAN_POINT ( 'NONE',  ( 29.81559632849957353, -282.8457929027379123, -234.6980312739503631 ) ) ;
#69952 = CARTESIAN_POINT ( 'NONE',  ( -87.00416110652288637, -283.1139222855458684, -324.0730167631756444 ) ) ;
#69953 = CARTESIAN_POINT ( 'NONE',  ( -0.1254269126662794498, -272.9559501441321459, -206.6173338480240318 ) ) ;
#69954 = CARTESIAN_POINT ( 'NONE',  ( -27.41629240917883692, -282.0398738299962247, -196.7403753057948563 ) ) ;
#69955 = CARTESIAN_POINT ( 'NONE',  ( 33.17424939053778132, -274.3133206007054241, -291.8106313566112817 ) ) ;
#69957 = CARTESIAN_POINT ( 'NONE',  ( 207.6679626695819820, 29.67996584739399069, 14.87498546835752222 ) ) ;
#69956 = VECTOR ( 'NONE', #83118, 1000.000000000000000 ) ;
#69958 = CARTESIAN_POINT ( 'NONE',  ( 34.13206991952225877, -276.4170298106874384, -254.0039281962677080 ) ) ;
#69959 = FACE_OUTER_BOUND ( 'NONE', #22746, .T. ) ;
#69960 = AXIS2_PLACEMENT_3D ( 'NONE', #51132, #85714, #20859 ) ;
#69961 = CARTESIAN_POINT ( 'NONE',  ( -17.38995559178933803, -277.6038541676886098, -344.5641280965680266 ) ) ;
#69962 = VERTEX_POINT ( 'NONE', #58690 ) ;
#69963 = ORIENTED_EDGE ( 'NONE', *, *, #44156, .T. ) ;
#69964 = CARTESIAN_POINT ( 'NONE',  ( 197.7323754217920282, 18.47808631421187542, 11.36704352365794790 ) ) ;
#69965 = CARTESIAN_POINT ( 'NONE',  ( -64.13293707563521195, -287.5667750853426128, -199.4773295001671158 ) ) ;
#69966 = CARTESIAN_POINT ( 'NONE',  ( -95.73938617503270621, -295.1313631101084525, -314.4534279047908285 ) ) ;
#69967 = EDGE_CURVE ( 'NONE', #59928, #57748, #50597, .T. ) ;
#69968 = CARTESIAN_POINT ( 'NONE',  ( -20.52678491702211971, -288.1904135201629060, -345.4528450825957293 ) ) ;
#69969 = CARTESIAN_POINT ( 'NONE',  ( -95.74301710409903876, -283.4241212034692126, -224.8734130622021041 ) ) ;
#69971 = CARTESIAN_POINT ( 'NONE',  ( -93.19092824606018155, -288.1083717983200927, -319.0056040404932673 ) ) ;
#69970 = CARTESIAN_POINT ( 'NONE',  ( -109.2367046352238020, -283.3330946910367629, -254.6025676901048769 ) ) ;
#69972 = CARTESIAN_POINT ( 'NONE',  ( -80.84923534651552757, -284.8623111566564603, -329.5363113563394677 ) ) ;
#69973 = CARTESIAN_POINT ( 'NONE',  ( 2.419046556365148426, -274.5195751371769006, -334.0153498427671366 ) ) ;
#69974 = CARTESIAN_POINT ( 'NONE',  ( 33.12745311249031488, -285.5781770154042647, -241.2311322837780665 ) ) ;
#69975 = CARTESIAN_POINT ( 'NONE',  ( -83.99282008578568082, -299.4112751593642088, -211.6357090669144725 ) ) ;
#69976 = CARTESIAN_POINT ( 'NONE',  ( 28.73854083186291319, -286.0280141197459329, -306.2949013406263248 ) ) ;
#69977 = CARTESIAN_POINT ( 'NONE',  ( -51.88577660282197002, -280.8028444406000403, -198.5326333571745465 ) ) ;
#69978 = CARTESIAN_POINT ( 'NONE',  ( -26.38599813561156893, -290.9131880073628622, -344.7250945994023823 ) ) ;
#69979 = DIRECTION ( 'NONE',  ( 0.000000000000000000, -1.000000000000000000, 0.000000000000000000 ) ) ;
#69980 = DIRECTION ( 'NONE',  ( -1.000000000000000000, 0.000000000000000000, 0.000000000000000000 ) ) ;
#69981 = CARTESIAN_POINT ( 'NONE',  ( -63.73976035961275954, -297.3138090366653046, -341.1598228694620616 ) ) ;
#69982 = AXIS2_PLACEMENT_3D ( 'NONE', #46457, #23304, #16658 ) ;
#69983 = CARTESIAN_POINT ( 'NONE',  ( -27.26511985092312074, -278.1799192299293964, -195.9885173964854346 ) ) ;
#69984 = CARTESIAN_POINT ( 'NONE',  ( 29.34059094481437668, -292.2522505028048272, -232.1821856066808039 ) ) ;
#69985 = CARTESIAN_POINT ( 'NONE',  ( -110.8451493102328129, -295.0454339692290091, -263.2020036758684682 ) ) ;
#69986 = CARTESIAN_POINT ( 'NONE',  ( 9.604337228643641922, -279.3982695602122135, -213.7499774159815900 ) ) ;
#69987 = CARTESIAN_POINT ( 'NONE',  ( 29.15845152836323706, -273.1867841343486134, -236.9090025847019945 ) ) ;
#69988 = CARTESIAN_POINT ( 'NONE',  ( 16.53196190812811395, -295.5809594945984600, -320.3498368810196553 ) ) ;
#69989 = CARTESIAN_POINT ( 'NONE',  ( -69.91165696735023971, -294.1233781216987495, -202.8022627189028810 ) ) ;
#69990 = CARTESIAN_POINT ( 'NONE',  ( -106.5457882174293616, -294.6168630523359866, -302.5092430074454342 ) ) ;
#69991 = CARTESIAN_POINT ( 'NONE',  ( -25.16149338894066645, -290.4452738144798332, -195.3570075918393059 ) ) ;
#69992 = CARTESIAN_POINT ( 'NONE',  ( -104.5787582552584638, -291.5765062153187159, -300.3959700923375067 ) ) ;
#69993 = CARTESIAN_POINT ( 'NONE',  ( 195.0811277904324754, 27.48493576247232895, 15.19607843137254477 ) ) ;
#69994 = CARTESIAN_POINT ( 'NONE',  ( -105.8654724817034491, -291.6979189197457458, -244.5834585213102343 ) ) ;
#69995 = DIRECTION ( 'NONE',  ( -1.000000000000000000, 0.000000000000000000, 0.000000000000000000 ) ) ;
#69996 = CARTESIAN_POINT ( 'NONE',  ( -90.52138181916453163, -292.5244193230292922, -215.1519230775317055 ) ) ;
#69998 = CARTESIAN_POINT ( 'NONE',  ( 12.90315701401277337, -292.7776524292532372, -217.4040190177323666 ) ) ;
#69997 = CARTESIAN_POINT ( 'NONE',  ( 36.52807747296611041, -279.7625270273228466, -285.2494611819862484 ) ) ;
#69999 = CARTESIAN_POINT ( 'NONE',  ( 15.16133415868702983, -280.7686147112395929, -213.9638891745606486 ) ) ;
#70000 = CARTESIAN_POINT ( 'NONE',  ( -88.31071586364588200, -283.4097281426055588, -328.1202810978776370 ) ) ;
#70001 = CARTESIAN_POINT ( 'NONE',  ( -98.87046001399515660, -287.9728612838627555, -312.9775389237487389 ) ) ;
#70002 = CARTESIAN_POINT ( 'NONE',  ( -51.27253721878857107, -281.3715667942249183, -343.3299413249704344 ) ) ;
#70003 = CARTESIAN_POINT ( 'NONE',  ( -79.51135550676674768, -277.9739975718666756, -206.7019273469587688 ) ) ;
#70004 = CARTESIAN_POINT ( 'NONE',  ( -4.892191116106971549, -285.3898590538238977, -200.8735516413862285 ) ) ;
#70005 = CARTESIAN_POINT ( 'NONE',  ( 195.8476942551502020, 41.45913785700680165, 14.14010213890159484 ) ) ;
#70006 = CARTESIAN_POINT ( 'NONE',  ( 0.2997534686382283264, -294.1627103920170043, -206.8822916992624528 ) ) ;
#70007 = CARTESIAN_POINT ( 'NONE',  ( 12.33541055560685784, -277.8012915519076387, -328.4196312728062708 ) ) ;
#70008 = CARTESIAN_POINT ( 'NONE',  ( -103.1519066630730919, -277.7895283523055809, -302.1183613250405529 ) ) ;
#70009 = CARTESIAN_POINT ( 'NONE',  ( -61.69059341658992679, -291.9111105554095502, -197.2561316515332237 ) ) ;
#70010 = AXIS2_PLACEMENT_3D ( 'NONE', #63953, #36438, #58240 ) ;
#70011 = CARTESIAN_POINT ( 'NONE',  ( 20.49177049563761699, -280.2992811304096108, -318.9883107528715414 ) ) ;
#70012 = CARTESIAN_POINT ( 'NONE',  ( 32.02776521367444218, -292.2980601191121082, -246.7237024695453442 ) ) ;
#70013 = CIRCLE ( 'NONE', #82090, 2.738891987356051327 ) ;
#70014 = CARTESIAN_POINT ( 'NONE',  ( -96.63668418683886330, -295.1817193960060308, -224.4154023411693402 ) ) ;
#70015 = ORIENTED_EDGE ( 'NONE', *, *, #66150, .T. ) ;
#70016 = DIRECTION ( 'NONE',  ( -0.000000000000000000, -1.000000000000000000, -0.000000000000000000 ) ) ;
#70017 = VECTOR ( 'NONE', #39171, 1000.000000000000000 ) ;
#70018 = CARTESIAN_POINT ( 'NONE',  ( 34.38359394569770444, -293.2431364434484635, -284.2704900693136096 ) ) ;
#70019 = LINE ( 'NONE', #39235, #85186 ) ;
#70020 = CARTESIAN_POINT ( 'NONE',  ( -102.0455923789670294, -281.6237833571633473, -301.4846348637937581 ) ) ;
#70021 = CARTESIAN_POINT ( 'NONE',  ( -88.45771724803582003, -294.8065940832087790, -327.7034579383222876 ) ) ;
#70022 = CARTESIAN_POINT ( 'NONE',  ( 29.64105354140610871, -279.2258184348530676, -234.8427613311651498 ) ) ;
#70023 = CARTESIAN_POINT ( 'NONE',  ( -15.56993195612021985, -287.6432004864767578, -196.9624524223594619 ) ) ;
#70024 = CARTESIAN_POINT ( 'NONE',  ( 34.75888697250452708, -287.5372221635396386, -281.8646580402398172 ) ) ;
#70025 = AXIS2_PLACEMENT_3D ( 'NONE', #38554, #8734, #16778 ) ;
#70026 = CARTESIAN_POINT ( 'NONE',  ( -76.71000586960695955, -279.1093007345367027, -332.7175468353536871 ) ) ;
#70027 = CARTESIAN_POINT ( 'NONE',  ( -85.55938317218904388, -293.7425687897037392, -327.4105953030698402 ) ) ;
#70028 = CARTESIAN_POINT ( 'NONE',  ( -110.3590002741893983, -298.1548430711811193, -282.4626837410476128 ) ) ;
#70029 = CARTESIAN_POINT ( 'NONE',  ( -102.2150070530536397, -276.8819810910147226, -304.6916372377997959 ) ) ;
#70030 = VERTEX_POINT ( 'NONE', #57765 ) ;
#70031 = LINE ( 'NONE', #88634, #43985 ) ;
#70032 = CARTESIAN_POINT ( 'NONE',  ( -98.21464024813640492, -296.8483285301734895, -223.2205352468766364 ) ) ;
#70033 = CARTESIAN_POINT ( 'NONE',  ( -75.43214031300453826, -291.4844407459838180, -334.3325814547297341 ) ) ;
#70034 = CARTESIAN_POINT ( 'NONE',  ( 14.94470690833983895, -295.9295690866154018, -325.7919041325711191 ) ) ;
#70035 = AXIS2_PLACEMENT_3D ( 'NONE', #10107, #11035, #54131 ) ;
#70036 = ADVANCED_FACE ( 'NONE', ( #78603 ), #51554, .F. ) ;
#70037 = CARTESIAN_POINT ( 'NONE',  ( -48.06775505554502814, -289.8434933283029977, -342.7229596913379623 ) ) ;
#70038 = CARTESIAN_POINT ( 'NONE',  ( -43.52141711092885146, -250.2819871534461242, -453.2997318089873033 ) ) ;
#70039 = ORIENTED_EDGE ( 'NONE', *, *, #38462, .F. ) ;
#70040 = CARTESIAN_POINT ( 'NONE',  ( 25.73014385346732524, -281.1910097350853448, -314.1422330179764231 ) ) ;
#70041 = CARTESIAN_POINT ( 'NONE',  ( -109.3391725997841206, -296.8597198683316947, -297.5238352205884098 ) ) ;
#70042 = CARTESIAN_POINT ( 'NONE',  ( -74.05920865460632285, -289.7092062044704903, -204.0879707117975670 ) ) ;
#70043 = CARTESIAN_POINT ( 'NONE',  ( 7.969379842708195660, -298.9382089701037444, -193.3797674470473567 ) ) ;
#70044 = DIRECTION ( 'NONE',  ( -0.000000000000000000, -0.000000000000000000, -1.000000000000000000 ) ) ;
#70045 = TOROIDAL_SURFACE ( 'NONE', #35297, 24.50000000000000355, 0.5000000000000000000 ) ;
#70046 = DIRECTION ( 'NONE',  ( 1.000000000000000000, 0.000000000000000000, -0.000000000000000000 ) ) ;
#70047 = LINE ( 'NONE', #91799, #37055 ) ;
#70048 = CARTESIAN_POINT ( 'NONE',  ( -75.30181922533614625, -291.0688199094076367, -336.5558089403842814 ) ) ;
#70049 = CARTESIAN_POINT ( 'NONE',  ( -115.3430155898818299, -293.8380690714490129, -288.1317622949166548 ) ) ;
#70050 = ORIENTED_EDGE ( 'NONE', *, *, #74984, .F. ) ;
#70051 = CARTESIAN_POINT ( 'NONE',  ( 15.09789521561530812, -280.1173063969657733, -214.0441939573391608 ) ) ;
#70052 = CARTESIAN_POINT ( 'NONE',  ( -52.48418468218542188, -287.8579096348968278, -197.0758289747388972 ) ) ;
#70053 = CARTESIAN_POINT ( 'NONE',  ( 39.01455486600244171, -286.1779079262321375, -274.4099502860120765 ) ) ;
#70054 = CARTESIAN_POINT ( 'NONE',  ( -33.93229131641489005, -272.0949882416676928, -195.6054870229756659 ) ) ;
#70055 = CARTESIAN_POINT ( 'NONE',  ( -24.36905806254085860, -276.1390528519882537, -197.0075956062217131 ) ) ;
#70056 = CARTESIAN_POINT ( 'NONE',  ( -108.3684020862248900, -288.9221122632346237, -248.0354542839610303 ) ) ;
#70057 = CARTESIAN_POINT ( 'NONE',  ( -111.2738085925807781, -280.2020354812181040, -286.9245965685014426 ) ) ;
#70058 = VECTOR ( 'NONE', #44954, 1000.000000000000000 ) ;
#70059 = ORIENTED_EDGE ( 'NONE', *, *, #76674, .F. ) ;
#70061 = CARTESIAN_POINT ( 'NONE',  ( 35.23995747301554360, -281.0208500775024731, -279.4791700419551717 ) ) ;
#70060 = CARTESIAN_POINT ( 'NONE',  ( -38.35385429679652702, -280.0391191326776834, -197.3557344419517960 ) ) ;
#70062 = CARTESIAN_POINT ( 'NONE',  ( -48.43562767465265750, -278.2697369981431166, -346.2990308494979104 ) ) ;
#70063 = CARTESIAN_POINT ( 'NONE',  ( -56.44273174643397795, -278.6063596657565427, -196.1231226425536249 ) ) ;
#70064 = CARTESIAN_POINT ( 'NONE',  ( 63.33052876804309506, 47.60566335709030739, -316.2373129133302996 ) ) ;
#70065 = CARTESIAN_POINT ( 'NONE',  ( -104.0310793156580615, -273.9898844114041481, -232.2366945470407984 ) ) ;
#70066 = CARTESIAN_POINT ( 'NONE',  ( -46.08063821706912933, -299.3686419053470331, -194.4517163698844797 ) ) ;
#70067 = EDGE_CURVE ( 'NONE', #18551, #74338, #71987, .T. ) ;
#70068 = CARTESIAN_POINT ( 'NONE',  ( -110.4542110544635705, -286.8376638359844719, -287.0812184334320705 ) ) ;
#70069 = ORIENTED_EDGE ( 'NONE', *, *, #43842, .F. ) ;
#70070 = LINE ( 'NONE', #54903, #3032 ) ;
#70071 = CARTESIAN_POINT ( 'NONE',  ( 6.038562617998687543, -289.5279785423485919, -329.5207427954307491 ) ) ;
#70072 = CARTESIAN_POINT ( 'NONE',  ( 23.34659609950567827, -289.9292637908608299, -316.0875295760779409 ) ) ;
#70073 = CARTESIAN_POINT ( 'NONE',  ( -48.08414619837272141, -288.5408766818652566, -342.7205274786652467 ) ) ;
#70074 = CARTESIAN_POINT ( 'NONE',  ( -95.29251645813006633, -283.3748125464334748, -320.9697120159855785 ) ) ;
#70075 = CARTESIAN_POINT ( 'NONE',  ( -27.43098593705121857, -278.5798868866773432, -197.1778517569633209 ) ) ;
#70076 = CARTESIAN_POINT ( 'NONE',  ( -57.75643385455133938, -287.6462839104783029, -198.9346158040809769 ) ) ;
#70077 = CARTESIAN_POINT ( 'NONE',  ( 20.71534566357370721, -280.6658037607555798, -315.7493013403125701 ) ) ;
#70078 = CARTESIAN_POINT ( 'NONE',  ( -107.7040704593373022, -280.1464140161695582, -249.1389522167001473 ) ) ;
#70079 = CARTESIAN_POINT ( 'NONE',  ( -93.64945299741332008, -278.3848553598327271, -316.9363339445436054 ) ) ;
#70080 = CARTESIAN_POINT ( 'NONE',  ( -110.4077783357235631, -289.0544869739360365, -293.5422813694628417 ) ) ;
#70081 = CARTESIAN_POINT ( 'NONE',  ( -102.3872318523210794, -285.8917376447013226, -229.4558906519198729 ) ) ;
#70082 = CARTESIAN_POINT ( 'NONE',  ( -106.6264174583855322, -285.4740623237248087, -236.9073461845415807 ) ) ;
#70083 = CARTESIAN_POINT ( 'NONE',  ( 30.33532281853748458, -282.0852809381280508, -297.7257040304157840 ) ) ;
#70084 = ORIENTED_EDGE ( 'NONE', *, *, #27513, .T. ) ;
#70085 = CARTESIAN_POINT ( 'NONE',  ( 154.7659666677360235, 19.56018909072649237, -12.94946946942526189 ) ) ;
#70086 = CARTESIAN_POINT ( 'NONE',  ( -112.1368265475510810, -292.2589893116461326, -282.4439382293692233 ) ) ;
#70087 = AXIS2_PLACEMENT_3D ( 'NONE', #14563, #50530, #27841 ) ;
#70088 = CARTESIAN_POINT ( 'NONE',  ( -34.95888523483504429, -290.7662912871851972, -193.8783166674654410 ) ) ;
#70089 = CARTESIAN_POINT ( 'NONE',  ( 30.39700795093223817, -274.2374291139962565, -242.3913104308159348 ) ) ;
#70090 = ADVANCED_FACE ( 'NONE', ( #29348 ), #35039, .T. ) ;
#70091 = CARTESIAN_POINT ( 'NONE',  ( -56.05351810221746689, -294.6356332292452294, -344.9478504111654615 ) ) ;
#70092 = CARTESIAN_POINT ( 'NONE',  ( -34.81429792446053995, -290.5643519943133697, -196.7111350089235771 ) ) ;
#70093 = CARTESIAN_POINT ( 'NONE',  ( -76.20901778210176758, -293.8187902417166129, -333.4074298022957805 ) ) ;
#70094 = CONICAL_SURFACE ( 'NONE', #29262, 2.888540232138026020, 0.09862129276974965220 ) ;
#70095 = CARTESIAN_POINT ( 'NONE',  ( -76.06527637435584666, -290.7872594468521470, -332.7118609393764359 ) ) ;
#70096 = DIRECTION ( 'NONE',  ( 0.000000000000000000, 0.000000000000000000, 1.000000000000000000 ) ) ;
#70097 = AXIS2_PLACEMENT_3D ( 'NONE', #14773, #85780, #65911 ) ;
#70098 = CARTESIAN_POINT ( 'NONE',  ( -110.0618102870256649, -292.7886552846488826, -251.9575803212418350 ) ) ;
#70099 = CARTESIAN_POINT ( 'NONE',  ( 37.82368939789227369, -291.5157384831929335, -267.5316428570143330 ) ) ;
#70100 = CARTESIAN_POINT ( 'NONE',  ( -47.79790937527012318, -297.1851520823764190, -344.6801606029999334 ) ) ;
#70101 = CARTESIAN_POINT ( 'NONE',  ( 7.060094920348323200, -287.6147388181897782, -212.0571258667505106 ) ) ;
#70102 = CARTESIAN_POINT ( 'NONE',  ( 31.74191530042645581, -295.9403147691383538, -300.1150034945645189 ) ) ;
#70103 = AXIS2_PLACEMENT_3D ( 'NONE', #79330, #28658, #27730 ) ;
#70104 = CARTESIAN_POINT ( 'NONE',  ( 0.3503886795678022303, -276.5314665964218079, -205.0950068330576812 ) ) ;
#70105 = PRODUCT_DEFINITION_SHAPE ( 'NONE', 'NONE',  #19232 ) ;
#70106 = CARTESIAN_POINT ( 'NONE',  ( -85.10803231170086747, -296.6087331962230564, -210.1736082341220140 ) ) ;
#70107 = CARTESIAN_POINT ( 'NONE',  ( 28.92796992001190048, -274.2341822440664600, -303.4357235838158431 ) ) ;
#70108 = CARTESIAN_POINT ( 'NONE',  ( -7.398199437998763450, -278.5277091080366745, -202.1951304345557219 ) ) ;
#70109 = CARTESIAN_POINT ( 'NONE',  ( -31.32236120155269887, -275.3349129568796343, -197.1985666610361250 ) ) ;
#70110 = CARTESIAN_POINT ( 'NONE',  ( 11.42371081850256509, -273.2874553746036099, -211.4659866461770150 ) ) ;
#70111 = AXIS2_PLACEMENT_3D ( 'NONE', #40249, #40711, #48772 ) ;
#70112 = ADVANCED_FACE ( 'NONE', ( #65822 ), #26200, .T. ) ;
#70113 = CARTESIAN_POINT ( 'NONE',  ( -110.8015486704573078, -298.0345106817683245, -265.9992871852042526 ) ) ;
#70114 = DIRECTION ( 'NONE',  ( 0.000000000000000000, 0.000000000000000000, -1.000000000000000000 ) ) ;
#70115 = CARTESIAN_POINT ( 'NONE',  ( -107.0199290459907076, -297.0578817382797183, -292.8307911038286306 ) ) ;
#70116 = DIRECTION ( 'NONE',  ( 1.000000000000000000, 0.000000000000000000, 0.000000000000000000 ) ) ;
#70118 = CARTESIAN_POINT ( 'NONE',  ( -35.81558274971027345, -298.0717807918495623, -197.3611180005151482 ) ) ;
#70117 = CARTESIAN_POINT ( 'NONE',  ( -56.88907468414934954, -287.3229788565211607, -343.1907819917381062 ) ) ;
#70119 = AXIS2_PLACEMENT_3D ( 'NONE', #32601, #40592, #84629 ) ;
#70120 = CARTESIAN_POINT ( 'NONE',  ( 16.29918898183453280, -286.7887501955512448, -215.1193311224510580 ) ) ;
#70121 = CARTESIAN_POINT ( 'NONE',  ( -75.65684075173737710, -289.2157159088247340, -337.1270845412653898 ) ) ;
#70122 = CARTESIAN_POINT ( 'NONE',  ( -88.51033734342924220, -299.3192809903030707, -214.9715400156740372 ) ) ;
#70123 = CARTESIAN_POINT ( 'NONE',  ( -41.15755579295959166, -293.1001064526491291, -345.1099872423227453 ) ) ;
#70124 = CARTESIAN_POINT ( 'NONE',  ( 35.17869001448485022, -280.4265417771505895, -244.8062382774861305 ) ) ;
#70125 = CARTESIAN_POINT ( 'NONE',  ( -110.4542110544635705, -288.2666405000204577, -253.6410175316879361 ) ) ;
#70126 = CARTESIAN_POINT ( 'NONE',  ( -72.05945324018348686, -277.5932229986503330, -203.8239042216753205 ) ) ;
#70127 = VECTOR ( 'NONE', #74678, 1000.000000000000000 ) ;
#70128 = DIRECTION ( 'NONE',  ( -1.000000000000000000, 0.000000000000000000, 0.000000000000000000 ) ) ;
#70129 = CARTESIAN_POINT ( 'NONE',  ( -96.88970423976742552, -288.7502650258430208, -313.2699249088517490 ) ) ;
#70130 = LINE ( 'NONE', #62562, #74395 ) ;
#70131 = CARTESIAN_POINT ( 'NONE',  ( -97.38436315569568080, -287.9377561632786069, -315.3256265021667559 ) ) ;
#70132 = CARTESIAN_POINT ( 'NONE',  ( -36.49202560124081884, -299.6630912361257515, -196.5608761726103353 ) ) ;
#70133 = CARTESIAN_POINT ( 'NONE',  ( 25.45650493751523058, -283.5571519956374686, -313.9156400115997485 ) ) ;
#70135 = CARTESIAN_POINT ( 'NONE',  ( 26.45883956513898383, -281.0671197595808621, -234.8858993806427407 ) ) ;
#70134 = CARTESIAN_POINT ( 'NONE',  ( -112.7422171607660033, -270.7040298161851410, -264.7091374725872015 ) ) ;
#70136 = CARTESIAN_POINT ( 'NONE',  ( -112.3053118441762308, -296.4981134196745529, -288.0095292644644474 ) ) ;
#70137 = CARTESIAN_POINT ( 'NONE',  ( -51.69400596789095914, -275.2903632745978939, -198.1328297875758437 ) ) ;
#70138 = CARTESIAN_POINT ( 'NONE',  ( 37.19214811362475359, -283.4392933617943413, -261.5587303271289557 ) ) ;
#70139 = CARTESIAN_POINT ( 'NONE',  ( -54.26962704452505193, -272.7498925234039007, -199.0332036506258078 ) ) ;
#70140 = ORIENTED_EDGE ( 'NONE', *, *, #36317, .F. ) ;
#70141 = CARTESIAN_POINT ( 'NONE',  ( 203.9792886337422146, 295.7120653557082619, -54.00000000006011902 ) ) ;
#70142 = CARTESIAN_POINT ( 'NONE',  ( -111.0492090421384148, -286.6852204622855993, -258.4880419259926612 ) ) ;
#70143 = CIRCLE ( 'NONE', #29316, 0.5000000000000004441 ) ;
#70144 = DIRECTION ( 'NONE',  ( 0.000000000000000000, 0.000000000000000000, 1.000000000000000000 ) ) ;
#70145 = CARTESIAN_POINT ( 'NONE',  ( -19.05039376806006857, -271.7666405000204009, -190.3683826091709363 ) ) ;
#70146 = CARTESIAN_POINT ( 'NONE',  ( -107.4330135628172940, -277.3448988729600160, -301.9766008593547326 ) ) ;
#70147 = CARTESIAN_POINT ( 'NONE',  ( -100.0341260492287887, -288.3740368261592835, -313.6750897223426477 ) ) ;
#70148 = CARTESIAN_POINT ( 'NONE',  ( -15.91257355089835102, -284.2900160933936036, -340.8699846958140824 ) ) ;
#70149 = CARTESIAN_POINT ( 'NONE',  ( 24.45234119004402373, -276.5992226907876557, -230.0134182647407783 ) ) ;
#70150 = CARTESIAN_POINT ( 'NONE',  ( -95.80765697662620539, -285.3096222734389471, -319.5782892374174367 ) ) ;
#70151 = CARTESIAN_POINT ( 'NONE',  ( -105.5887832998617455, -282.9861027242961882, -297.5081712046438724 ) ) ;
#70152 = CARTESIAN_POINT ( 'NONE',  ( -38.40717569289950006, -282.0389554427737835, -195.3559412704315434 ) ) ;
#70153 = CARTESIAN_POINT ( 'NONE',  ( -60.87313913315630032, -273.9218203818846860, -196.9892450004276157 ) ) ;
#70154 = CARTESIAN_POINT ( 'NONE',  ( 26.93172964526132063, -274.8278898435115707, -227.9591577722697195 ) ) ;
#70155 = CARTESIAN_POINT ( 'NONE',  ( -71.57161381736655414, -297.4280830105003588, -336.4785320829901707 ) ) ;
#70156 = CARTESIAN_POINT ( 'NONE',  ( -26.41588298435790350, -486.4924983417995463, -507.6442049081570076 ) ) ;
#70157 = EDGE_CURVE ( 'NONE', #12291, #41724, #85139, .T. ) ;
#70158 = CARTESIAN_POINT ( 'NONE',  ( 222.4306832106270804, -142.7221692137691775, -21.50000000000000000 ) ) ;
#70159 = CARTESIAN_POINT ( 'NONE',  ( -98.08767205084976126, -295.3040801123506753, -225.0599817903433859 ) ) ;
#70160 = CARTESIAN_POINT ( 'NONE',  ( 34.22357723811858676, -275.2536962473726021, -285.0716420161719498 ) ) ;
#70161 = VECTOR ( 'NONE', #25346, 1000.000000000000114 ) ;
#70162 = CARTESIAN_POINT ( 'NONE',  ( -78.05007469219722793, -298.5981637663423953, -205.3663431947522611 ) ) ;
#70163 = CARTESIAN_POINT ( 'NONE',  ( 19.42473902992207258, -288.6471739415850379, -222.8487983678375599 ) ) ;
#70164 = CARTESIAN_POINT ( 'NONE',  ( -22.21587914087880122, -296.3819188786374639, -345.1536128626588038 ) ) ;
#70165 = CARTESIAN_POINT ( 'NONE',  ( 32.95390440070720217, -294.3673171916275351, -239.9220525983916446 ) ) ;
#70166 = CARTESIAN_POINT ( 'NONE',  ( -110.9785136476887715, -292.3807953644222266, -283.6895883847779487 ) ) ;
#70167 = CARTESIAN_POINT ( 'NONE',  ( 6.005326123405473560, -278.6415284148576461, -209.3605955337199305 ) ) ;
#70168 = TOROIDAL_SURFACE ( 'NONE', #617, 24.16304133878946558, 4.003189038634632269 ) ;
#70169 = CARTESIAN_POINT ( 'NONE',  ( -111.7179230733174080, -280.4324571250195959, -273.4419710379085586 ) ) ;
#70170 = CARTESIAN_POINT ( 'NONE',  ( -71.61514395911544284, -293.5883958783925323, -336.4559767305045739 ) ) ;
#70171 = CARTESIAN_POINT ( 'NONE',  ( -107.0807543817784051, -286.0279732045419223, -300.1055317402342553 ) ) ;
#70172 = CARTESIAN_POINT ( 'NONE',  ( -110.4049637105465962, -283.3936745071776500, -276.3599168378987088 ) ) ;
#70173 = CARTESIAN_POINT ( 'NONE',  ( 201.4080446206525892, 287.5879394527656814, -97.22726418418297101 ) ) ;
#70174 = ORIENTED_EDGE ( 'NONE', *, *, #58173, .T. ) ;
#70175 = CARTESIAN_POINT ( 'NONE',  ( -77.05700576180784367, -285.1708569975347132, -209.0248506957818506 ) ) ;
#70176 = VERTEX_POINT ( 'NONE', #13747 ) ;
#70177 = CARTESIAN_POINT ( 'NONE',  ( 29.49926489302045240, -283.1228378733546833, -308.0696210621243267 ) ) ;
#70178 = CIRCLE ( 'NONE', #33867, 7.999999999999992895 ) ;
#70179 = CARTESIAN_POINT ( 'NONE',  ( -89.26018638665631499, -273.6294670924335151, -219.0136908671740343 ) ) ;
#70180 = CARTESIAN_POINT ( 'NONE',  ( 37.90305207048154301, -286.1665472847081446, -256.0001992751724060 ) ) ;
#70181 = AXIS2_PLACEMENT_3D ( 'NONE', #45316, #74220, #9339 ) ;
#70182 = CARTESIAN_POINT ( 'NONE',  ( 27.64575054332746618, -281.9556242751584136, -229.4026027034914819 ) ) ;
#70183 = CARTESIAN_POINT ( 'NONE',  ( -56.72901356050696364, -278.8176855415479736, -344.2183796032391001 ) ) ;
#70184 = CARTESIAN_POINT ( 'NONE',  ( 21.88688421964502595, -281.5433865196819170, -221.3173866481988910 ) ) ;
#70185 = CARTESIAN_POINT ( 'NONE',  ( -105.5937364680635966, -275.8380690714489560, -285.9065529553535612 ) ) ;
#70186 = CARTESIAN_POINT ( 'NONE',  ( -11.98663864091307474, -92.10731666755650338, -360.1219413251452579 ) ) ;
#70187 = EDGE_LOOP ( 'NONE', ( #6126, #4493, #24628, #17018 ) ) ;
#70188 = CARTESIAN_POINT ( 'NONE',  ( 6.223881610526908581, -276.6447947857928966, -209.4524614016336272 ) ) ;
#70189 = CARTESIAN_POINT ( 'NONE',  ( 102.4330173972533942, 116.6819059004242121, -282.6453656452667360 ) ) ;
#70190 = VECTOR ( 'NONE', #55057, 1000.000000000000000 ) ;
#70191 = CARTESIAN_POINT ( 'NONE',  ( -19.10892650690468741, -278.3079144654925585, -197.9238567164312883 ) ) ;
#70192 = CARTESIAN_POINT ( 'NONE',  ( 36.09737169397146772, -295.0641840472533204, -250.8000357066200081 ) ) ;
#70193 = CARTESIAN_POINT ( 'NONE',  ( -35.65656996429540726, -294.3790745905125164, -343.4561398372795793 ) ) ;
#70194 = CARTESIAN_POINT ( 'NONE',  ( -56.16765608581226843, -291.3237198226568694, -195.7065483182462060 ) ) ;
#70195 = CARTESIAN_POINT ( 'NONE',  ( 165.2494399300530290, -11.64849832608277325, -3.999999999999998224 ) ) ;
#70197 = CARTESIAN_POINT ( 'NONE',  ( 26.37659004006917840, -286.4587747241707802, -307.6967606629390275 ) ) ;
#70196 = CARTESIAN_POINT ( 'NONE',  ( -71.82449624844453240, -294.0737123054893800, -338.5486759869114621 ) ) ;
#70198 = CARTESIAN_POINT ( 'NONE',  ( 30.98348576775781282, -295.0277830734895588, -241.2032618519249354 ) ) ;
#70199 = CARTESIAN_POINT ( 'NONE',  ( -86.06553647444221156, -286.6753809574609022, -215.2728046087326277 ) ) ;
#70200 = VERTEX_POINT ( 'NONE', #43082 ) ;
#70201 = CARTESIAN_POINT ( 'NONE',  ( -114.1545492466821941, -291.4824016675901248, -271.2380696515119780 ) ) ;
#70202 = CARTESIAN_POINT ( 'NONE',  ( 22.63887298028547335, -282.6254565140579871, -312.0782522480375860 ) ) ;
#70203 = CARTESIAN_POINT ( 'NONE',  ( -112.8153637342337134, -295.1785656691827171, -283.7659655300626014 ) ) ;
#70204 = CIRCLE ( 'NONE', #50584, 5.343514653206204557 ) ;
#70205 = CARTESIAN_POINT ( 'NONE',  ( -112.4842181883824708, -291.5569336040776420, -254.2440706921088065 ) ) ;
#70206 = CARTESIAN_POINT ( 'NONE',  ( -85.12154886832037448, -290.1837793380809671, -330.7334241161838122 ) ) ;
#70207 = CARTESIAN_POINT ( 'NONE',  ( 31.83991718493888712, -287.4093023902037203, -247.0608211935572740 ) ) ;
#70208 = EDGE_LOOP ( 'NONE', ( #54070, #10398 ) ) ;
#70209 = DIRECTION ( 'NONE',  ( 0.000000000000000000, 0.000000000000000000, 1.000000000000000000 ) ) ;
#70210 = CARTESIAN_POINT ( 'NONE',  ( -108.6956664422981476, -298.7393526825194385, -244.8872692269707727 ) ) ;
#70211 = CARTESIAN_POINT ( 'NONE',  ( -33.34954539967857556, -296.7859813466320702, -193.8551358194268346 ) ) ;
#70212 = CARTESIAN_POINT ( 'NONE',  ( -9.145715563525500968, -279.4888762562534907, -202.7712156085632671 ) ) ;
#70213 = CARTESIAN_POINT ( 'NONE',  ( 19.99420486186082613, -274.3627555347478051, -218.9786170727966521 ) ) ;
#70214 = CARTESIAN_POINT ( 'NONE',  ( -109.9557685152110196, -295.1962332349838221, -257.7950992953176410 ) ) ;
#70215 = CARTESIAN_POINT ( 'NONE',  ( -9.503543598582819385, -278.5449066972386163, -339.1928092203173719 ) ) ;
#70216 = CARTESIAN_POINT ( 'NONE',  ( 35.09338491650915870, -273.9032675378040835, -286.6676536452231971 ) ) ;
#70217 = CARTESIAN_POINT ( 'NONE',  ( -95.07632328465967930, -297.1216045472151563, -315.6804714105925314 ) ) ;
#70218 = CARTESIAN_POINT ( 'NONE',  ( -110.3595161834604284, -297.7248020632274574, -263.2834286698070514 ) ) ;
#70219 = CARTESIAN_POINT ( 'NONE',  ( -76.65187845323568183, -297.1687053925359123, -335.6999819723004066 ) ) ;
#70220 = CARTESIAN_POINT ( 'NONE',  ( -23.74768633649188843, -296.2217872372291936, -195.1990643542264934 ) ) ;
#70221 = CARTESIAN_POINT ( 'NONE',  ( -4.795139363022840051, -293.1438916811865170, -204.8902111711572047 ) ) ;
#70222 = CARTESIAN_POINT ( 'NONE',  ( -95.91125400491768005, -274.0270365449062524, -220.6038861598206040 ) ) ;
#70223 = CARTESIAN_POINT ( 'NONE',  ( -108.9970896909220954, -289.3469120019418028, -253.5467446630191830 ) ) ;
#70224 = LINE ( 'NONE', #11020, #18563 ) ;
#70225 = CARTESIAN_POINT ( 'NONE',  ( -113.8022095549412853, -273.1516701801307931, -261.7985598755788033 ) ) ;
#70226 = CARTESIAN_POINT ( 'NONE',  ( -110.2625633184394331, -296.8349840934420740, -274.1867157484186919 ) ) ;
#70227 = CARTESIAN_POINT ( 'NONE',  ( -22.90650122120761267, -282.2157121806354212, -196.3483607646245162 ) ) ;
#70228 = CARTESIAN_POINT ( 'NONE',  ( 38.38076764984798217, -280.3745236848430409, -281.2884299263073444 ) ) ;
#70229 = CARTESIAN_POINT ( 'NONE',  ( 8.174043579994970443, -275.7967030543647979, -332.4079228316180092 ) ) ;
#70230 = CARTESIAN_POINT ( 'NONE',  ( 33.58731567090119086, -279.5936540000705008, -242.3689314604473282 ) ) ;
#70231 = CARTESIAN_POINT ( 'NONE',  ( 37.87600967575217226, -279.5469251472152905, -269.9659483041411931 ) ) ;
#70232 = EDGE_CURVE ( 'NONE', #34264, #70640, #22233, .T. ) ;
#70233 = CARTESIAN_POINT ( 'NONE',  ( -64.77169839840712484, -272.2615217326580250, -202.0615872460528806 ) ) ;
#70234 = CARTESIAN_POINT ( 'NONE',  ( -110.5504780882395153, -280.3423608634501534, -286.7123844378165813 ) ) ;
#70235 = CARTESIAN_POINT ( 'NONE',  ( 175.2296996224750103, 158.6892791692949629, 0.000000000000000000 ) ) ;
#70236 = PLANE ( 'NONE',  #27733 ) ;
#70237 = CARTESIAN_POINT ( 'NONE',  ( -70.26938460875699377, -295.8640182837222596, -201.8794298262254756 ) ) ;
#70238 = AXIS2_PLACEMENT_3D ( 'NONE', #3948, #2552, #82995 ) ;
#70239 = CARTESIAN_POINT ( 'NONE',  ( -40.63242019631586999, -292.0118699220529379, -193.4182850485302367 ) ) ;
#70240 = CARTESIAN_POINT ( 'NONE',  ( 20.34052322117934963, -278.2166602097238410, -318.5564449296827547 ) ) ;
#70241 = CARTESIAN_POINT ( 'NONE',  ( -21.48706350752827987, -272.2552977671797976, -197.0560626092981238 ) ) ;
#70242 = CARTESIAN_POINT ( 'NONE',  ( 194.7510731661265595, -164.3527196417747689, 21.50000000000000000 ) ) ;
#70243 = CARTESIAN_POINT ( 'NONE',  ( -58.06783165448300821, -285.2378985831060163, -343.0774042051185120 ) ) ;
#70244 = AXIS2_PLACEMENT_3D ( 'NONE', #90336, #33066, #54369 ) ;
#70245 = CARTESIAN_POINT ( 'NONE',  ( 23.24267728912972686, -284.9485168767567416, -226.0659953627877314 ) ) ;
#70246 = LINE ( 'NONE', #41794, #24050 ) ;
#70247 = CARTESIAN_POINT ( 'NONE',  ( -7.842727875097758705, -293.4517127829731180, -337.5829601827294368 ) ) ;
#70248 = CARTESIAN_POINT ( 'NONE',  ( 3.140099106848808663, -284.7418703323610316, -208.1350028090945443 ) ) ;
#70249 = CARTESIAN_POINT ( 'NONE',  ( 193.6056169066500274, 279.7126221763799094, -126.0203154767880989 ) ) ;
#70250 = CARTESIAN_POINT ( 'NONE',  ( -64.31133829564589632, -293.4037719593771385, -340.3992879172372454 ) ) ;
#70251 = CARTESIAN_POINT ( 'NONE',  ( 7.155476341450177635, -285.1256556595370739, -208.3064391421114578 ) ) ;
#70252 = CARTESIAN_POINT ( 'NONE',  ( -27.47133515261248249, -281.7796282053889172, -197.1723980869047637 ) ) ;
#70253 = CARTESIAN_POINT ( 'NONE',  ( -10.14934143917211884, -287.6042921766826339, -198.6904798207445992 ) ) ;
#70254 = CARTESIAN_POINT ( 'NONE',  ( 30.16648155789390273, -280.2476415581548395, -305.2411898978089084 ) ) ;
#70255 = CARTESIAN_POINT ( 'NONE',  ( 23.50949717981876219, -288.1119817840691439, -310.7092745384828163 ) ) ;
#70256 = AXIS2_PLACEMENT_3D ( 'NONE', #75866, #68781, #76346 ) ;
#70257 = CARTESIAN_POINT ( 'NONE',  ( -37.02385347869132914, -281.4814833932616693, -196.7725734079370454 ) ) ;
#70258 = CARTESIAN_POINT ( 'NONE',  ( -39.71669486285533424, -280.8244339688591253, -197.2256526752249499 ) ) ;
#70259 = CARTESIAN_POINT ( 'NONE',  ( -15.90600449527480897, -288.3078116544500631, -198.0648377633520170 ) ) ;
#70260 = ORIENTED_EDGE ( 'NONE', *, *, #17026, .T. ) ;
#70261 = CARTESIAN_POINT ( 'NONE',  ( -54.59310246451565263, -297.6696818863487692, -195.3185359247007682 ) ) ;
#70262 = CARTESIAN_POINT ( 'NONE',  ( -93.81709411303738477, -293.2121608428080322, -221.5515218024827675 ) ) ;
#70263 = CARTESIAN_POINT ( 'NONE',  ( 221.8344101925596306, -43.55766379199612004, -22.50000000000000000 ) ) ;
#70264 = CARTESIAN_POINT ( 'NONE',  ( 108.5619616845123971, -302.2645883696979467, -190.3030568020281805 ) ) ;
#70265 = VERTEX_POINT ( 'NONE', #57308 ) ;
#70266 = CARTESIAN_POINT ( 'NONE',  ( 0.2999342423192604135, -272.5520562232745760, -205.2836413248113843 ) ) ;
#70267 = CARTESIAN_POINT ( 'NONE',  ( 189.9243309297870610, 215.0000000000000568, 20.22542485937349355 ) ) ;
#70268 = CARTESIAN_POINT ( 'NONE',  ( -74.23705991405583404, -293.9336245985008418, -337.0923468979850668 ) ) ;
#70269 = CARTESIAN_POINT ( 'NONE',  ( -84.10942055557747210, -296.8968344065521023, -214.1633592599051781 ) ) ;
#70270 = CARTESIAN_POINT ( 'NONE',  ( -58.87339304845819044, -290.8557890698519373, -340.8920315504221321 ) ) ;
#70271 = CIRCLE ( 'NONE', #92955, 1.000000000000000888 ) ;
#70272 = CARTESIAN_POINT ( 'NONE',  ( 24.51730149701409545, -282.7554761154105449, -229.6308450041551055 ) ) ;
#70273 = CARTESIAN_POINT ( 'NONE',  ( -62.55198748662395047, -290.7990188331613695, -342.5492201428829731 ) ) ;
#70274 = CARTESIAN_POINT ( 'NONE',  ( -112.6449147126792383, -291.6962458976706785, -283.9525761666745325 ) ) ;
#70275 = CARTESIAN_POINT ( 'NONE',  ( -91.11408915279824328, -287.2888084187766822, -218.0033848817627131 ) ) ;
#70276 = CARTESIAN_POINT ( 'NONE',  ( 10.82135480106749092, -280.8636275364432890, -210.2151607901950285 ) ) ;
#70277 = CARTESIAN_POINT ( 'NONE',  ( -110.8673717908075247, -294.8539699541096866, -252.9459002434879551 ) ) ;
#70278 = CARTESIAN_POINT ( 'NONE',  ( -35.90132357153543552, -282.8679097882399560, -347.3607618358029754 ) ) ;
#70279 = CARTESIAN_POINT ( 'NONE',  ( 35.37926986804953344, -277.6060787597874082, -285.2784235686195871 ) ) ;
#70280 = CARTESIAN_POINT ( 'NONE',  ( -67.74223827176244583, -276.1233781216987495, -207.3071070584150277 ) ) ;
#70281 = CARTESIAN_POINT ( 'NONE',  ( 18.14770556826152159, -274.5095428760557184, -322.2735429811021390 ) ) ;
#70282 = CARTESIAN_POINT ( 'NONE',  ( -57.23711263161519724, -282.8906705383787994, 52.50000000000000711 ) ) ;
#70283 = CARTESIAN_POINT ( 'NONE',  ( 23.73742078915519826, -280.5033509488308141, -230.1783568695826148 ) ) ;
#70284 = CARTESIAN_POINT ( 'NONE',  ( -84.60924697647813275, -278.8916447344553262, -330.7094156097239193 ) ) ;
#70285 = CARTESIAN_POINT ( 'NONE',  ( -109.7513235723459246, -283.9334340416561417, -244.8725588767660213 ) ) ;
#70286 = CARTESIAN_POINT ( 'NONE',  ( 2.771125923696083682, -294.3581215681567187, -208.0996517589562416 ) ) ;
#70287 = CARTESIAN_POINT ( 'NONE',  ( -76.04415078586332299, -275.1447050386446449, -204.6605124888353373 ) ) ;
#70288 = ADVANCED_FACE ( 'NONE', ( #85691 ), #29190, .T. ) ;
#70289 = CARTESIAN_POINT ( 'NONE',  ( -34.14069766185071586, -275.4067897676488315, -193.9212602059480162 ) ) ;
#70290 = LINE ( 'NONE', #92975, #62186 ) ;
#70292 = EDGE_CURVE ( 'NONE', #67510, #73033, #48831, .T. ) ;
#70291 = CARTESIAN_POINT ( 'NONE',  ( 35.35381607985218722, -275.4733338648393897, -277.0215930222729526 ) ) ;
#70293 = CARTESIAN_POINT ( 'NONE',  ( -110.5785107945265509, -298.7509451813999135, -254.9241625969769132 ) ) ;
#70294 = CARTESIAN_POINT ( 'NONE',  ( -110.4506616161603318, -282.7582995415833125, -254.3292779525702088 ) ) ;
#70295 = CARTESIAN_POINT ( 'NONE',  ( -37.79064699900006730, -291.7133938579762003, -193.3835710070106018 ) ) ;
#70296 = CARTESIAN_POINT ( 'NONE',  ( 35.11164791481240854, -273.3405586240686489, -252.4067546239757576 ) ) ;
#70297 = CARTESIAN_POINT ( 'NONE',  ( 35.62529218920555252, -289.4313103761550678, -292.3668612921380827 ) ) ;
#70298 = CARTESIAN_POINT ( 'NONE',  ( -99.96857200631606588, -289.9950998411681553, -232.2546750636778654 ) ) ;
#70299 = ORIENTED_EDGE ( 'NONE', *, *, #85455, .F. ) ;
#70300 = CARTESIAN_POINT ( 'NONE',  ( -47.64582717111662902, -290.4984690050655445, -194.5949154214187047 ) ) ;
#70301 = CARTESIAN_POINT ( 'NONE',  ( -79.53946562107320517, -291.1314442144685586, -210.7052165904021592 ) ) ;
#70302 = VERTEX_POINT ( 'NONE', #79070 ) ;
#70303 = CARTESIAN_POINT ( 'NONE',  ( 25.60589750796334130, -289.2140786410971032, -314.2597679163053499 ) ) ;
#70304 = CARTESIAN_POINT ( 'NONE',  ( -70.95517775584033870, -279.9291345889272975, -205.5224812524338631 ) ) ;
#70305 = CARTESIAN_POINT ( 'NONE',  ( -0.8653597404803231585, -293.4997981559777713, -337.8368132333877156 ) ) ;
#70306 = CARTESIAN_POINT ( 'NONE',  ( -7.390497174086534393, -287.0860008576058249, -199.4791340293585904 ) ) ;
#70307 = CARTESIAN_POINT ( 'NONE',  ( -114.3056797163455229, -284.9259843041483009, -267.1195321435994856 ) ) ;
#70308 = CARTESIAN_POINT ( 'NONE',  ( 35.72403600755610142, -281.8979466298940793, -271.3097986877388053 ) ) ;
#70309 = CARTESIAN_POINT ( 'NONE',  ( -107.8472915499240230, -262.5275434182412937, -317.6634998498594200 ) ) ;
#70310 = CARTESIAN_POINT ( 'NONE',  ( 83.29146807913110706, 83.53839643160537776, -301.3178837860347130 ) ) ;
#70311 = CARTESIAN_POINT ( 'NONE',  ( 187.7931042187957189, 269.0293024058671563, -137.6635259067655568 ) ) ;
#70312 = CARTESIAN_POINT ( 'NONE',  ( 34.53404840778943452, -274.5695729566004957, -256.7054049009872756 ) ) ;
#70313 = CARTESIAN_POINT ( 'NONE',  ( 1.021519072595784339, -275.4477503498168858, -332.8906680306652106 ) ) ;
#70314 = CARTESIAN_POINT ( 'NONE',  ( -114.2479071756398525, -296.1052303320313399, -266.7319245010062900 ) ) ;
#70315 = CARTESIAN_POINT ( 'NONE',  ( -109.2583768833345346, -269.3191087492390920, -295.4032835330162357 ) ) ;
#70316 = CARTESIAN_POINT ( 'NONE',  ( 37.42017352094932647, -274.4422531652433008, -286.6691281790893413 ) ) ;
#70317 = CARTESIAN_POINT ( 'NONE',  ( -74.80539363038832334, -275.3066419526037407, -206.4703545262239572 ) ) ;
#70318 = VERTEX_POINT ( 'NONE', #14222 ) ;
#70319 = CARTESIAN_POINT ( 'NONE',  ( -112.3730818592268861, -297.6976051538242132, -254.0789924899772814 ) ) ;
#70320 = CARTESIAN_POINT ( 'NONE',  ( 10.16002664193914917, -288.8688850165066810, -325.9399473659889850 ) ) ;
#70321 = CARTESIAN_POINT ( 'NONE',  ( -93.56433119474081650, -296.6393211319078773, -322.7558176957816158 ) ) ;
#70322 = CARTESIAN_POINT ( 'NONE',  ( -93.64016104097697735, -296.3288858487308630, -322.8210595970627992 ) ) ;
#70323 = CARTESIAN_POINT ( 'NONE',  ( 28.73761629076754787, -293.2983231851065398, -239.2172540221910140 ) ) ;
#70324 = ORIENTED_EDGE ( 'NONE', *, *, #43435, .F. ) ;
#70325 = AXIS2_PLACEMENT_3D ( 'NONE', #86639, #58717, #80943 ) ;
#70326 = CARTESIAN_POINT ( 'NONE',  ( 31.71382831265789193, -277.8711922514915500, -301.0311063593334211 ) ) ;
#70327 = ORIENTED_EDGE ( 'NONE', *, *, #14172, .F. ) ;
#70328 = CARTESIAN_POINT ( 'NONE',  ( -33.91173708077440807, -279.6018746095932670, -193.4991491237396417 ) ) ;
#70329 = UNCERTAINTY_MEASURE_WITH_UNIT (LENGTH_MEASURE( 1.000000000000000082E-05 ), #7172, 'distance_accuracy_value', 'NONE');
#70330 = CARTESIAN_POINT ( 'NONE',  ( -43.21404479819425859, -278.0693793825921603, -343.3605975443823013 ) ) ;
#70331 = CARTESIAN_POINT ( 'NONE',  ( 0.6688505955550543280, -276.3117510966048371, -204.5495922861765621 ) ) ;
#70332 = CARTESIAN_POINT ( 'NONE',  ( -76.97180381096681856, -275.5999126088041749, -334.5143685359605570 ) ) ;
#70333 = CARTESIAN_POINT ( 'NONE',  ( -91.92652286646358561, -297.8979031564689990, -221.7361265174787093 ) ) ;
#70334 = AXIS2_PLACEMENT_3D ( 'NONE', #44059, #59223, #88069 ) ;
#70335 = CARTESIAN_POINT ( 'NONE',  ( -99.23866911703809990, -294.5793800156246220, -310.2557597311214863 ) ) ;
#70336 = CARTESIAN_POINT ( 'NONE',  ( 152.9200301536558584, 20.54241773159133899, -11.30461213543805599 ) ) ;
#70337 = CARTESIAN_POINT ( 'NONE',  ( 35.26752485054985442, -281.7215128284715320, -244.7574394713518302 ) ) ;
#70338 = CARTESIAN_POINT ( 'NONE',  ( 29.15513977667851009, -276.1247760911959404, -300.4803856888670452 ) ) ;
#70339 = CIRCLE ( 'NONE', #83953, 28.04691768583012035 ) ;
#70340 = CARTESIAN_POINT ( 'NONE',  ( 25.95881791097069424, -285.6665569705854750, -227.3686180763505149 ) ) ;
#70341 = CARTESIAN_POINT ( 'NONE',  ( -103.8475580135583556, -275.0127505345258783, -235.5793378281366870 ) ) ;
#70342 = LINE ( 'NONE', #13047, #56593 ) ;
#70343 = CARTESIAN_POINT ( 'NONE',  ( 33.85587433152726788, -286.9709573917939451, -287.1987876137876583 ) ) ;
#70344 = CARTESIAN_POINT ( 'NONE',  ( -8.836647185372752844, -278.6701192954755584, -202.0571212369497971 ) ) ;
#70346 = CARTESIAN_POINT ( 'NONE',  ( -79.20627427203412196, -281.7018087495495138, -331.9133041952593999 ) ) ;
#70345 = CARTESIAN_POINT ( 'NONE',  ( -67.53155515161816425, -278.2228937145070518, -203.2359474512934128 ) ) ;
#70347 = CARTESIAN_POINT ( 'NONE',  ( 29.07781926739929190, -289.0895138703878047, -235.4160744100857983 ) ) ;
#70348 = CARTESIAN_POINT ( 'NONE',  ( 14.02009782656586268, -277.5170055668595523, -322.8637408111001719 ) ) ;
#70349 = DIRECTION ( 'NONE',  ( -0.2456588035076220367, 0.9693563597868450898, 0.000000000000000000 ) ) ;
#70350 = CARTESIAN_POINT ( 'NONE',  ( -89.41610783252477290, -293.3193760031869033, -216.3144224936077364 ) ) ;
#70351 = CARTESIAN_POINT ( 'NONE',  ( -39.95090737751955601, -275.3243437782816727, -346.3158716445261689 ) ) ;
#70352 = CARTESIAN_POINT ( 'NONE',  ( 31.36040426466440323, -276.5376682192219278, -295.4865229812849634 ) ) ;
#70353 = CARTESIAN_POINT ( 'NONE',  ( 1.177063809260052718, -284.5392268197408043, -334.9082577420206803 ) ) ;
#70354 = DIRECTION ( 'NONE',  ( 0.000000000000000000, -1.000000000000000000, 0.000000000000000000 ) ) ;
#70355 = CARTESIAN_POINT ( 'NONE',  ( -112.3804373308198592, -292.3538969915509824, -279.6519411409492477 ) ) ;
#70356 = CARTESIAN_POINT ( 'NONE',  ( -109.7278565081622475, -294.8049147501040466, -250.6854236694423435 ) ) ;
#70357 = CARTESIAN_POINT ( 'NONE',  ( -85.40393358707706284, -284.6039895329334399, -210.4096331391698982 ) ) ;
#70358 = CARTESIAN_POINT ( 'NONE',  ( 120.8395553409046528, -299.5541904835127980, -193.1741385666954898 ) ) ;
#70359 = CARTESIAN_POINT ( 'NONE',  ( 0.8831657230102820666, -273.2586099572882290, -207.5908773543315817 ) ) ;
#70360 = CARTESIAN_POINT ( 'NONE',  ( 0.5597263908309599856, -290.7027243267227732, -206.5305034773938928 ) ) ;
#70361 = CARTESIAN_POINT ( 'NONE',  ( 196.9658976021800356, 41.89417665433578009, 12.94436659007928547 ) ) ;
#70362 = CARTESIAN_POINT ( 'NONE',  ( 197.3133474189782248, 24.42324672360810212, 12.74999999999999112 ) ) ;
#70363 = CARTESIAN_POINT ( 'NONE',  ( -109.7666508136769750, -289.3391132043227572, -246.1681118314136256 ) ) ;
#70364 = CARTESIAN_POINT ( 'NONE',  ( -99.69617312076667304, -285.6115192369749707, -309.9328171761367798 ) ) ;
#70365 = CARTESIAN_POINT ( 'NONE',  ( -7.717229398908735938, -284.6748359554690069, -200.3311702558887646 ) ) ;
#70366 = CARTESIAN_POINT ( 'NONE',  ( -94.59180408132135653, -286.6262451252516712, -224.1047848647469323 ) ) ;
#70367 = CARTESIAN_POINT ( 'NONE',  ( -8.200002786311845426, -287.2466821978695179, -203.2540155016641279 ) ) ;
#70368 = CARTESIAN_POINT ( 'NONE',  ( -30.86433191212338656, -294.1133918285856907, -195.2331887625418858 ) ) ;
#70369 = CARTESIAN_POINT ( 'NONE',  ( -15.03852053104803943, -274.8454834371672746, -342.6092616765690764 ) ) ;
#70370 = CARTESIAN_POINT ( 'NONE',  ( 38.70605821425171200, -275.7350446589559283, -258.3395677487113744 ) ) ;
#70371 = CARTESIAN_POINT ( 'NONE',  ( 12.35019880327456399, -290.8176870250891284, -213.4398620582861668 ) ) ;
#70372 = CARTESIAN_POINT ( 'NONE',  ( -108.6564331676212447, -278.1833601874256487, -299.3991766556042649 ) ) ;
#70373 = CARTESIAN_POINT ( 'NONE',  ( -36.96242811806868644, -297.0272377422477916, -345.0176632965091699 ) ) ;
#70374 = CARTESIAN_POINT ( 'NONE',  ( -48.18343439339133027, -248.3668650810961083, -474.9365983928495893 ) ) ;
#70375 = DIRECTION ( 'NONE',  ( -1.000000000000000000, 0.000000000000000000, 0.000000000000000000 ) ) ;
#70376 = CARTESIAN_POINT ( 'NONE',  ( -87.27610497077372997, -282.4502683532564333, -324.3547651650628154 ) ) ;
#70377 = CARTESIAN_POINT ( 'NONE',  ( -106.6543584422696824, -276.9258367037618314, -241.7122778040967432 ) ) ;
#70378 = LINE ( 'NONE', #19228, #45243 ) ;
#70379 = CARTESIAN_POINT ( 'NONE',  ( -34.11298181892665582, -272.5719519753736222, -194.1227868622081871 ) ) ;
#70380 = CARTESIAN_POINT ( 'NONE',  ( -91.04836999871002945, -277.1887992585210441, -320.0279663859444099 ) ) ;
#70381 = CARTESIAN_POINT ( 'NONE',  ( -0.3937189787852397593, -296.0719105576415018, -334.1810671305825053 ) ) ;
#70382 = CARTESIAN_POINT ( 'NONE',  ( 36.69023775462581227, -280.2202080807005018, -250.2921754138708934 ) ) ;
#70383 = CARTESIAN_POINT ( 'NONE',  ( -6.655435022424898150, -295.5803027959955216, -336.8574455707059769 ) ) ;
#70384 = CARTESIAN_POINT ( 'NONE',  ( -50.36697883633235762, -296.5301414763106891, -345.8046382676407120 ) ) ;
#70385 = CARTESIAN_POINT ( 'NONE',  ( 51.67140180705295904, -299.0303371588389041, -197.3637701282314367 ) ) ;
#70386 = CARTESIAN_POINT ( 'NONE',  ( -89.33494695934896868, -293.3208142704036732, -216.2365416088703682 ) ) ;
#70387 = CARTESIAN_POINT ( 'NONE',  ( -18.18407961466337142, -286.4590021806242817, -195.7272952184086989 ) ) ;
#70388 = CARTESIAN_POINT ( 'NONE',  ( 38.39673295420836041, -273.6663299575354245, -268.3623103142480204 ) ) ;
#70389 = CARTESIAN_POINT ( 'NONE',  ( -28.97928851788870475, -288.7823927679049234, -346.9592064938008207 ) ) ;
#70390 = CARTESIAN_POINT ( 'NONE',  ( -107.0593680910357648, -280.8820552013037855, -243.5461288344261561 ) ) ;
#70391 = CARTESIAN_POINT ( 'NONE',  ( -101.1906023740660743, -284.1013890589640596, -234.3862549440055147 ) ) ;
#70392 = CARTESIAN_POINT ( 'NONE',  ( -110.3640301712797509, -288.7716880691907591, -253.2514725013641623 ) ) ;
#70393 = CARTESIAN_POINT ( 'NONE',  ( -107.5887910744927609, -275.4946769126667618, -270.3985833712262092 ) ) ;
#70394 = CARTESIAN_POINT ( 'NONE',  ( 23.58884919973117889, -286.4998199235967036, -229.9525588811646060 ) ) ;
#70395 = CARTESIAN_POINT ( 'NONE',  ( 201.1937845308156341, 300.0127519931331790, -5.237596670121819287 ) ) ;
#70396 = CARTESIAN_POINT ( 'NONE',  ( 22.34789876270433240, -283.1428196582348278, -318.6516454077776643 ) ) ;
#70397 = CARTESIAN_POINT ( 'NONE',  ( -86.35356385484118391, -290.4499913419300583, -211.2103214523775137 ) ) ;
#70398 = CARTESIAN_POINT ( 'NONE',  ( -94.37667358441451881, -280.8440455433234320, -219.8294227883827716 ) ) ;
#70399 = EDGE_CURVE ( 'NONE', #64853, #34296, #60955, .T. ) ;
#70400 = CARTESIAN_POINT ( 'NONE',  ( -112.2382481018925802, -280.0646488581643325, -254.6836037667670780 ) ) ;
#70401 = CARTESIAN_POINT ( 'NONE',  ( 21.33024004803469964, -280.7762299713866696, -226.9050300157267372 ) ) ;
#70402 = CARTESIAN_POINT ( 'NONE',  ( 32.01487516473824968, -277.1783681150890288, -241.6825061669991612 ) ) ;
#70403 = CARTESIAN_POINT ( 'NONE',  ( 23.17167253478684330, -294.1891097677450944, -317.9966791641726331 ) ) ;
#70404 = CARTESIAN_POINT ( 'NONE',  ( -109.9562191162959124, -288.3491720125779239, -287.6521109819722710 ) ) ;
#70405 =( GEOMETRIC_REPRESENTATION_CONTEXT ( 3 ) GLOBAL_UNCERTAINTY_ASSIGNED_CONTEXT ( ( #4574 ) ) GLOBAL_UNIT_ASSIGNED_CONTEXT ( ( #34987, #56311, #50117 ) ) REPRESENTATION_CONTEXT ( 'NONE', 'WORKASPACE' ) );
#70406 = CARTESIAN_POINT ( 'NONE',  ( -82.12211458236384942, -296.3456210552271841, -212.2542148528756911 ) ) ;
#70407 = ORIENTED_EDGE ( 'NONE', *, *, #54121, .T. ) ;
#70408 = ORIENTED_EDGE ( 'NONE', *, *, #41382, .F. ) ;
#70409 = CARTESIAN_POINT ( 'NONE',  ( -2.934474104838156627, -284.5139946081728795, -336.3864382472799548 ) ) ;
#70410 = CARTESIAN_POINT ( 'NONE',  ( -75.67276744759786311, -295.2454202719474665, -332.5716325998578213 ) ) ;
#70411 = CARTESIAN_POINT ( 'NONE',  ( 22.85684462535671102, -293.9935047048724073, -222.8256381593327546 ) ) ;
#70412 = CARTESIAN_POINT ( 'NONE',  ( -10.93121159424621780, -283.3500625993008839, -338.5791273654646147 ) ) ;
#70413 = CARTESIAN_POINT ( 'NONE',  ( 32.34451463327189913, -274.1962932348337745, -238.0374159404958334 ) ) ;
#70414 = CARTESIAN_POINT ( 'NONE',  ( -112.4639845129818951, -290.9978056478661870, -286.7914306978094032 ) ) ;
#70415 = CARTESIAN_POINT ( 'NONE',  ( -67.97920228707845069, -283.7938315207817936, -201.0530431313786721 ) ) ;
#70416 = CARTESIAN_POINT ( 'NONE',  ( -111.9751168400454446, -291.1220455917654704, -251.4507212874577817 ) ) ;
#70417 = CARTESIAN_POINT ( 'NONE',  ( 33.04851782932698256, -287.6288386330920730, -250.9367852337041143 ) ) ;
#70418 = CARTESIAN_POINT ( 'NONE',  ( 73.43068321062709458, -178.2391364535880882, -4.999999999999990230 ) ) ;
#70419 = DIRECTION ( 'NONE',  ( -0.000000000000000000, -1.000000000000000000, -0.000000000000000000 ) ) ;
#70420 = CARTESIAN_POINT ( 'NONE',  ( 173.3795401471607249, 240.5383949446079441, -177.0376500821581089 ) ) ;
#70421 = CARTESIAN_POINT ( 'NONE',  ( -81.14755544000014709, -285.1552235838548199, -332.9054245497384272 ) ) ;
#70422 = CARTESIAN_POINT ( 'NONE',  ( 21.31550574532286291, -290.4094976428776249, -223.6242672951989618 ) ) ;
#70423 = EDGE_LOOP ( 'NONE', ( #4684, #12191, #68630, #8981 ) ) ;
#70424 = CARTESIAN_POINT ( 'NONE',  ( 20.76934989462517933, -279.8459479456881809, -225.6491903601987872 ) ) ;
#70425 = CARTESIAN_POINT ( 'NONE',  ( 35.17962102336328911, -275.5465393844146433, -296.3329793798410492 ) ) ;
#70426 = CARTESIAN_POINT ( 'NONE',  ( -107.9866991209911475, -280.2301735140410983, -295.2023742165029034 ) ) ;
#70427 = CARTESIAN_POINT ( 'NONE',  ( -20.06228311212446158, -109.6411408614775098, -360.8968400945585131 ) ) ;
#70428 = CARTESIAN_POINT ( 'NONE',  ( 26.22158160618183231, -280.6893963199886457, -312.7676682769504737 ) ) ;
#70429 = CARTESIAN_POINT ( 'NONE',  ( -90.82413384932404199, -283.3093974308474685, -218.2151351854687391 ) ) ;
#70430 = CARTESIAN_POINT ( 'NONE',  ( -112.7716210525488094, -298.4286507919750306, -261.1795580784037156 ) ) ;
#70431 = CARTESIAN_POINT ( 'NONE',  ( 12.94097172995459211, -293.2699203188096249, -217.3550678338742443 ) ) ;
#70432 = ORIENTED_EDGE ( 'NONE', *, *, #5214, .F. ) ;
#70433 = CARTESIAN_POINT ( 'NONE',  ( -109.6671955743595817, -289.0659965806693208, -283.4097266189107813 ) ) ;
#70434 = CARTESIAN_POINT ( 'NONE',  ( -45.63037386966995257, -277.8058605918876651, -346.8641594955472556 ) ) ;
#70435 = CARTESIAN_POINT ( 'NONE',  ( -36.48553719244878124, -298.2298444201506413, -197.3610928647055971 ) ) ;
#70436 = ORIENTED_EDGE ( 'NONE', *, *, #62500, .F. ) ;
#70437 = CARTESIAN_POINT ( 'NONE',  ( -93.90793867459910871, -272.1798830500507620, -218.5560862486163387 ) ) ;
#70438 = CARTESIAN_POINT ( 'NONE',  ( 142.6449502718966755, -0.9999999999999991118, 22.50000000000000000 ) ) ;
#70439 = CARTESIAN_POINT ( 'NONE',  ( 222.8344101925596306, -44.55766379199611293, -22.08578643762690419 ) ) ;
#70440 = CARTESIAN_POINT ( 'NONE',  ( 33.95398569155008772, -282.8566693598043003, -287.4777196629380001 ) ) ;
#70441 = CARTESIAN_POINT ( 'NONE',  ( 5.592988562297290578, -282.3851735003717636, -207.6667281306568213 ) ) ;
#70442 = CARTESIAN_POINT ( 'NONE',  ( -100.6104141097120248, -283.1063119040639435, -307.2457798186815126 ) ) ;
#70443 = CARTESIAN_POINT ( 'NONE',  ( -37.02646435070128206, -281.9165565869342345, -196.1265834965426791 ) ) ;
#70444 = CARTESIAN_POINT ( 'NONE',  ( 34.51409877170166141, -273.8176575088681375, -253.9506748952433099 ) ) ;
#70445 = ADVANCED_FACE ( 'NONE', ( #44916 ), #74272, .T. ) ;
#70446 = CARTESIAN_POINT ( 'NONE',  ( 194.4755092218382799, 40.71494654549765357, 14.33893281099658346 ) ) ;
#70447 = CARTESIAN_POINT ( 'NONE',  ( -72.75714463488614570, -278.3119017690627857, -338.5660027969175303 ) ) ;
#70448 = VERTEX_POINT ( 'NONE', #17462 ) ;
#70449 = VERTEX_POINT ( 'NONE', #80917 ) ;
#70450 = DIRECTION ( 'NONE',  ( 0.000000000000000000, 0.000000000000000000, 1.000000000000000000 ) ) ;
#70451 = CARTESIAN_POINT ( 'NONE',  ( -113.0926791583531781, -286.4528732810155134, -267.1901203344636997 ) ) ;
#70452 = CARTESIAN_POINT ( 'NONE',  ( 35.58457702316624705, -292.8264702047973174, -276.2228436234940432 ) ) ;
#70453 = CARTESIAN_POINT ( 'NONE',  ( 10.15845928634537820, -287.7655187065291784, -330.9023823249069096 ) ) ;
#70454 = CARTESIAN_POINT ( 'NONE',  ( -41.35578234679477561, -284.2408107500264123, -196.4440404413563499 ) ) ;
#70456 = CARTESIAN_POINT ( 'NONE',  ( -71.66228721505896715, -287.7519132252717213, -335.9503674799708506 ) ) ;
#70455 = CARTESIAN_POINT ( 'NONE',  ( -108.9345668287926401, -283.3503187269599835, -253.2823250766483909 ) ) ;
#70457 = CARTESIAN_POINT ( 'NONE',  ( -96.23120351448213228, -285.1460434797748462, -314.1693009701115784 ) ) ;
#70458 = CARTESIAN_POINT ( 'NONE',  ( 18.37392987649216991, -274.2519160757052532, -320.5875924219042190 ) ) ;
#70459 = CARTESIAN_POINT ( 'NONE',  ( -33.74449561457781499, -284.4965878972702171, -194.2460699548436480 ) ) ;
#70460 = CARTESIAN_POINT ( 'NONE',  ( -36.59203453992425636, -300.0616930923462178, -195.3608536800668105 ) ) ;
#70461 = CARTESIAN_POINT ( 'NONE',  ( -66.45489673066794012, -283.6716376144769924, -201.0614050545398186 ) ) ;
#70462 = CARTESIAN_POINT ( 'NONE',  ( 32.95709836510569346, -282.2226865089769490, -249.8309601934315936 ) ) ;
#70463 = CARTESIAN_POINT ( 'NONE',  ( 36.86922392046123065, -289.7094520682850316, -282.6267391372953171 ) ) ;
#70464 = CARTESIAN_POINT ( 'NONE',  ( -48.18343439339133027, -283.1093320178187582, -502.6442049081569508 ) ) ;
#70465 = CARTESIAN_POINT ( 'NONE',  ( -2.607253171737097919, -296.5165584644005889, -337.4642654165792806 ) ) ;
#70466 = CARTESIAN_POINT ( 'NONE',  ( -34.20486192780585100, -278.0914102157768752, -195.4138537235818376 ) ) ;
#70467 = CARTESIAN_POINT ( 'NONE',  ( -104.4639435055522085, -290.2352048047389985, -232.9610743457317028 ) ) ;
#70468 = CARTESIAN_POINT ( 'NONE',  ( -66.38654922876303033, -293.8388077363383672, -338.2053303899429011 ) ) ;
#70469 = CARTESIAN_POINT ( 'NONE',  ( -107.6943845293313871, -277.5164906040081974, -249.1068648560783743 ) ) ;
#70470 = CARTESIAN_POINT ( 'NONE',  ( -39.17548730034383198, -296.1685143501420043, -196.1359479003110096 ) ) ;
#70471 = CARTESIAN_POINT ( 'NONE',  ( 35.78425105212308921, -294.7647574848086265, -262.5328525572728040 ) ) ;
#70472 = CARTESIAN_POINT ( 'NONE',  ( 35.78497577281001440, -290.2662352645559167, -287.0191576251351080 ) ) ;
#70473 = CARTESIAN_POINT ( 'NONE',  ( -113.6444734326017283, -295.0417619637821076, -269.5900557760484730 ) ) ;
#70474 = CARTESIAN_POINT ( 'NONE',  ( 4.080296576367366868, -290.0842725910494551, -331.5018673095632948 ) ) ;
#70475 = CARTESIAN_POINT ( 'NONE',  ( 33.52598945148352527, -291.4383954758265531, -242.7976370683088874 ) ) ;
#70476 = CARTESIAN_POINT ( 'NONE',  ( -105.2537969564822333, -292.3561414895329449, -241.8854979274368588 ) ) ;
#70477 = DIRECTION ( 'NONE',  ( 1.000000000000000000, 0.000000000000000000, 0.000000000000000000 ) ) ;
#70478 = CARTESIAN_POINT ( 'NONE',  ( -70.30260065243886913, -292.4089624490845836, -205.0451110309617491 ) ) ;
#70479 = CARTESIAN_POINT ( 'NONE',  ( 175.2296996224750103, 149.6461846693799487, 0.000000000000000000 ) ) ;
#70480 = CARTESIAN_POINT ( 'NONE',  ( -110.0588545373884273, -292.0638715102076617, -246.1071754726964116 ) ) ;
#70482 = CARTESIAN_POINT ( 'NONE',  ( 35.42443431690416134, -293.6291734838542311, -276.1997546328657904 ) ) ;
#70481 = CARTESIAN_POINT ( 'NONE',  ( 16.63022849512995194, -280.3097522843655725, -323.0230798578372742 ) ) ;
#70483 = CARTESIAN_POINT ( 'NONE',  ( 39.64064422321507664, -281.5108343277557879, -267.0573769879011365 ) ) ;
#70484 = CARTESIAN_POINT ( 'NONE',  ( -105.7672995175042701, -283.7629100493165311, -305.7433051657801002 ) ) ;
#70485 = CARTESIAN_POINT ( 'NONE',  ( -34.53410916004471432, -287.0167631654152842, -345.1925978278831622 ) ) ;
#70486 = CARTESIAN_POINT ( 'NONE',  ( -74.43418150951416123, -281.6902171684786254, -334.7237745564837041 ) ) ;
#70487 = CARTESIAN_POINT ( 'NONE',  ( -88.50284191313016890, -283.3351405266946017, -215.4494796820675901 ) ) ;
#70488 = FACE_BOUND ( 'NONE', #82906, .T. ) ;
#70489 = CARTESIAN_POINT ( 'NONE',  ( -11.72372324553491829, -278.8595073497788803, -198.4277721252866797 ) ) ;
#70490 = CARTESIAN_POINT ( 'NONE',  ( 2.591835866407439237, -285.4947844899659799, -204.8874193511742590 ) ) ;
#70491 = CARTESIAN_POINT ( 'NONE',  ( 195.5093152655051938, 40.06852958779855811, 14.92626378859575809 ) ) ;
#70492 = CARTESIAN_POINT ( 'NONE',  ( -14.61923420005219754, -293.9517609463957797, -200.1462338332117383 ) ) ;
#70493 = CARTESIAN_POINT ( 'NONE',  ( 0.8848012538291770701, -275.9769362108248174, -204.1844758618515527 ) ) ;
#70494 = CARTESIAN_POINT ( 'NONE',  ( -105.2890244228423740, -277.8613220640744430, -297.1052501967619150 ) ) ;
#70495 = CARTESIAN_POINT ( 'NONE',  ( -64.39079182615223829, -291.8755264076513640, -198.2123187016681527 ) ) ;
#70496 = CARTESIAN_POINT ( 'NONE',  ( -63.43805831982277255, -281.4694368201828070, -341.2715846753409892 ) ) ;
#70497 = EDGE_CURVE ( 'NONE', #64642, #9910, #68518, .T. ) ;
#70498 = CARTESIAN_POINT ( 'NONE',  ( -34.83726953145153260, -291.1431283816995688, -197.1686574687067264 ) ) ;
#70499 = CARTESIAN_POINT ( 'NONE',  ( -90.20725363860721302, -295.3043287389435250, -217.1611753172365127 ) ) ;
#70500 = ORIENTED_EDGE ( 'NONE', *, *, #74108, .T. ) ;
#70501 = CARTESIAN_POINT ( 'NONE',  ( 157.4851178187871312, 1.000000000000000888, -7.000000000000000888 ) ) ;
#70502 = CARTESIAN_POINT ( 'NONE',  ( 14.92391109133455984, -292.3211182338945946, -219.2367707040171467 ) ) ;
#70503 = CARTESIAN_POINT ( 'NONE',  ( 208.0345994753939181, 28.60382334453963082, 12.94649967097967647 ) ) ;
#70504 = CARTESIAN_POINT ( 'NONE',  ( -102.0455923789670294, -275.6237833571633473, -301.4846348637937581 ) ) ;
#70505 = CARTESIAN_POINT ( 'NONE',  ( -96.33830285497202794, -294.9480838607117335, -319.4959286018274724 ) ) ;
#70506 = CARTESIAN_POINT ( 'NONE',  ( -9.295961007020183686, -278.5544922487031840, -199.9782933864558458 ) ) ;
#70507 = CARTESIAN_POINT ( 'NONE',  ( -102.1099567258476810, -286.4039964930817632, -229.6380138591213438 ) ) ;
#70508 = CARTESIAN_POINT ( 'NONE',  ( 4.727098966536575020, -286.4710138708360319, -210.6400924584868619 ) ) ;
#70509 = CARTESIAN_POINT ( 'NONE',  ( -4.742113838513839497, -278.1349480867809234, -336.4657971616366581 ) ) ;
#70510 = CARTESIAN_POINT ( 'NONE',  ( -83.39395379547509890, -293.7065546999000958, -329.1725608119978119 ) ) ;
#70511 = CARTESIAN_POINT ( 'NONE',  ( -91.12843962527867347, -297.5892523712590219, -321.2774091184696204 ) ) ;
#70512 = CARTESIAN_POINT ( 'NONE',  ( -91.26997362820775095, -276.6352260836397932, -320.2233339681659459 ) ) ;
#70513 = VERTEX_POINT ( 'NONE', #73364 ) ;
#70514 = CARTESIAN_POINT ( 'NONE',  ( 194.8940620914166573, 40.53306711095739701, 13.77184909798794621 ) ) ;
#70515 = CARTESIAN_POINT ( 'NONE',  ( -90.70047796957018704, -295.4502669847406082, -325.9195091387227876 ) ) ;
#70516 = CARTESIAN_POINT ( 'NONE',  ( -71.81839302994913510, -291.4316134962004980, -336.3502989366946849 ) ) ;
#70517 = CARTESIAN_POINT ( 'NONE',  ( 197.7129307445490269, 68.09401877024910732, -12.80442219784224811 ) ) ;
#70518 = ADVANCED_FACE ( 'NONE', ( #87996 ), #53428, .T. ) ;
#70519 = CARTESIAN_POINT ( 'NONE',  ( 16.09113264438434854, -288.9207513429436744, -320.3233196171364625 ) ) ;
#70520 = ORIENTED_EDGE ( 'NONE', *, *, #69090, .T. ) ;
#70521 = CARTESIAN_POINT ( 'NONE',  ( -39.56838718495048113, -279.0836178488788164, -193.6157013656127504 ) ) ;
#70522 = CARTESIAN_POINT ( 'NONE',  ( -98.18870956582244958, -296.5750772831426048, -317.3819030626211770 ) ) ;
#70523 = CARTESIAN_POINT ( 'NONE',  ( -111.9514636064411093, -288.8592497763979168, -257.1820180260689881 ) ) ;
#70524 = CARTESIAN_POINT ( 'NONE',  ( -99.90684308770038058, -297.4798921422525382, -225.5130725624387082 ) ) ;
#70525 = CARTESIAN_POINT ( 'NONE',  ( 28.41543976323979592, -294.3163836630541255, -302.2281114412960505 ) ) ;
#70526 = DIRECTION ( 'NONE',  ( -0.000000000000000000, -0.000000000000000000, 1.000000000000000000 ) ) ;
#70527 = FILL_AREA_STYLE ('',( #34062 ) ) ;
#70528 = DIRECTION ( 'NONE',  ( -1.000000000000000000, 0.000000000000000000, 0.000000000000000000 ) ) ;
#70529 = CARTESIAN_POINT ( 'NONE',  ( 26.87191746113027335, -289.6190549378038668, -311.6813801045261130 ) ) ;
#70530 = CARTESIAN_POINT ( 'NONE',  ( 40.64545035920995986, -277.8376638359844719, -252.5284128619064461 ) ) ;
#70531 = ORIENTED_EDGE ( 'NONE', *, *, #82892, .T. ) ;
#70532 = CARTESIAN_POINT ( 'NONE',  ( 36.50415773423206645, -280.6308635198334400, -248.8639039775103754 ) ) ;
#70533 = CARTESIAN_POINT ( 'NONE',  ( -111.3065374100586382, -286.4017563320265936, -282.0608388809010876 ) ) ;
#70534 = CARTESIAN_POINT ( 'NONE',  ( 7.215181859690259714, -285.2204900623581807, -208.2210605758807276 ) ) ;
#70535 = CARTESIAN_POINT ( 'NONE',  ( -91.50643881267039603, -271.2786216153082250, -218.7070261488613028 ) ) ;
#70536 = CARTESIAN_POINT ( 'NONE',  ( -109.7568286238355455, -288.4089004734184414, -287.6053450330914529 ) ) ;
#70537 = CARTESIAN_POINT ( 'NONE',  ( 28.04214118035680769, -277.9189128043040000, -308.6398166849419908 ) ) ;
#70538 = ORIENTED_EDGE ( 'NONE', *, *, #55137, .F. ) ;
#70540 = CARTESIAN_POINT ( 'NONE',  ( -35.65213787455041228, -279.4224568114539125, -197.2662921318444376 ) ) ;
#70539 = CARTESIAN_POINT ( 'NONE',  ( -95.27301981713750934, -277.9272385251546211, -314.7791571005171249 ) ) ;
#70541 = CARTESIAN_POINT ( 'NONE',  ( 5.709167299155815556, -277.5632098443919062, -333.8285531193897668 ) ) ;
#70542 = CARTESIAN_POINT ( 'NONE',  ( -112.1002724823039216, -277.1370401253649902, -287.0693369216727433 ) ) ;
#70543 = CARTESIAN_POINT ( 'NONE',  ( -104.5224035930334026, -253.8871293345330571, -324.9516776915779133 ) ) ;
#70544 = CARTESIAN_POINT ( 'NONE',  ( -24.21168110473835355, -275.1569922701014548, -194.6736417776367318 ) ) ;
#70545 = CARTESIAN_POINT ( 'NONE',  ( -111.7713335972482156, -274.2845451784580746, -253.5403743149537945 ) ) ;
#70546 = CARTESIAN_POINT ( 'NONE',  ( -69.85430415644619018, -285.9805209788416391, -337.9475929042657754 ) ) ;
#70547 = EDGE_LOOP ( 'NONE', ( #58897, #72051, #79973, #69930 ) ) ;
#70548 = CARTESIAN_POINT ( 'NONE',  ( 82.65974748999957455, -298.7023692776643315, -193.0048141087816873 ) ) ;
#70549 = CARTESIAN_POINT ( 'NONE',  ( 28.51143791346287060, -289.0663006257602774, -302.5727662283608197 ) ) ;
#70550 = CARTESIAN_POINT ( 'NONE',  ( 38.56404369920143438, -289.2551970462341728, -265.8558366280998939 ) ) ;
#70551 = CARTESIAN_POINT ( 'NONE',  ( 29.51492657283014154, -287.2995634214986467, -300.0515900678584558 ) ) ;
#70552 = CARTESIAN_POINT ( 'NONE',  ( -113.4256106562333173, -284.2073298583755445, -258.5747209378415050 ) ) ;
#70553 = CARTESIAN_POINT ( 'NONE',  ( -54.66097731631204226, -278.2258574878790114, -198.5693601604544085 ) ) ;
#70554 = CARTESIAN_POINT ( 'NONE',  ( -88.56362733314142588, -287.1848107600865205, -216.6286357019850470 ) ) ;
#70555 = CARTESIAN_POINT ( 'NONE',  ( 21.89775871414668984, -279.4230068406447458, -226.5061608593920255 ) ) ;
#70556 = CARTESIAN_POINT ( 'NONE',  ( -110.6517425572639581, -279.9352688195127143, -265.1764139382601684 ) ) ;
#70557 = CARTESIAN_POINT ( 'NONE',  ( -74.03876740984465243, -278.0463375420149532, -333.5379625905061971 ) ) ;
#70558 = CARTESIAN_POINT ( 'NONE',  ( 0.5096636765602601260, -287.3546639809325711, -337.0189745407465693 ) ) ;
#70559 = CARTESIAN_POINT ( 'NONE',  ( 4.466430853208652962, -283.3067222230526454, -334.8929082276620761 ) ) ;
#70560 = CARTESIAN_POINT ( 'NONE',  ( -102.4697208731003002, -285.5813023078417814, -229.3993331460938521 ) ) ;
#70561 = CARTESIAN_POINT ( 'NONE',  ( 22.58598527377359844, -282.2998419389450646, -312.0465174275540221 ) ) ;
#70562 = EDGE_LOOP ( 'NONE', ( #29982, #87042, #24278, #27694 ) ) ;
#70563 = ORIENTED_EDGE ( 'NONE', *, *, #40622, .T. ) ;
#70564 = CARTESIAN_POINT ( 'NONE',  ( 200.2349812190172713, 66.43136063442170780, 7.741079165001067963 ) ) ;
#70565 = CARTESIAN_POINT ( 'NONE',  ( -14.00086639007882283, -291.0334651374545842, -197.4460178483741402 ) ) ;
#70566 = CARTESIAN_POINT ( 'NONE',  ( 9.645194837510528529, -273.7757085634275995, -214.1196150562338403 ) ) ;
#70567 = CARTESIAN_POINT ( 'NONE',  ( -5.847044738855327495, -293.9974277255686275, -340.5138048082750970 ) ) ;
#70568 = CARTESIAN_POINT ( 'NONE',  ( -53.57996250580212916, -287.7441635392947319, -342.2431504067977812 ) ) ;
#70569 = CARTESIAN_POINT ( 'NONE',  ( -3.148454756994365500, -290.7501947822848933, -204.7196982342544800 ) ) ;
#70570 = CARTESIAN_POINT ( 'NONE',  ( -68.91495787515356142, -290.6819340885292604, -336.6201543584406295 ) ) ;
#70571 = DIRECTION ( 'NONE',  ( 0.000000000000000000, 1.000000000000000000, 0.000000000000000000 ) ) ;
#70572 = CARTESIAN_POINT ( 'NONE',  ( -111.2068297495384712, -292.7192025140495275, -257.3632998353992889 ) ) ;
#70573 = CARTESIAN_POINT ( 'NONE',  ( -61.08474469181454225, -289.7446191069391830, -198.9880305177079549 ) ) ;
#70574 = CARTESIAN_POINT ( 'NONE',  ( 20.74891257241985087, -294.8983806487808579, -222.9019554595395505 ) ) ;
#70575 = CARTESIAN_POINT ( 'NONE',  ( -22.42358052685474235, -287.1889949089036236, -198.6092940153311019 ) ) ;
#70576 = CARTESIAN_POINT ( 'NONE',  ( -37.65514352323639713, -297.0561888998693689, -345.5399029053422737 ) ) ;
#70577 = CARTESIAN_POINT ( 'NONE',  ( 193.9646936176702070, 21.00000000000000000, 15.00000000000000000 ) ) ;
#70578 = CARTESIAN_POINT ( 'NONE',  ( -3.323129829970142168, -276.4789223926416071, -203.1072809199720837 ) ) ;
#70579 = CARTESIAN_POINT ( 'NONE',  ( -114.2394590020185916, -271.9367054066718197, -267.4891729012607016 ) ) ;
#70580 = CARTESIAN_POINT ( 'NONE',  ( -11.11039515779607001, -272.6384964782828320, -201.0972641572010104 ) ) ;
#70581 = CARTESIAN_POINT ( 'NONE',  ( -100.4078346138884825, -276.0953483828931780, -310.0045983443858404 ) ) ;
#70582 = CARTESIAN_POINT ( 'NONE',  ( -110.2820711298114276, -273.8644937171459901, -262.1859860191879648 ) ) ;
#70583 = CARTESIAN_POINT ( 'NONE',  ( 36.71864045377575536, -273.8897485159754979, -251.5549422005593954 ) ) ;
#70584 = CARTESIAN_POINT ( 'NONE',  ( -80.48567844983057284, -297.0752971806296046, -329.9763178078274564 ) ) ;
#70585 = DIRECTION ( 'NONE',  ( 0.000000000000000000, 0.000000000000000000, -1.000000000000000000 ) ) ;
#70586 = CARTESIAN_POINT ( 'NONE',  ( -75.30315452064391479, -298.3352225353988842, -207.7601539663718881 ) ) ;
#70587 = CARTESIAN_POINT ( 'NONE',  ( 104.1964229570258311, -299.5541904835127980, -197.2570935515975918 ) ) ;
#70589 = CARTESIAN_POINT ( 'NONE',  ( -70.46754843473301833, -297.6027994932200613, -205.2958560991954187 ) ) ;
#70588 = CARTESIAN_POINT ( 'NONE',  ( 37.16323037804039586, -285.4269053045680380, -258.9868763035073016 ) ) ;
#70590 = CARTESIAN_POINT ( 'NONE',  ( 22.99188654876190441, -286.9117271993318354, -222.4980882501235442 ) ) ;
#70591 = CARTESIAN_POINT ( 'NONE',  ( -23.31995607027534589, -288.5444258586746855, -346.1062668668715219 ) ) ;
#70592 = CARTESIAN_POINT ( 'NONE',  ( -107.8886063954649757, -298.1879848769862633, -296.9948174597930688 ) ) ;
#70593 = CARTESIAN_POINT ( 'NONE',  ( 20.22756712470414087, -292.2135310225754097, -318.1712413682008673 ) ) ;
#70594 = CARTESIAN_POINT ( 'NONE',  ( 24.11978028618081638, -281.3644002837964422, -316.4766820177440536 ) ) ;
#70595 = CARTESIAN_POINT ( 'NONE',  ( -20.19161114001082069, -283.7666405000204009, -195.3683826091709363 ) ) ;
#70596 = CARTESIAN_POINT ( 'NONE',  ( 201.2104617360081704, 250.0000000000000568, 15.00000000000000000 ) ) ;
#70597 = CARTESIAN_POINT ( 'NONE',  ( -53.51085341094929504, -288.0591590709166212, -341.9550352222351535 ) ) ;
#70598 = LINE ( 'NONE', #19448, #3362 ) ;
#70599 = CARTESIAN_POINT ( 'NONE',  ( -34.52779919839132816, -287.0167631635330849, -345.3592581997543220 ) ) ;
#70600 = CARTESIAN_POINT ( 'NONE',  ( -35.13795689164769698, -299.6803177653247872, -196.5604998867146662 ) ) ;
#70601 = CARTESIAN_POINT ( 'NONE',  ( -31.13982462235754767, -281.5541829127319033, -194.1501602831974367 ) ) ;
#70603 = CARTESIAN_POINT ( 'NONE',  ( -13.52936602132302646, -282.7343400366372066, -339.4217709840478960 ) ) ;
#70602 = CARTESIAN_POINT ( 'NONE',  ( -76.25493553000536906, -293.5892621223344463, -334.9521914411866419 ) ) ;
#70604 = CARTESIAN_POINT ( 'NONE',  ( -113.9430046164710291, -296.6209616882620139, -278.1867269155716826 ) ) ;
#70605 = CARTESIAN_POINT ( 'NONE',  ( -39.20508215459190637, -299.5485054782038787, -196.6788177819891814 ) ) ;
#70606 = CARTESIAN_POINT ( 'NONE',  ( 37.41608068887489935, -283.4749831315580195, -264.3382570356354790 ) ) ;
#70607 = EDGE_CURVE ( 'NONE', #76418, #72836, #53363, .T. ) ;
#70608 = CARTESIAN_POINT ( 'NONE',  ( -44.58045220042586010, -297.0171962089432895, -197.4339045375737953 ) ) ;
#70609 = ORIENTED_EDGE ( 'NONE', *, *, #14384, .F. ) ;
#70610 = DIRECTION ( 'NONE',  ( 0.000000000000000000, 0.000000000000000000, 1.000000000000000000 ) ) ;
#70611 = CARTESIAN_POINT ( 'NONE',  ( -76.97965838967209606, -285.5654508912245433, -333.6731560313812111 ) ) ;
#70612 = CARTESIAN_POINT ( 'NONE',  ( 140.6539576904058606, 275.0000000000000568, 10.50000000000000000 ) ) ;
#70613 = CARTESIAN_POINT ( 'NONE',  ( 25.18497378105905682, -279.6952119285918457, -320.2651865833026363 ) ) ;
#70614 = CARTESIAN_POINT ( 'NONE',  ( 0.9576560570261686278, -275.7521778843654943, -337.0346634714132961 ) ) ;
#70615 = CARTESIAN_POINT ( 'NONE',  ( -20.07010538936605926, -292.1135301807131555, -199.3814768179931320 ) ) ;
#70616 = CARTESIAN_POINT ( 'NONE',  ( -48.41393097179969374, -284.7157729575237113, -343.2179190051014075 ) ) ;
#70617 = CARTESIAN_POINT ( 'NONE',  ( 19.81396966363418954, -277.8063247213278828, -317.0679731432012431 ) ) ;
#70618 = CARTESIAN_POINT ( 'NONE',  ( -67.63096305686403298, -284.8671335737280401, -340.5121468077363716 ) ) ;
#70619 = CARTESIAN_POINT ( 'NONE',  ( -61.68079291410877119, -282.1703689347894510, -339.6587028862649049 ) ) ;
#70620 = CARTESIAN_POINT ( 'NONE',  ( -43.95207306985640372, -281.9688793268086329, -195.6013848918130975 ) ) ;
#70621 = CARTESIAN_POINT ( 'NONE',  ( 37.28470295454496153, -275.4814433800626148, -251.3900882931308729 ) ) ;
#70622 = CARTESIAN_POINT ( 'NONE',  ( 37.90522360908004629, -275.5905612598006087, -286.7598025223084051 ) ) ;
#70623 = CARTESIAN_POINT ( 'NONE',  ( -109.6929327665311718, -298.2450868897143437, -287.9251779765749006 ) ) ;
#70624 = DIRECTION ( 'NONE',  ( 1.000000000000000000, 0.000000000000000000, 0.000000000000000000 ) ) ;
#70625 = EDGE_CURVE ( 'NONE', #79604, #60489, #52032, .T. ) ;
#70626 = CARTESIAN_POINT ( 'NONE',  ( 185.8264795993290477, 214.9910457053126720, 23.09031830825835385 ) ) ;
#70627 = CARTESIAN_POINT ( 'NONE',  ( -94.66276608479341803, -294.0115916068578485, -319.9050467741159878 ) ) ;
#70628 = CARTESIAN_POINT ( 'NONE',  ( 35.70455869101828483, -275.0401079366844783, -268.8669580202108591 ) ) ;
#70629 = CARTESIAN_POINT ( 'NONE',  ( 34.83696766509952170, -295.3889646272189111, -295.2809408000693452 ) ) ;
#70630 = CARTESIAN_POINT ( 'NONE',  ( -0.8815773038446524934, -295.7841761692653222, -337.7455661287014550 ) ) ;
#70631 = CARTESIAN_POINT ( 'NONE',  ( -71.06925274681060500, -293.6060966429259338, -203.5593169245541390 ) ) ;
#70632 = CARTESIAN_POINT ( 'NONE',  ( -96.74345866326923726, -275.9274016480878799, -315.8744073948667506 ) ) ;
#70633 = CARTESIAN_POINT ( 'NONE',  ( -110.9115808234451919, -280.3255004165364426, -281.7095475203002479 ) ) ;
#70634 = CARTESIAN_POINT ( 'NONE',  ( -111.4822010659440963, -294.7254598494309903, -263.1360414614928231 ) ) ;
#70635 = CARTESIAN_POINT ( 'NONE',  ( -13.78315774987723508, -284.6100173665847706, -342.3701490817223316 ) ) ;
#70636 = CARTESIAN_POINT ( 'NONE',  ( -85.92074389041499671, -284.2809209862342072, -215.3906168898256510 ) ) ;
#70637 = CARTESIAN_POINT ( 'NONE',  ( 175.7436469805359138, 241.6859982463862764, -179.0910351515699404 ) ) ;
#70638 = ORIENTED_EDGE ( 'NONE', *, *, #16017, .F. ) ;
#70639 = CARTESIAN_POINT ( 'NONE',  ( -108.3850958888772453, -284.4421330787102988, -253.4276063474368925 ) ) ;
#70640 = VERTEX_POINT ( 'NONE', #9873 ) ;
#70641 = CARTESIAN_POINT ( 'NONE',  ( 22.29162071927039079, -283.2812166626516159, -318.6038246925293720 ) ) ;
#70642 = CARTESIAN_POINT ( 'NONE',  ( -85.25255792420603029, -284.2018111161890488, -210.5902352494255183 ) ) ;
#70643 = CARTESIAN_POINT ( 'NONE',  ( -113.0065967426592692, -279.6558260396728883, -257.4133910178989595 ) ) ;
#70644 = CARTESIAN_POINT ( 'NONE',  ( -67.41735561851342595, -278.9596546773233854, -340.4907315612996968 ) ) ;
#70645 = CARTESIAN_POINT ( 'NONE',  ( -19.78756432573599255, -280.9233879431179162, -195.4387709399019286 ) ) ;
#70646 = CARTESIAN_POINT ( 'NONE',  ( -67.68488546085839630, -271.1237833571632905, -207.2794874003663779 ) ) ;
#70647 = CARTESIAN_POINT ( 'NONE',  ( 154.9793621001980171, 206.4414210594577810, -217.3080705048732000 ) ) ;
#70648 = CARTESIAN_POINT ( 'NONE',  ( -65.27622544172163543, -275.6864015259907319, -200.9233048794513081 ) ) ;
#70649 = CARTESIAN_POINT ( 'NONE',  ( -56.72725910259299553, -169.1093196520039896, -364.2234470880441677 ) ) ;
#70650 = CARTESIAN_POINT ( 'NONE',  ( -16.43746510500518454, -278.3437527998024734, -198.7031822165723440 ) ) ;
#70651 = CARTESIAN_POINT ( 'NONE',  ( -33.61182275531538721, -293.8586316445739044, -194.4660454823589646 ) ) ;
#70652 = CARTESIAN_POINT ( 'NONE',  ( -73.35984233925489661, -294.8920769460565907, -333.9739005027352050 ) ) ;
#70653 = CARTESIAN_POINT ( 'NONE',  ( -91.55961797117340950, -289.3066363431200898, -325.0249355406274390 ) ) ;
#70654 = DIRECTION ( 'NONE',  ( 0.000000000000000000, 0.000000000000000000, 1.000000000000000000 ) ) ;
#70656 = CARTESIAN_POINT ( 'NONE',  ( -44.07732395128466862, -284.3654367520975370, -196.8691334757363336 ) ) ;
#70655 = CARTESIAN_POINT ( 'NONE',  ( -108.3343685712820843, -295.4897563664371205, -241.9586675408789631 ) ) ;
#70657 = CARTESIAN_POINT ( 'NONE',  ( -104.6866562303662960, -292.8271419034650762, -239.1277645757311348 ) ) ;
#70658 = CARTESIAN_POINT ( 'NONE',  ( -91.89848163743893394, -286.5684738427502793, -221.0440507880120720 ) ) ;
#70659 = ORIENTED_EDGE ( 'NONE', *, *, #21995, .T. ) ;
#70660 = CARTESIAN_POINT ( 'NONE',  ( -97.28736398845788358, -292.1376555841567892, -222.4097092588899898 ) ) ;
#70661 = CARTESIAN_POINT ( 'NONE',  ( 33.02040192359089588, -282.3043472551283912, -290.0375769284212311 ) ) ;
#70662 = CARTESIAN_POINT ( 'NONE',  ( -5.974399706019373646, -293.4438547410977662, -340.2474627434253307 ) ) ;
#70663 = CARTESIAN_POINT ( 'NONE',  ( -34.66219235671446341, -289.8221113137282714, -347.1529082926700767 ) ) ;
#70664 = CARTESIAN_POINT ( 'NONE',  ( -113.6060034133675032, -291.1765843419334487, -259.8080197763021602 ) ) ;
#70665 = CARTESIAN_POINT ( 'NONE',  ( 34.96066830824933191, -287.8528494374757543, -280.5202924721663749 ) ) ;
#70666 = ORIENTED_EDGE ( 'NONE', *, *, #89671, .T. ) ;
#70667 = CARTESIAN_POINT ( 'NONE',  ( 222.8344101925596306, 7.222594520736746447E-16, 22.08578643762690419 ) ) ;
#70668 = CARTESIAN_POINT ( 'NONE',  ( -111.0777919943166836, -298.6339279672222915, -252.9457729987560413 ) ) ;
#70669 = CARTESIAN_POINT ( 'NONE',  ( -30.52231065812785005, -296.8206805055173731, -193.8557524509169241 ) ) ;
#70670 = CARTESIAN_POINT ( 'NONE',  ( 32.96382175207060072, -280.3404865373345842, -249.8539962539578028 ) ) ;
#70671 = EDGE_LOOP ( 'NONE', ( #10873, #21814, #10530, #32586, #66699 ) ) ;
#70672 = CARTESIAN_POINT ( 'NONE',  ( 7.922900236742358437, -297.9535122079532243, -193.4678911002017969 ) ) ;
#70673 = CARTESIAN_POINT ( 'NONE',  ( -89.00156356406070302, -294.2738993897837645, -322.9872633757727272 ) ) ;
#70674 = CARTESIAN_POINT ( 'NONE',  ( 17.29411997095717268, -278.0188502902738605, -320.3089888615491532 ) ) ;
#70675 = CARTESIAN_POINT ( 'NONE',  ( -59.82760629727908253, -271.8974409596727355, -199.5595195205677896 ) ) ;
#70676 = CARTESIAN_POINT ( 'NONE',  ( -7.814561675065936797, -295.8614746109129214, -337.5705935758317651 ) ) ;
#70677 = CARTESIAN_POINT ( 'NONE',  ( -4.184601490418486947, -295.6840477155105305, -335.7573827203992209 ) ) ;
#70678 = CARTESIAN_POINT ( 'NONE',  ( -22.23600029014999180, -296.4619124217902595, -345.0488562389193703 ) ) ;
#70679 = CARTESIAN_POINT ( 'NONE',  ( -110.8334523444457744, -270.7850977723512642, -253.7067142414082355 ) ) ;
#70680 = CARTESIAN_POINT ( 'NONE',  ( -0.04606956585158543394, -293.2141482659956750, -207.4887980860360983 ) ) ;
#70681 = CARTESIAN_POINT ( 'NONE',  ( -85.71451769584137992, -274.2046527044727213, -210.6599509876731133 ) ) ;
#70682 = CARTESIAN_POINT ( 'NONE',  ( -109.8542297915555821, -289.2948059940875396, -257.5283358732006604 ) ) ;
#70683 = CARTESIAN_POINT ( 'NONE',  ( 50.62885399555703003, -301.1535713209074743, -195.3311200258940801 ) ) ;
#70684 = CARTESIAN_POINT ( 'NONE',  ( -58.11103645772325166, -274.2832579749527895, -196.2236088678313308 ) ) ;
#70685 = CARTESIAN_POINT ( 'NONE',  ( -94.47051604516552459, -297.5274950952226050, -224.8816074443593891 ) ) ;
#70686 = CARTESIAN_POINT ( 'NONE',  ( 18.88425334251419940, -282.8367697728737653, -220.1715236988281674 ) ) ;
#70687 = CARTESIAN_POINT ( 'NONE',  ( 36.71023826732177753, -280.4791589901851125, -289.5863278382886392 ) ) ;
#70688 = CARTESIAN_POINT ( 'NONE',  ( -103.5223005592907413, -277.3887585378208200, -309.6247324694608096 ) ) ;
#70689 = CARTESIAN_POINT ( 'NONE',  ( 38.00683522936126479, -279.8041368919586489, -258.6587801150954533 ) ) ;
#70690 = CARTESIAN_POINT ( 'NONE',  ( 23.13230107297217231, -278.9442864628056213, -225.7189450079954440 ) ) ;
#70691 = EDGE_CURVE ( 'NONE', #53738, #53411, #16062, .T. ) ;
#70692 = CARTESIAN_POINT ( 'NONE',  ( -83.54657151150803429, -271.9786011799494645, -213.0856016090108938 ) ) ;
#70693 = CARTESIAN_POINT ( 'NONE',  ( -109.5194072967893817, -280.8166845782808991, -249.7960249768669314 ) ) ;
#70694 = CARTESIAN_POINT ( 'NONE',  ( 161.2244399300530233, 8.542400036368780647, 9.000000000000001776 ) ) ;
#70695 = DIRECTION ( 'NONE',  ( 0.000000000000000000, 0.000000000000000000, 1.000000000000000000 ) ) ;
#70696 = CARTESIAN_POINT ( 'NONE',  ( 52.12392687579448136, -297.3974167468510927, -194.4008023326589125 ) ) ;
#70697 = CARTESIAN_POINT ( 'NONE',  ( 35.12940740477638712, -291.3072444358027155, -249.6659116943681056 ) ) ;
#70698 = CARTESIAN_POINT ( 'NONE',  ( -0.8038585024801646606, -292.5237588303530174, -202.5821674939128343 ) ) ;
#70699 = CARTESIAN_POINT ( 'NONE',  ( 37.10481316069009949, -277.4193302802048606, -259.9810849550235616 ) ) ;
#70700 = CARTESIAN_POINT ( 'NONE',  ( -10.75812699870826528, -272.3985159328415762, -200.1748887448128755 ) ) ;
#70701 = CARTESIAN_POINT ( 'NONE',  ( 133.0872704186301405, -299.5541904835127980, -195.3611179825600175 ) ) ;
#70702 = CARTESIAN_POINT ( 'NONE',  ( 28.51897698165462813, -283.9631852285235709, -307.5040850942365864 ) ) ;
#70703 = CARTESIAN_POINT ( 'NONE',  ( 60.83730532400069535, -250.0090898647485176, -21.50000000000000000 ) ) ;
#70704 = CARTESIAN_POINT ( 'NONE',  ( -10.29800412807189858, -284.4048991122417647, -200.3929035370040594 ) ) ;
#70705 = CARTESIAN_POINT ( 'NONE',  ( 145.2857639756989272, -299.5541904835127980, -197.7582414438974183 ) ) ;
#70706 = CARTESIAN_POINT ( 'NONE',  ( -38.36312993873905697, -293.8601601522237843, -343.7510845122176875 ) ) ;
#70707 = CARTESIAN_POINT ( 'NONE',  ( -7.741012508047727003, -284.5838641656993104, -202.2827456846001724 ) ) ;
#70708 = CARTESIAN_POINT ( 'NONE',  ( 175.2296996224750103, 247.0000000000001137, 8.550761578869359170 ) ) ;
#70709 = CARTESIAN_POINT ( 'NONE',  ( 15.71356215118052013, -292.3014939926353577, -323.4448647308847171 ) ) ;
#70710 = CARTESIAN_POINT ( 'NONE',  ( -87.87699077656239410, -282.2230783892252362, -327.6059123063656102 ) ) ;
#70711 = CARTESIAN_POINT ( 'NONE',  ( -35.66482983202826773, -281.6736341949624602, -196.5676293687050133 ) ) ;
#70712 = CARTESIAN_POINT ( 'NONE',  ( 38.69836476072104858, -288.8791217104626980, -280.0576190536216927 ) ) ;
#70713 = CARTESIAN_POINT ( 'NONE',  ( 15.03858046935243031, -280.5651228866703377, -325.4090990231875935 ) ) ;
#70714 = CARTESIAN_POINT ( 'NONE',  ( 19.51519123708373726, -286.9046031848852181, -224.5560103911538761 ) ) ;
#70715 = CARTESIAN_POINT ( 'NONE',  ( -98.49328912324190810, -280.5425154618237684, -229.3333581189755535 ) ) ;
#70716 = CARTESIAN_POINT ( 'NONE',  ( -93.72395175566229852, -278.6952905057843850, -317.0030921002418154 ) ) ;
#70717 = CARTESIAN_POINT ( 'NONE',  ( -1.768764252945906001, -288.5010164096829612, -203.9309061948313229 ) ) ;
#70718 = ORIENTED_EDGE ( 'NONE', *, *, #14576, .F. ) ;
#70719 = CARTESIAN_POINT ( 'NONE',  ( -34.75730480598763705, -297.9169931902062558, -193.3611886416082939 ) ) ;
#70720 = CARTESIAN_POINT ( 'NONE',  ( -94.71999691202900351, -293.1946494561245800, -222.5962301135205337 ) ) ;
#70721 = FACE_OUTER_BOUND ( 'NONE', #15920, .T. ) ;
#70722 = CARTESIAN_POINT ( 'NONE',  ( -95.99890600148557951, -275.6948066931273615, -223.6242672951989618 ) ) ;
#70723 = EDGE_LOOP ( 'NONE', ( #93661, #16966 ) ) ;
#70724 = CARTESIAN_POINT ( 'NONE',  ( 33.01491732840578663, -273.2091214656009583, -243.9040810211828330 ) ) ;
#70725 = CARTESIAN_POINT ( 'NONE',  ( -65.32883455222767566, -293.8117891581078993, -341.2494538634662717 ) ) ;
#70726 = CARTESIAN_POINT ( 'NONE',  ( -34.47060486770152465, -297.5967001460852543, -197.2998270489071899 ) ) ;
#70727 = CARTESIAN_POINT ( 'NONE',  ( 18.36221253671129361, -289.7540299844526430, -318.6846380148112416 ) ) ;
#70728 = CARTESIAN_POINT ( 'NONE',  ( 11.96443253659156269, -282.5089370640034190, -215.1625736811821241 ) ) ;
#70729 = CARTESIAN_POINT ( 'NONE',  ( -84.78451456822662635, -291.1165543216309288, -330.3267409472321106 ) ) ;
#70730 = CARTESIAN_POINT ( 'NONE',  ( -111.5205782233828273, -292.1037796233807740, -251.5788515009789137 ) ) ;
#70731 = CARTESIAN_POINT ( 'NONE',  ( -24.83265226918851809, -288.2117554175019336, -196.3589449734167829 ) ) ;
#70732 = CARTESIAN_POINT ( 'NONE',  ( 19.15871865419534359, -281.0062233138215788, -218.0476141624534989 ) ) ;
#70733 = CARTESIAN_POINT ( 'NONE',  ( 26.86906999661741580, -292.1639613655659105, -310.2876393133010424 ) ) ;
#70734 = CARTESIAN_POINT ( 'NONE',  ( 8.548240937587799237, -280.4943831958558462, -208.4635080494362853 ) ) ;
#70735 = CARTESIAN_POINT ( 'NONE',  ( -11.07496819274521904, -276.2584696785129950, -200.8732889035858022 ) ) ;
#70736 = CARTESIAN_POINT ( 'NONE',  ( -92.08974858914540107, -275.6948066931273047, -226.7417163044926838 ) ) ;
#70737 = CARTESIAN_POINT ( 'NONE',  ( 27.64765862432134469, -273.2700632916935319, -230.8859052190877605 ) ) ;
#70738 = CARTESIAN_POINT ( 'NONE',  ( 11.63197158325052172, -282.8906705383787994, 52.50000000000000711 ) ) ;
#70739 = CARTESIAN_POINT ( 'NONE',  ( 31.41037744323099545, -281.3905397257452137, -295.2319184282449669 ) ) ;
#70740 = CARTESIAN_POINT ( 'NONE',  ( -70.11712441390601214, -278.6794192926264486, -339.6126107171586455 ) ) ;
#70741 = CARTESIAN_POINT ( 'NONE',  ( -90.56522099978477058, -274.5934213320003892, -219.6623275673659634 ) ) ;
#70742 = CARTESIAN_POINT ( 'NONE',  ( -23.81554843122183840, -285.2795309959327597, -194.7434271090556024 ) ) ;
#70743 = CARTESIAN_POINT ( 'NONE',  ( -108.3740525596705595, -292.5841545060434328, -249.5223453703365237 ) ) ;
#70744 = CARTESIAN_POINT ( 'NONE',  ( -18.76493754809575165, -275.8874733854373176, -196.4057545819365771 ) ) ;
#70745 = CARTESIAN_POINT ( 'NONE',  ( -91.82967052955407894, -274.6097341848593487, -216.6548859997681404 ) ) ;
#70746 = CARTESIAN_POINT ( 'NONE',  ( 199.1087447750284980, 64.61450673763175701, 10.46317447812566570 ) ) ;
#70747 = CARTESIAN_POINT ( 'NONE',  ( 11.74613352572937686, -276.1813034930604545, -324.4610386118191059 ) ) ;
#70748 = CARTESIAN_POINT ( 'NONE',  ( -107.7024545047438124, -298.2193793716484720, -295.9965257390982174 ) ) ;
#70749 = CARTESIAN_POINT ( 'NONE',  ( -97.21790990838889002, -283.1666775140588470, -225.4738376924498766 ) ) ;
#70750 = CARTESIAN_POINT ( 'NONE',  ( -11.15645225876424185, -292.0508542489702677, -197.9167176020374086 ) ) ;
#70751 = CARTESIAN_POINT ( 'NONE',  ( 21.15997851667113139, -272.9321101434353523, -223.9790298987078643 ) ) ;
#70752 = CARTESIAN_POINT ( 'NONE',  ( 7.480570308289862247, -290.0526243487146871, -332.0492819720870443 ) ) ;
#70753 = EDGE_CURVE ( 'NONE', #2466, #20445, #33780, .T. ) ;
#70754 = CARTESIAN_POINT ( 'NONE',  ( -110.2790591626303609, -289.5693331432657374, -262.9876703303661429 ) ) ;
#70755 = EDGE_LOOP ( 'NONE', ( #33257, #42629, #90182, #30570 ) ) ;
#70756 = CARTESIAN_POINT ( 'NONE',  ( -111.0595049218839279, -289.3812287864160453, -250.2045108625517855 ) ) ;
#70757 = CARTESIAN_POINT ( 'NONE',  ( -100.3243372570148324, -289.7104707549527234, -307.4103441977669036 ) ) ;
#70758 = VERTEX_POINT ( 'NONE', #75217 ) ;
#70759 = CARTESIAN_POINT ( 'NONE',  ( 11.86865752226332660, -287.7967430556263935, -211.4714849669444163 ) ) ;
#70760 = CARTESIAN_POINT ( 'NONE',  ( -107.1355745642640898, -278.5991251391711785, -291.9990437630934252 ) ) ;
#70761 = EDGE_CURVE ( 'NONE', #15223, #90518, #65507, .T. ) ;
#70762 = CARTESIAN_POINT ( 'NONE',  ( -50.42835683319628970, -294.1356815582636841, -345.9809241825311688 ) ) ;
#70763 = CARTESIAN_POINT ( 'NONE',  ( -74.21979752927676088, -284.1801574528889773, -337.8988115726390902 ) ) ;
#70764 = CARTESIAN_POINT ( 'NONE',  ( -106.6619132904246214, -285.3150219072456366, -236.8879595035300554 ) ) ;
#70765 = CARTESIAN_POINT ( 'NONE',  ( -6.020023963921404153, -282.9621175227376284, -336.3372867996187097 ) ) ;
#70766 = CARTESIAN_POINT ( 'NONE',  ( 121.7669983244749403, 149.6016541078746798, -263.6324895168810372 ) ) ;
#70767 = CARTESIAN_POINT ( 'NONE',  ( -110.7434605763195350, -265.2408335553506049, -306.4457901866108500 ) ) ;
#70768 = CARTESIAN_POINT ( 'NONE',  ( -13.40524764562645998, -91.92062792358137813, -356.3535239457285684 ) ) ;
#70769 = CARTESIAN_POINT ( 'NONE',  ( 21.61736411087281695, -274.1437539661689584, -227.0433332815328527 ) ) ;
#70770 = CARTESIAN_POINT ( 'NONE',  ( -29.94506394337190969, -273.0682956552009273, -197.4261068655856093 ) ) ;
#70771 = CARTESIAN_POINT ( 'NONE',  ( -97.36337231765800482, -295.4141523037879438, -318.5164254622376916 ) ) ;
#70772 = CARTESIAN_POINT ( 'NONE',  ( -81.75305709561430945, -219.5167969555488696, -349.4486404927797594 ) ) ;
#70773 = CARTESIAN_POINT ( 'NONE',  ( 28.66199125000223802, -274.7438343475895408, -309.0497596781670495 ) ) ;
#70774 = CARTESIAN_POINT ( 'NONE',  ( -84.88375982183343638, -299.2492189638595619, -213.2797923915757963 ) ) ;
#70775 = CARTESIAN_POINT ( 'NONE',  ( -103.8424724307707834, -292.0465230206620504, -239.5086730910153960 ) ) ;
#70776 = VERTEX_POINT ( 'NONE', #66716 ) ;
#70777 = CARTESIAN_POINT ( 'NONE',  ( -107.5626621740012610, -297.8917778681564528, -239.2161547970895015 ) ) ;
#70778 = CARTESIAN_POINT ( 'NONE',  ( 30.54468721774808770, -288.4071901495208863, -297.5055009630654013 ) ) ;
#70779 = CARTESIAN_POINT ( 'NONE',  ( -114.1765953379295553, -297.3643426482988161, -269.6143261189695863 ) ) ;
#70780 = CARTESIAN_POINT ( 'NONE',  ( -61.56623761386740057, -295.8508433272298248, -343.4421396056974913 ) ) ;
#70781 = CARTESIAN_POINT ( 'NONE',  ( 34.48279183177873364, -293.5457952988538750, -257.2439245673625692 ) ) ;
#70782 = ORIENTED_EDGE ( 'NONE', *, *, #57774, .F. ) ;
#70783 = CARTESIAN_POINT ( 'NONE',  ( 36.50367686172460679, -277.6770576018200813, -286.4271100973249418 ) ) ;
#70784 = CARTESIAN_POINT ( 'NONE',  ( 37.92577506058935199, -280.8594089999433550, -254.3502113396222626 ) ) ;
#70785 = CARTESIAN_POINT ( 'NONE',  ( 22.46608172164806660, -275.9050657113726288, -228.0731430680824872 ) ) ;
#70786 = CARTESIAN_POINT ( 'NONE',  ( -18.81897362504284743, -276.0474604769079860, -196.6122938103376896 ) ) ;
#70787 = CARTESIAN_POINT ( 'NONE',  ( -96.65031552451543462, -275.9373209348626688, -316.8465452376109397 ) ) ;
#70788 = CARTESIAN_POINT ( 'NONE',  ( -35.15223256983011879, -298.7316880494328188, -197.2589340308238377 ) ) ;
#70789 = CARTESIAN_POINT ( 'NONE',  ( -108.0202760814093637, -295.3957475003086302, -249.8693191578521464 ) ) ;
#70790 = DIRECTION ( 'NONE',  ( 0.000000000000000000, 0.000000000000000000, 1.000000000000000000 ) ) ;
#70791 = CARTESIAN_POINT ( 'NONE',  ( -97.65256745355323176, -279.6842546397919023, -222.5895135921271617 ) ) ;
#70792 = CARTESIAN_POINT ( 'NONE',  ( -64.33116664940294527, -277.5809682468732262, -338.2422917424806883 ) ) ;
#70793 = CARTESIAN_POINT ( 'NONE',  ( 9.521973557649090480, -285.3664268247834457, -209.8872032745990737 ) ) ;
#70794 = CARTESIAN_POINT ( 'NONE',  ( -72.44761772685525614, -299.5891825052127615, -203.8386099904832065 ) ) ;
#70795 = LINE ( 'NONE', #63715, #85282 ) ;
#70796 = CARTESIAN_POINT ( 'NONE',  ( 32.46461100160329494, -287.0409532486501121, -292.4312667663220395 ) ) ;
#70797 = CARTESIAN_POINT ( 'NONE',  ( -92.95524589532598725, -277.4797638914051845, -221.5042826305259496 ) ) ;
#70799 = CARTESIAN_POINT ( 'NONE',  ( -36.19540709172365922, -281.1175158213353598, -344.7922956809714492 ) ) ;
#70798 = CARTESIAN_POINT ( 'NONE',  ( -108.8580466930563233, -277.3538706080149154, -253.0179033753887552 ) ) ;
#70800 = CARTESIAN_POINT ( 'NONE',  ( -9.061834272863206863, -288.4220971198014922, -200.8834562642012145 ) ) ;
#70801 = CARTESIAN_POINT ( 'NONE',  ( 12.02606585383540150, -277.5528384434420559, -324.7435777997233117 ) ) ;
#70802 = DIRECTION ( 'NONE',  ( 0.000000000000000000, 1.000000000000000000, 0.000000000000000000 ) ) ;
#70803 = CARTESIAN_POINT ( 'NONE',  ( -96.77930032168920604, -293.1791205013205399, -224.6000568379405706 ) ) ;
#70804 = CARTESIAN_POINT ( 'NONE',  ( -48.36937523186626464, -275.4303816882110141, -345.5965130343774376 ) ) ;
#70805 = VECTOR ( 'NONE', #60610, 1000.000000000000114 ) ;
#70806 = CARTESIAN_POINT ( 'NONE',  ( 35.20830795973833460, -276.3270031044157236, -279.7311829732614115 ) ) ;
#70807 = CARTESIAN_POINT ( 'NONE',  ( 33.58899650509938084, -283.2290831287344872, -245.3288222576561850 ) ) ;
#70808 = EDGE_CURVE ( 'NONE', #1443, #33827, #13171, .T. ) ;
#70809 = EDGE_CURVE ( 'NONE', #90307, #49439, #9395, .T. ) ;
#70810 = DIRECTION ( 'NONE',  ( 0.000000000000000000, -0.000000000000000000, 1.000000000000000000 ) ) ;
#70811 = CARTESIAN_POINT ( 'NONE',  ( 36.70217038495741946, -289.6642440373236695, -285.4216438930553181 ) ) ;
#70812 = CARTESIAN_POINT ( 'NONE',  ( -15.02810889987506648, -292.7631167202657707, -342.0183686775097840 ) ) ;
#70813 = CARTESIAN_POINT ( 'NONE',  ( 165.2494399300530290, 8.542400036368780647, 10.00000000000000000 ) ) ;
#70814 = CARTESIAN_POINT ( 'NONE',  ( -13.89234434362371395, -273.0477289436876731, -200.7093327168589951 ) ) ;
#70815 = CARTESIAN_POINT ( 'NONE',  ( 34.50961580373898840, -291.4494648481593231, -251.6995563758633807 ) ) ;
#70816 = CARTESIAN_POINT ( 'NONE',  ( 201.7194887906492795, 294.2213704821156739, -83.28174295417332473 ) ) ;
#70817 = CARTESIAN_POINT ( 'NONE',  ( -16.79453476385504018, -290.7927503646538980, -196.8728757492164902 ) ) ;
#70818 = CARTESIAN_POINT ( 'NONE',  ( -81.08410058457873504, -285.2573002304844181, -329.8640910098963559 ) ) ;
#70819 = CARTESIAN_POINT ( 'NONE',  ( 4.638762607568192031, -284.8498623947787110, -206.9611264115397091 ) ) ;
#70820 = CARTESIAN_POINT ( 'NONE',  ( -81.84925480297376055, -286.8573669588631105, -211.7569159802048375 ) ) ;
#70821 = CARTESIAN_POINT ( 'NONE',  ( -97.49451986551379434, -285.9341491107848583, -228.6947617901457761 ) ) ;
#70822 = CARTESIAN_POINT ( 'NONE',  ( -100.3234184067648300, -293.0888348299243376, -228.8946195672068598 ) ) ;
#70823 = CARTESIAN_POINT ( 'NONE',  ( 35.89564589079301982, -273.3949467998783120, -251.7706540483175672 ) ) ;
#70824 = CARTESIAN_POINT ( 'NONE',  ( 26.91057509555442451, -275.3277704181090257, -227.9654882538820857 ) ) ;
#70825 = CARTESIAN_POINT ( 'NONE',  ( -99.50999185160974037, -288.0540628125497165, -313.3078024046383803 ) ) ;
#70826 = CARTESIAN_POINT ( 'NONE',  ( 12.70461835195821187, -276.3762486724124869, -328.8792007142631064 ) ) ;
#70827 = CARTESIAN_POINT ( 'NONE',  ( -81.09904172917407550, -297.6298277862287023, -330.8354253859787377 ) ) ;
#70828 = CARTESIAN_POINT ( 'NONE',  ( -48.18343439339133027, -254.0547856900534214, -480.4587914081801614 ) ) ;
#70829 = DIRECTION ( 'NONE',  ( 1.000000000000000000, 0.000000000000000000, 0.000000000000000000 ) ) ;
#70830 = CARTESIAN_POINT ( 'NONE',  ( -109.9884243026998689, -283.0869569537228472, -281.8100087106455476 ) ) ;
#70831 = CARTESIAN_POINT ( 'NONE',  ( -69.09190519811453157, -277.6344828303724626, -202.3991451189241957 ) ) ;
#70832 = CARTESIAN_POINT ( 'NONE',  ( 133.0872704186301405, -299.5541904835127980, -195.3611179825600175 ) ) ;
#70833 = CARTESIAN_POINT ( 'NONE',  ( 37.54211186496195296, -273.8469372919240072, -255.6940645699230572 ) ) ;
#70834 = CARTESIAN_POINT ( 'NONE',  ( -18.99936815586674754, -276.1583093663208501, -341.1244667279741520 ) ) ;
#70835 = CARTESIAN_POINT ( 'NONE',  ( -34.25294064596364763, -296.5327388078561626, -343.9896947619949401 ) ) ;
#70836 = CARTESIAN_POINT ( 'NONE',  ( 24.35129957681044033, -279.8646267406712127, -224.8038320897036613 ) ) ;
#70837 = CARTESIAN_POINT ( 'NONE',  ( 12.52383084865697604, -295.2782116472359917, -324.0667909051300057 ) ) ;
#70838 = CARTESIAN_POINT ( 'NONE',  ( 3.975161723384856849, -295.8236933992315016, -334.8146109976244134 ) ) ;
#70839 = CARTESIAN_POINT ( 'NONE',  ( -110.3626861462309137, -272.2548568503066235, -267.6322362053812185 ) ) ;
#70840 = CARTESIAN_POINT ( 'NONE',  ( -108.4760689522130832, -292.8595474916429566, -246.5934462369953337 ) ) ;
#70841 = CARTESIAN_POINT ( 'NONE',  ( -7.345088173612762894, -286.6013459820299545, -199.3875874785503015 ) ) ;
#70842 = CARTESIAN_POINT ( 'NONE',  ( -1.858659863862177630, -272.6567042821487235, -203.4189090541416931 ) ) ;
#70843 = CARTESIAN_POINT ( 'NONE',  ( 9.812428825423710421, -286.5147359564604699, -209.4883972685940705 ) ) ;
#70844 = CARTESIAN_POINT ( 'NONE',  ( -95.23176189144186310, -281.1843245766279438, -223.2380073489340191 ) ) ;
#70845 = CARTESIAN_POINT ( 'NONE',  ( -37.26864129253610258, -285.1117984819755975, -197.1133809304161559 ) ) ;
#70846 = AXIS2_PLACEMENT_3D ( 'NONE', #18745, #84987, #49025 ) ;
#70847 = CARTESIAN_POINT ( 'NONE',  ( -102.0851540078492832, -288.0449517654854503, -308.3226612088314482 ) ) ;
#70848 = CARTESIAN_POINT ( 'NONE',  ( -109.0101294763935016, -268.7602059993127455, -295.2240039188629339 ) ) ;
#70849 = CARTESIAN_POINT ( 'NONE',  ( -33.22892778159213378, -285.6128458873258751, -197.3655671618930967 ) ) ;
#70850 = CARTESIAN_POINT ( 'NONE',  ( 154.9065949031809453, 18.65395765032405961, 9.525636664968139655 ) ) ;
#70851 = CARTESIAN_POINT ( 'NONE',  ( 4.427753012850422110, -283.4451193332757271, -334.8299503909703390 ) ) ;
#70852 = CARTESIAN_POINT ( 'NONE',  ( -47.69974089432111697, -290.9824113499088867, -194.2448091947306921 ) ) ;
#70853 = CARTESIAN_POINT ( 'NONE',  ( -111.9386192217766620, -280.3495570346349268, -254.7501178991218183 ) ) ;
#70854 = CARTESIAN_POINT ( 'NONE',  ( -113.5861292134884764, -279.7799453703643735, -277.3031037038877571 ) ) ;
#70855 = CARTESIAN_POINT ( 'NONE',  ( 33.64965152270030302, -281.6105199244289565, -287.4209966694936611 ) ) ;
#70856 = CARTESIAN_POINT ( 'NONE',  ( -3.216824501555996640, -276.5029539138312202, -203.5597764831137795 ) ) ;
#70857 = CARTESIAN_POINT ( 'NONE',  ( -92.69700478724686832, -295.8189102268943316, -323.8848533351208516 ) ) ;
#70858 = CARTESIAN_POINT ( 'NONE',  ( -111.3270007188919664, -288.7049181055403437, -260.0780928245881682 ) ) ;
#70859 = CARTESIAN_POINT ( 'NONE',  ( -90.64139173792274562, -294.7498978232420654, -320.7668231668674821 ) ) ;
#70860 = EDGE_LOOP ( 'NONE', ( #15337, #16349, #16385, #54498 ) ) ;
#70861 = ORIENTED_EDGE ( 'NONE', *, *, #82755, .F. ) ;
#70862 = CARTESIAN_POINT ( 'NONE',  ( 20.48585876962583185, -284.1228759773125034, -317.2564523177530305 ) ) ;
#70863 = CARTESIAN_POINT ( 'NONE',  ( -69.73726499790593891, -295.1576538710190789, -335.8028085447425042 ) ) ;
#70864 = CARTESIAN_POINT ( 'NONE',  ( 39.19467391036910442, -294.7026612976429192, -276.0026567837508651 ) ) ;
#70865 = CARTESIAN_POINT ( 'NONE',  ( -16.09496319479997339, -283.4214472279232950, -340.3073032797045130 ) ) ;
#70866 = CARTESIAN_POINT ( 'NONE',  ( -10.41887150142800245, -273.4536276322706954, -198.4158897540949340 ) ) ;
#70867 = CARTESIAN_POINT ( 'NONE',  ( -112.7663882200000387, -291.0151208418662350, -285.4087876665742556 ) ) ;
#70868 = CARTESIAN_POINT ( 'NONE',  ( -43.54118546448030003, -284.1143461959666752, -194.7979735607809175 ) ) ;
#70869 = CARTESIAN_POINT ( 'NONE',  ( -110.4121741973763733, -291.1922175175238294, -245.9775461755935453 ) ) ;
#70870 = CARTESIAN_POINT ( 'NONE',  ( 30.99288311759143966, -287.5403570270709679, -244.4798690943914607 ) ) ;
#70871 = CARTESIAN_POINT ( 'NONE',  ( 153.6987871352711181, 19.48326534539917887, -11.45812909362560639 ) ) ;
#70872 = CARTESIAN_POINT ( 'NONE',  ( 153.4133700136260927, 129.9709486557056834, -11.65454253063697898 ) ) ;
#70873 = CARTESIAN_POINT ( 'NONE',  ( -111.0016612856833831, -271.0675853585269692, -270.3422158909584709 ) ) ;
#70874 = CARTESIAN_POINT ( 'NONE',  ( 22.86789198823231928, -283.7044044627420476, -317.2598756660011077 ) ) ;
#70875 = CARTESIAN_POINT ( 'NONE',  ( 21.31550574532286291, -284.4094976428775681, -223.6242672951989618 ) ) ;
#70876 = VERTEX_POINT ( 'NONE', #31207 ) ;
#70877 = CARTESIAN_POINT ( 'NONE',  ( 0.5715380142630172022, -279.4903416938436180, -207.5583266017104904 ) ) ;
#70878 = CARTESIAN_POINT ( 'NONE',  ( -9.223495967937791917, -276.3611309706924999, -342.0208059970449881 ) ) ;
#70879 = CARTESIAN_POINT ( 'NONE',  ( -57.05930384398344302, -279.3071096992368325, -342.6038788174282672 ) ) ;
#70880 = CARTESIAN_POINT ( 'NONE',  ( -110.4560292262735146, -273.1165755189331890, -283.8932947766008397 ) ) ;
#70881 = CARTESIAN_POINT ( 'NONE',  ( 39.03029897396627490, -280.1575556320187843, -272.7950539921042719 ) ) ;
#70882 = CARTESIAN_POINT ( 'NONE',  ( -70.69524898940100854, -283.6302444693379812, -203.5682154360150946 ) ) ;
#70883 = CARTESIAN_POINT ( 'NONE',  ( -110.9809931515036681, -298.0740481028470867, -289.1546767135573646 ) ) ;
#70884 = CARTESIAN_POINT ( 'NONE',  ( 28.45269661009361073, -294.4754240874830771, -302.2439228450415385 ) ) ;
#70886 = ORIENTED_EDGE ( 'NONE', *, *, #791, .T. ) ;
#70885 = ADVANCED_FACE ( 'NONE', ( #10331 ), #65730, .T. ) ;
#70887 = CARTESIAN_POINT ( 'NONE',  ( -108.2057804588883840, -288.9790778856013276, -290.0302338702121574 ) ) ;
#70888 = CARTESIAN_POINT ( 'NONE',  ( -10.39112158241530715, -275.0460359887375148, -198.2837869965204618 ) ) ;
#70889 = CARTESIAN_POINT ( 'NONE',  ( -108.5348967160139750, -272.7650774939410780, -254.2202146747527536 ) ) ;
#70890 = ORIENTED_EDGE ( 'NONE', *, *, #83847, .F. ) ;
#70891 = DIRECTION ( 'NONE',  ( -0.000000000000000000, 0.000000000000000000, -1.000000000000000000 ) ) ;
#70892 = CARTESIAN_POINT ( 'NONE',  ( 180.5131398354828320, 250.5000000000000568, -23.92352941176473635 ) ) ;
#70893 = CARTESIAN_POINT ( 'NONE',  ( 34.86921037486619213, -282.4657665448449961, -257.7195010579127938 ) ) ;
#70894 = CARTESIAN_POINT ( 'NONE',  ( -86.17093577143498351, -281.1462028920039984, -212.0715622585161952 ) ) ;
#70895 = CARTESIAN_POINT ( 'NONE',  ( -42.96289909478856117, -282.1834426611433742, -343.4306137799651424 ) ) ;
#70896 = CARTESIAN_POINT ( 'NONE',  ( 28.87259822389665587, -282.9630759024261124, -236.6833557885064465 ) ) ;
#70897 = CARTESIAN_POINT ( 'NONE',  ( 22.05135022558042834, -273.4265805182347435, -226.7357432167933950 ) ) ;
#70898 = CARTESIAN_POINT ( 'NONE',  ( 154.3452702497934013, 20.31595811206259938, 11.82731014213360510 ) ) ;
#70899 = CARTESIAN_POINT ( 'NONE',  ( 197.2116943569230045, 250.0000000000000568, -12.92446933126075592 ) ) ;
#70900 = CARTESIAN_POINT ( 'NONE',  ( -112.0158217758180541, -279.1273359679276496, -288.5251568024719404 ) ) ;
#70901 = ORIENTED_EDGE ( 'NONE', *, *, #59380, .F. ) ;
#70902 = EDGE_LOOP ( 'NONE', ( #28449, #26601, #24127, #33730 ) ) ;
#70903 = CARTESIAN_POINT ( 'NONE',  ( 140.6539576904058606, 249.5000000000000568, -12.50000000000000000 ) ) ;
#70904 = CARTESIAN_POINT ( 'NONE',  ( -64.63248303161870467, -285.3865656027595605, -340.6147484032086368 ) ) ;
#70905 = CARTESIAN_POINT ( 'NONE',  ( 19.81351785695841627, -293.3932589804636564, -316.0525511050038858 ) ) ;
#70906 = CARTESIAN_POINT ( 'NONE',  ( 12.34364164194936997, -287.7296803646689227, -329.0525108734586297 ) ) ;
#70907 = CARTESIAN_POINT ( 'NONE',  ( -98.17623918014778894, -283.3715890535725066, -228.1826710478582925 ) ) ;
#70909 = CARTESIAN_POINT ( 'NONE',  ( -76.42256932269475556, -287.8225205175797328, -333.2153913122146491 ) ) ;
#70908 = CARTESIAN_POINT ( 'NONE',  ( -77.35434431741335004, -284.0790417985784870, -208.5401351762213267 ) ) ;
#70910 = AXIS2_PLACEMENT_3D ( 'NONE', #42258, #35169, #85816 ) ;
#70911 = CARTESIAN_POINT ( 'NONE',  ( 34.87890127943792606, -282.9298848429468762, -283.5203675050298102 ) ) ;
#70912 = CARTESIAN_POINT ( 'NONE',  ( -0.9918670210656873598, -272.5344510748199127, -204.7439945824827134 ) ) ;
#70913 = CARTESIAN_POINT ( 'NONE',  ( -36.55302976323596909, -284.4617733364769947, -194.1522928282763871 ) ) ;
#70914 = CARTESIAN_POINT ( 'NONE',  ( -43.16067667201198788, -299.9789741420964901, -195.5353624317758374 ) ) ;
#70915 = CARTESIAN_POINT ( 'NONE',  ( -26.85116024546423574, -284.1849662824337202, -195.8778696644413628 ) ) ;
#70916 = CARTESIAN_POINT ( 'NONE',  ( 34.29284375403562279, -282.2924094522277301, -255.0731314231204294 ) ) ;
#70917 = CARTESIAN_POINT ( 'NONE',  ( 36.31695888212765766, -289.7442375099765286, -285.3421187120097215 ) ) ;
#70918 = DIRECTION ( 'NONE',  ( -0.000000000000000000, -1.000000000000000000, -0.000000000000000000 ) ) ;
#70919 = EDGE_CURVE ( 'NONE', #4814, #93104, #39756, .T. ) ;
#70920 = ADVANCED_FACE ( 'NONE', ( #77078 ), #61942, .F. ) ;
#70921 = DIRECTION ( 'NONE',  ( 0.000000000000000000, 0.000000000000000000, 1.000000000000000000 ) ) ;
#70922 = CARTESIAN_POINT ( 'NONE',  ( 20.28556648569308507, -296.1435760537691522, -319.2325037150431513 ) ) ;
#70923 = CARTESIAN_POINT ( 'NONE',  ( -65.09632711984581022, -275.4144774322957119, -340.0918235675195547 ) ) ;
#70924 = CARTESIAN_POINT ( 'NONE',  ( -94.58416970613943420, -290.4461144431871844, -219.1023772910478158 ) ) ;
#70925 = CARTESIAN_POINT ( 'NONE',  ( -8.941649358748334109, -293.0742662204073099, -338.4915175732525654 ) ) ;
#70926 = CARTESIAN_POINT ( 'NONE',  ( -79.32294263654321753, -278.1568557582464791, -210.0384957387145164 ) ) ;
#70927 = CARTESIAN_POINT ( 'NONE',  ( -67.29639256208635345, -295.7947203239685905, -202.4238560137765148 ) ) ;
#70928 = CARTESIAN_POINT ( 'NONE',  ( 21.73278676675897714, -295.4761871959046289, -314.0812332294733551 ) ) ;
#70929 = CARTESIAN_POINT ( 'NONE',  ( -95.99890600148557951, -299.6948066931273615, -223.6242672951989618 ) ) ;
#70930 = CARTESIAN_POINT ( 'NONE',  ( -84.77021355066884212, -295.8915592484684112, -210.5845016062207264 ) ) ;
#70931 = CARTESIAN_POINT ( 'NONE',  ( 6.334305210621300475, -290.0483517657721109, -329.9130267857101444 ) ) ;
#70932 = CARTESIAN_POINT ( 'NONE',  ( 30.01125611929756332, -291.3308207911303498, -235.0689059052033656 ) ) ;
#70933 = CARTESIAN_POINT ( 'NONE',  ( -110.9577112757685597, -292.0022508219814767, -268.4645381554518053 ) ) ;
#70934 = DIRECTION ( 'NONE',  ( 0.000000000000000000, 0.000000000000000000, 1.000000000000000000 ) ) ;
#70935 = CARTESIAN_POINT ( 'NONE',  ( -107.1587676930076185, -291.6446595430831508, -248.4515961203839538 ) ) ;
#70936 = DIRECTION ( 'NONE',  ( 1.000000000000000000, 0.000000000000000000, 0.000000000000000000 ) ) ;
#70937 = CARTESIAN_POINT ( 'NONE',  ( -113.8539525038285518, -291.7103843890140524, -274.0872357949349407 ) ) ;
#70939 = CARTESIAN_POINT ( 'NONE',  ( -22.74062800065226497, -292.2442654610633213, -198.8362363487564437 ) ) ;
#70938 = CARTESIAN_POINT ( 'NONE',  ( 14.60113001986866088, -280.3454073179602801, -324.9536925428371319 ) ) ;
#70940 = CARTESIAN_POINT ( 'NONE',  ( 3.821971522519374442, -280.5895950612058414, -205.2247000109324802 ) ) ;
#70941 = CARTESIAN_POINT ( 'NONE',  ( -13.43253302121093462, -282.4166736702749176, -343.5328066313844602 ) ) ;
#70942 = CARTESIAN_POINT ( 'NONE',  ( -20.74695442014492031, -286.8384563326493435, -343.3312683061507187 ) ) ;
#70943 = CARTESIAN_POINT ( 'NONE',  ( 20.65563762792238833, -279.0480263361336597, -224.0235058588398260 ) ) ;
#70944 = CARTESIAN_POINT ( 'NONE',  ( -43.47659215277207068, -283.9746241947050294, -195.5605720765545925 ) ) ;
#70945 = CARTESIAN_POINT ( 'NONE',  ( -28.28788035157748126, -278.6447914057597472, -194.5403293769619779 ) ) ;
#70946 = CARTESIAN_POINT ( 'NONE',  ( -69.65003909050393816, -284.5570965961844649, -200.7934953595722334 ) ) ;
#70947 = CARTESIAN_POINT ( 'NONE',  ( 15.55648881015009444, -275.6268389283337683, -219.7468865658700281 ) ) ;
#70948 = CARTESIAN_POINT ( 'NONE',  ( 195.3159225978357085, 40.29405723410430795, 14.88612872638837636 ) ) ;
#70949 = CARTESIAN_POINT ( 'NONE',  ( -22.60053319631199997, -293.8441363279615075, -198.0483361901948456 ) ) ;
#70950 = CARTESIAN_POINT ( 'NONE',  ( -32.73639169844857122, -275.5343578870714509, -194.0762026658211425 ) ) ;
#70951 = CARTESIAN_POINT ( 'NONE',  ( -69.26449129827435058, -277.1507585818379198, -336.0485681243608838 ) ) ;
#70952 = CARTESIAN_POINT ( 'NONE',  ( -56.19084167351235237, -291.9826410033352886, -195.6488867628638957 ) ) ;
#70953 = CARTESIAN_POINT ( 'NONE',  ( -91.42051961426787443, -281.8943788855058301, -323.1322794279773234 ) ) ;
#70954 = EDGE_CURVE ( 'NONE', #3752, #50728, #52957, .T. ) ;
#70955 = CARTESIAN_POINT ( 'NONE',  ( -33.48409333257379217, -291.1606104851200598, -197.2149591771018038 ) ) ;
#70956 = CARTESIAN_POINT ( 'NONE',  ( 14.08822429628926542, -292.3298601329112216, -324.9501601104191764 ) ) ;
#70957 = EDGE_LOOP ( 'NONE', ( #50571, #85894 ) ) ;
#70958 = CARTESIAN_POINT ( 'NONE',  ( 152.0139507567534736, 20.82771571514191677, 9.304222368691537071 ) ) ;
#70959 = CARTESIAN_POINT ( 'NONE',  ( -57.66605211493640581, -291.2903292289551018, -200.1305009064132889 ) ) ;
#70960 = CARTESIAN_POINT ( 'NONE',  ( 196.3496553477289979, 276.0000000000000568, -12.41762739670150850 ) ) ;
#70961 = CARTESIAN_POINT ( 'NONE',  ( -92.08974858914540107, -299.6948066931273047, -226.7417163044926838 ) ) ;
#70962 = CARTESIAN_POINT ( 'NONE',  ( -98.04052598606990898, -296.2404562455266159, -223.3455175950362275 ) ) ;
#70963 = CARTESIAN_POINT ( 'NONE',  ( 34.43121265529653385, -280.0042729836175113, -294.7923907890756254 ) ) ;
#70964 = CARTESIAN_POINT ( 'NONE',  ( -87.43974517206224562, -286.6857938340589840, -212.4681002627114594 ) ) ;
#70965 = CARTESIAN_POINT ( 'NONE',  ( 35.27461090180653258, -287.2868672477175664, -262.8864021414252079 ) ) ;
#70966 = CARTESIAN_POINT ( 'NONE',  ( 36.04621583837688092, -277.1598641289244256, -277.0634714136897401 ) ) ;
#70967 = CARTESIAN_POINT ( 'NONE',  ( -101.2932450241813314, -295.0914935827347563, -231.7632958673291910 ) ) ;
#70968 = CARTESIAN_POINT ( 'NONE',  ( -111.0617634904087794, -298.4051622642763846, -263.2239262074630233 ) ) ;
#70969 = CARTESIAN_POINT ( 'NONE',  ( 9.908016002244695031, -275.1789883518918600, -326.5268978601913545 ) ) ;
#70970 = VERTEX_POINT ( 'NONE', #11280 ) ;
#70971 = CARTESIAN_POINT ( 'NONE',  ( 208.4306832106271088, 42.44233620800392970, 0.000000000000000000 ) ) ;
#70972 = CARTESIAN_POINT ( 'NONE',  ( -113.7532781696036182, -296.3355659216187519, -261.0329331272471904 ) ) ;
#70973 = CARTESIAN_POINT ( 'NONE',  ( 8.893081617182170717, -290.3323940235146665, -328.7020054615854860 ) ) ;
#70974 = CARTESIAN_POINT ( 'NONE',  ( -43.95506239605219179, -295.9685147819440090, -195.6024511661221084 ) ) ;
#70975 = CARTESIAN_POINT ( 'NONE',  ( -39.95334237696749113, -289.7371159817230932, -343.4660310767235956 ) ) ;
#70976 = ORIENTED_EDGE ( 'NONE', *, *, #31797, .T. ) ;
#70977 = CARTESIAN_POINT ( 'NONE',  ( -79.77071900964088513, -278.5527743114512305, -206.3239389937831163 ) ) ;
#70978 = CARTESIAN_POINT ( 'NONE',  ( -105.1676193242628727, -297.6737069820127317, -234.0133818564297314 ) ) ;
#70979 = CARTESIAN_POINT ( 'NONE',  ( -69.08370068343513992, -289.7787504853539531, -201.5520164022698566 ) ) ;
#70980 = AXIS2_PLACEMENT_3D ( 'NONE', #38869, #59282, #1975 ) ;
#70981 = CARTESIAN_POINT ( 'NONE',  ( -84.16897645924262861, -296.0092153158394126, -331.5261984271884899 ) ) ;
#70982 = CARTESIAN_POINT ( 'NONE',  ( 32.64812548547408255, -293.6078836452310838, -249.3659678097900496 ) ) ;
#70983 = CARTESIAN_POINT ( 'NONE',  ( 198.6884013828325521, 64.61450673763175701, -9.555809373750793867 ) ) ;
#70984 = FACE_OUTER_BOUND ( 'NONE', #61295, .T. ) ;
#70985 = DIRECTION ( 'NONE',  ( -0.000000000000000000, -0.000000000000000000, -1.000000000000000000 ) ) ;
#70986 = CARTESIAN_POINT ( 'NONE',  ( -15.13535091360628293, -290.2899352147778700, -343.4203839086674179 ) ) ;
#70987 = CARTESIAN_POINT ( 'NONE',  ( 13.84574458161073096, -284.9090924074130839, -334.4957818155094174 ) ) ;
#70988 = VERTEX_POINT ( 'NONE', #18377 ) ;
#70989 = CARTESIAN_POINT ( 'NONE',  ( 36.37857623291522202, -281.1776607550194171, -292.4219308133722279 ) ) ;
#70990 = CARTESIAN_POINT ( 'NONE',  ( 11.11474070345475340, -284.3800312527851588, -327.4556088445825139 ) ) ;
#70991 = CARTESIAN_POINT ( 'NONE',  ( 38.20576885447741233, -285.9814356807377749, -258.8202113663200521 ) ) ;
#70992 = CARTESIAN_POINT ( 'NONE',  ( -89.69076770301721524, -287.8774487862178262, -323.2845468276768202 ) ) ;
#70993 = CARTESIAN_POINT ( 'NONE',  ( -4.508345881559846724, -278.4845773872683026, -338.6562503927178795 ) ) ;
#70994 = ORIENTED_EDGE ( 'NONE', *, *, #88732, .F. ) ;
#70996 = CARTESIAN_POINT ( 'NONE',  ( -38.34693172036762121, -279.3878115182692454, -197.2536785777012653 ) ) ;
#70995 = CARTESIAN_POINT ( 'NONE',  ( -109.9040205576796581, -278.4409636319444985, -278.7898166426994635 ) ) ;
#70997 = CARTESIAN_POINT ( 'NONE',  ( 22.40885946167023590, -277.2789281126348442, -318.4585332682208900 ) ) ;
#70998 = CARTESIAN_POINT ( 'NONE',  ( -61.90569913442672600, -278.5348624283664662, -197.7474876212106096 ) ) ;
#70999 = CARTESIAN_POINT ( 'NONE',  ( 183.1810840045989153, 262.4765370933737927, -151.7797582644170689 ) ) ;
#71000 = CARTESIAN_POINT ( 'NONE',  ( -108.9514565853776418, -273.8464409009349652, -242.5585825294248821 ) ) ;
#71001 = CONTEXT_DEPENDENT_SHAPE_REPRESENTATION ( #91607, #50491 ) ;
#71002 = CARTESIAN_POINT ( 'NONE',  ( -29.15655736420033861, -299.5780001754430373, -193.9484034568351092 ) ) ;
#71003 = CARTESIAN_POINT ( 'NONE',  ( -20.19161114001083490, -291.3376638359845856, -345.3538533559490702 ) ) ;
#71004 = LINE ( 'NONE', #28847, #68061 ) ;
#71005 = CARTESIAN_POINT ( 'NONE',  ( 18.06816511220410604, -289.3136505918149055, -318.4368582874723188 ) ) ;
#71006 = CARTESIAN_POINT ( 'NONE',  ( -108.0932797217043912, -286.6699263575930559, -242.5017078258306071 ) ) ;
#71007 = CARTESIAN_POINT ( 'NONE',  ( 30.57681734277025143, -287.2636138766055183, -297.5340165952620168 ) ) ;
#71008 = CARTESIAN_POINT ( 'NONE',  ( -65.23572785461395540, -282.9147251450477825, -342.0792168366573378 ) ) ;
#71009 = CARTESIAN_POINT ( 'NONE',  ( -6.415782336955198062, -278.8651154760787563, -203.3396500841393504 ) ) ;
#71010 = CARTESIAN_POINT ( 'NONE',  ( -40.04218151361544642, -287.8782752587993059, -196.1750486518603225 ) ) ;
#71011 = CARTESIAN_POINT ( 'NONE',  ( 25.73970730979781152, -279.5114031048926790, -232.1643675973944880 ) ) ;
#71012 = CARTESIAN_POINT ( 'NONE',  ( -24.22524791666972277, -278.1964863749546453, -342.7261405411380792 ) ) ;
#71013 = CARTESIAN_POINT ( 'NONE',  ( 34.68526514554316975, -275.8820380125085876, -258.0351228961662855 ) ) ;
#71014 = CARTESIAN_POINT ( 'NONE',  ( -57.20282309589141079, -288.0976706260811966, -344.3993492817485844 ) ) ;
#71015 = CARTESIAN_POINT ( 'NONE',  ( -65.18412495702396825, -284.2096959302913888, -341.9920363842768438 ) ) ;
#71016 = CARTESIAN_POINT ( 'NONE',  ( -111.0472198917028095, -284.7668147128538862, -292.4754576098026178 ) ) ;
#71017 = CARTESIAN_POINT ( 'NONE',  ( -24.06341276463702528, -283.0444876222459243, -342.1433378505650467 ) ) ;
#71018 = ORIENTED_EDGE ( 'NONE', *, *, #69429, .T. ) ;
#71019 = ORIENTED_EDGE ( 'NONE', *, *, #16970, .T. ) ;
#71020 = DIRECTION ( 'NONE',  ( 1.000000000000000000, 0.000000000000000000, 0.000000000000000000 ) ) ;
#71021 = CARTESIAN_POINT ( 'NONE',  ( -59.64076283008457580, -291.1983806427256809, -342.7700765517646460 ) ) ;
#71022 = CARTESIAN_POINT ( 'NONE',  ( -73.18773698749311052, -290.2719188009806999, -202.7566715567104723 ) ) ;
#71023 = CARTESIAN_POINT ( 'NONE',  ( -33.79202179531848316, -297.2948722605341914, -197.2001395970567046 ) ) ;
#71024 = ADVANCED_FACE ( 'NONE', ( #92202, #5592, #4179 ), #26424, .T. ) ;
#71025 = CARTESIAN_POINT ( 'NONE',  ( 0.4831257527222759807, -293.9104241770919543, -337.3284635517964034 ) ) ;
#71026 = CARTESIAN_POINT ( 'NONE',  ( -108.3994899467361392, -288.7741630443317717, -290.0813334014044358 ) ) ;
#71027 = CARTESIAN_POINT ( 'NONE',  ( 34.63844841391625806, -291.5671854479851959, -253.0780841330124247 ) ) ;
#71028 = CARTESIAN_POINT ( 'NONE',  ( 27.38785085396388297, -289.2276159197001562, -305.0701358544159802 ) ) ;
#71029 = CARTESIAN_POINT ( 'NONE',  ( -54.49178911615187815, -300.3376638359845856, -195.3683826091709363 ) ) ;
#71030 = CARTESIAN_POINT ( 'NONE',  ( -74.64620179888198948, -291.5487809400572701, -335.4255076630119561 ) ) ;
#71031 = CARTESIAN_POINT ( 'NONE',  ( -78.56711798594803042, -289.4987559722096080, -207.4459624674158817 ) ) ;
#71032 = CARTESIAN_POINT ( 'NONE',  ( -68.14284374770194574, -293.6478781926342663, -201.9638501743547181 ) ) ;
#71033 = CARTESIAN_POINT ( 'NONE',  ( -67.65599995281158385, -286.5855699896985698, -203.6943970872609952 ) ) ;
#71034 = CARTESIAN_POINT ( 'NONE',  ( -7.931572173716351593, -294.4366931742251268, -201.1729190378534895 ) ) ;
#71035 = FACE_OUTER_BOUND ( 'NONE', #28505, .T. ) ;
#71036 = ADVANCED_FACE ( 'NONE', ( #25478 ), #5121, .T. ) ;
#71037 = DIRECTION ( 'NONE',  ( 0.000000000000000000, 0.000000000000000000, 1.000000000000000000 ) ) ;
#71038 = CARTESIAN_POINT ( 'NONE',  ( -35.58789420918336077, -276.0539128029232643, -195.0134754155124881 ) ) ;
#71039 = CARTESIAN_POINT ( 'NONE',  ( -113.2284528385501119, -295.9014665725534314, -258.2213182009091383 ) ) ;
#71040 = CARTESIAN_POINT ( 'NONE',  ( 36.60060927247352680, -273.7365971362049208, -266.1027050548266857 ) ) ;
#71041 = CARTESIAN_POINT ( 'NONE',  ( -73.56367644284699736, -275.6165488471139042, -335.4087207316974855 ) ) ;
#71042 = CARTESIAN_POINT ( 'NONE',  ( -35.39509422559458329, -275.2821693190704195, -196.9772883050819416 ) ) ;
#71043 = CARTESIAN_POINT ( 'NONE',  ( 13.58538674600394280, -273.3233641706381150, -213.3251595027922747 ) ) ;
#71044 = CARTESIAN_POINT ( 'NONE',  ( -88.90184662709367558, -297.2188191018969974, -322.9391523296335436 ) ) ;
#71045 = CYLINDRICAL_SURFACE ( 'NONE', #26284, 35.00000000000000000 ) ;
#71046 = CARTESIAN_POINT ( 'NONE',  ( -79.83011133144879068, -298.2636766780665880, -210.8015961583539024 ) ) ;
#71047 = VECTOR ( 'NONE', #59672, 1000.000000000000000 ) ;
#71048 = CARTESIAN_POINT ( 'NONE',  ( -5.802570524182334211, -229.5268262511776527, 22.47499999999998721 ) ) ;
#71050 = CARTESIAN_POINT ( 'NONE',  ( 51.66927062525243031, -299.1969939837661059, -197.3611649956296219 ) ) ;
#71049 = CARTESIAN_POINT ( 'NONE',  ( 34.29348792924363920, -285.2697269482018214, -246.8101712888540078 ) ) ;
#71051 = CARTESIAN_POINT ( 'NONE',  ( 26.35736521459429227, -286.9815187556657179, -227.0775473300800229 ) ) ;
#71052 = CIRCLE ( 'NONE', #93671, 8.222204860432944074 ) ;
#71053 = CARTESIAN_POINT ( 'NONE',  ( -102.2857046502224989, -289.6758900029295205, -311.7874237894229736 ) ) ;
#71054 = CARTESIAN_POINT ( 'NONE',  ( -104.4805427056391380, -298.0804573685408627, -304.6926879629928635 ) ) ;
#71055 = CARTESIAN_POINT ( 'NONE',  ( -9.839340531551428626, -292.6919539707508306, -339.9574443497089078 ) ) ;
#71056 = CARTESIAN_POINT ( 'NONE',  ( -59.24630802888157177, -278.9727894298121100, -196.7109518402720028 ) ) ;
#71057 = CARTESIAN_POINT ( 'NONE',  ( 39.58706461736020543, -285.0523547857347353, -270.3937649182068981 ) ) ;
#71058 = CARTESIAN_POINT ( 'NONE',  ( 154.4030696693785956, 128.9756020784251120, 12.16842021443607180 ) ) ;
#71059 = CARTESIAN_POINT ( 'NONE',  ( -82.80417032364881891, -288.4849050554818746, -327.9831129786138604 ) ) ;
#71060 = CARTESIAN_POINT ( 'NONE',  ( 175.2296996224750103, 160.0000000000000568, 0.000000000000000000 ) ) ;
#71061 = CARTESIAN_POINT ( 'NONE',  ( -99.00746273454316793, -287.9728612830038514, -313.0724997197551716 ) ) ;
#71062 = CARTESIAN_POINT ( 'NONE',  ( -67.16106842550161105, -299.2547051593111860, -202.8399111089550217 ) ) ;
#71063 = CARTESIAN_POINT ( 'NONE',  ( -39.58826171436156471, -281.4497594915775380, -193.9704268204985453 ) ) ;
#71065 = CARTESIAN_POINT ( 'NONE',  ( 1.101307911923784744, -282.5237073002345483, -332.4776586972570271 ) ) ;
#71064 = CARTESIAN_POINT ( 'NONE',  ( -103.1784170829603227, -294.0854131515289396, -307.1275494892859683 ) ) ;
#71066 = CARTESIAN_POINT ( 'NONE',  ( -109.4367899747259969, -296.3750647719400035, -297.5540603233302477 ) ) ;
#71067 = CARTESIAN_POINT ( 'NONE',  ( -69.57813917461248820, -299.1399929613908739, -204.0925752768931716 ) ) ;
#71068 = CARTESIAN_POINT ( 'NONE',  ( 38.16404851057426839, -285.6831058116866302, -274.3713544293959785 ) ) ;
#71069 = CARTESIAN_POINT ( 'NONE',  ( 24.61370853033482220, -282.9788861601489884, -228.0032031214378492 ) ) ;
#71070 = CARTESIAN_POINT ( 'NONE',  ( -100.3750793511504611, -295.0990382903758587, -307.7464054593901324 ) ) ;
#71071 = ORIENTED_EDGE ( 'NONE', *, *, #87140, .F. ) ;
#71072 = CARTESIAN_POINT ( 'NONE',  ( 199.0061125298537377, 250.5000000000000568, -12.72542485937401580 ) ) ;
#71073 = CARTESIAN_POINT ( 'NONE',  ( -10.35817444959822708, -284.6783272466427093, -340.0128696143515867 ) ) ;
#71074 = DIRECTION ( 'NONE',  ( 1.124465274301078034E-16, 1.000000000000000000, 0.000000000000000000 ) ) ;
#71075 = CARTESIAN_POINT ( 'NONE',  ( -85.33152481854864391, -287.1952119285919025, -330.4860931364850671 ) ) ;
#71076 = CARTESIAN_POINT ( 'NONE',  ( 38.76564757903747704, -274.6167894020144900, -259.7861264738814384 ) ) ;
#71077 = CARTESIAN_POINT ( 'NONE',  ( 32.62969052999584818, -293.1080031279846594, -249.3781517199462314 ) ) ;
#71078 = CARTESIAN_POINT ( 'NONE',  ( 34.73934199120477473, -282.8711856018877597, -254.9703439682002397 ) ) ;
#71079 = CARTESIAN_POINT ( 'NONE',  ( 34.36867661861910506, -277.3804864202372187, -287.8517960041486390 ) ) ;
#71080 = CARTESIAN_POINT ( 'NONE',  ( -49.97805349975100597, -284.6354845063489734, -345.7732474453188161 ) ) ;
#71081 = CARTESIAN_POINT ( 'NONE',  ( -97.86845138257616838, -282.7712435999849276, -311.9665010078609271 ) ) ;
#71082 = CARTESIAN_POINT ( 'NONE',  ( -98.50228014096481388, -279.9620341462559736, -313.7929055038277966 ) ) ;
#71083 = CARTESIAN_POINT ( 'NONE',  ( -109.1673689681241797, -273.0719936843019013, -242.4641456104056090 ) ) ;
#71084 = CARTESIAN_POINT ( 'NONE',  ( 27.64768956126589927, -275.9278280799842946, -311.7564625740425868 ) ) ;
#71085 = CARTESIAN_POINT ( 'NONE',  ( 25.65876316291412351, -296.0105492116871915, -310.1096752745310710 ) ) ;
#71086 = CARTESIAN_POINT ( 'NONE',  ( 185.1905923765118587, 275.0000000000000568, 21.83530662808691147 ) ) ;
#71087 = CARTESIAN_POINT ( 'NONE',  ( -87.80074239612507370, -293.8875780899065262, -326.9486608867872519 ) ) ;
#71088 = CARTESIAN_POINT ( 'NONE',  ( 33.89516528870262846, -274.8452658272979647, -254.0787183080210809 ) ) ;
#71089 = CARTESIAN_POINT ( 'NONE',  ( -13.97578042415391586, -296.2744937728448917, -343.0023015346546345 ) ) ;
#71090 = CARTESIAN_POINT ( 'NONE',  ( 25.39830413111177876, -295.3416449737861171, -314.3351323283593501 ) ) ;
#71091 = CARTESIAN_POINT ( 'NONE',  ( 13.41759824623720831, -290.3405140230750590, -325.4181176257684456 ) ) ;
#71092 = CARTESIAN_POINT ( 'NONE',  ( -100.7415431858061510, -276.0153548592995207, -310.2133175259565974 ) ) ;
#71093 = CARTESIAN_POINT ( 'NONE',  ( -103.1181352505607833, -280.0067078608882412, -305.2147372736505986 ) ) ;
#71094 = CARTESIAN_POINT ( 'NONE',  ( -109.3689979981711247, -294.3880186820214817, -289.2100530622470842 ) ) ;
#71095 = CARTESIAN_POINT ( 'NONE',  ( 32.03228451635645513, -283.0178133680506107, -239.9053183300221121 ) ) ;
#71096 = CARTESIAN_POINT ( 'NONE',  ( -54.81675334284438605, -284.7426530091502173, -199.1127542649804809 ) ) ;
#71097 = CARTESIAN_POINT ( 'NONE',  ( -10.98649374757405184, -92.81748071270037315, -359.1663498857263903 ) ) ;
#71098 = ORIENTED_EDGE ( 'NONE', *, *, #3235, .F. ) ;
#71099 = CARTESIAN_POINT ( 'NONE',  ( -107.3740255834325268, -284.4944870705180051, -249.5082399866224421 ) ) ;
#71100 = VERTEX_POINT ( 'NONE', #32602 ) ;
#71101 = CARTESIAN_POINT ( 'NONE',  ( 38.97197785513164803, -282.7336692635807935, -278.4721153531405093 ) ) ;
#71102 = CARTESIAN_POINT ( 'NONE',  ( -95.50496169006194691, -284.0239253035009028, -220.4313640935382637 ) ) ;
#71103 = CARTESIAN_POINT ( 'NONE',  ( -69.87360205621597231, -280.5754186639417753, -200.8162348394174614 ) ) ;
#71104 = CARTESIAN_POINT ( 'NONE',  ( -69.98667028192203077, -278.9944144872179095, -339.3465316473948405 ) ) ;
#71105 = CARTESIAN_POINT ( 'NONE',  ( -53.74683284575205278, -280.4984930536186880, -195.1788329381531071 ) ) ;
#71106 = CIRCLE ( 'NONE', #19724, 4.499999999999993783 ) ;
#71107 = CARTESIAN_POINT ( 'NONE',  ( -109.1418805571601069, -299.0519495502701943, -270.3937649182068412 ) ) ;
#71108 = CARTESIAN_POINT ( 'NONE',  ( 204.5908736159001080, 295.1817123384394677, -68.66699096479933928 ) ) ;
#71109 = ORIENTED_EDGE ( 'NONE', *, *, #25741, .T. ) ;
#71110 = CARTESIAN_POINT ( 'NONE',  ( -33.98326286685349373, -276.0946628066722610, -195.6031797567647175 ) ) ;
#71111 = CARTESIAN_POINT ( 'NONE',  ( -22.58273187492847001, -108.0340517556413147, -362.5798773164220279 ) ) ;
#71112 = AXIS2_PLACEMENT_3D ( 'NONE', #70596, #93284, #485 ) ;
#71113 = CARTESIAN_POINT ( 'NONE',  ( -75.32143482974849746, -277.5636852982876235, -206.0414142660602295 ) ) ;
#71114 = CARTESIAN_POINT ( 'NONE',  ( -72.97857665290149498, -293.3467370114904043, -203.2346619172767817 ) ) ;
#71115 = CARTESIAN_POINT ( 'NONE',  ( 22.67635874622380854, -292.3196178315226916, -228.6050766485717247 ) ) ;
#71116 = CARTESIAN_POINT ( 'NONE',  ( -114.3286190704364600, -290.0490331724351449, -271.2218060457985302 ) ) ;
#71117 = DIRECTION ( 'NONE',  ( 0.000000000000000000, 0.000000000000000000, 1.000000000000000000 ) ) ;
#71119 = CARTESIAN_POINT ( 'NONE',  ( -70.32184978685793908, -284.0099468332284687, -204.3261914499192358 ) ) ;
#71118 = CARTESIAN_POINT ( 'NONE',  ( -36.30082194905342163, -293.6141135822393835, -346.7778052962706283 ) ) ;
#71120 = CARTESIAN_POINT ( 'NONE',  ( -33.46726754236494372, -293.9618258522103815, -196.2143852620230291 ) ) ;
#71121 = CARTESIAN_POINT ( 'NONE',  ( 5.140709190119024719, -285.1177898088805591, -210.0827781962700840 ) ) ;
#71122 = CARTESIAN_POINT ( 'NONE',  ( -3.378693778027990646, -283.9091123691318899, -335.5500429987772009 ) ) ;
#71123 = EDGE_LOOP ( 'NONE', ( #19272, #67142 ) ) ;
#71124 = CARTESIAN_POINT ( 'NONE',  ( -33.56297233337575392, -293.0398747076706059, -193.6894711398170443 ) ) ;
#71125 = CARTESIAN_POINT ( 'NONE',  ( 24.18564823801470709, -282.5902013626234748, -309.8543107402443866 ) ) ;
#71126 = CARTESIAN_POINT ( 'NONE',  ( 33.04561821504316299, -292.7355944149769584, -300.7213966613971934 ) ) ;
#71127 = CARTESIAN_POINT ( 'NONE',  ( -17.75560214892808375, -289.6085933106230073, -344.6614785871051936 ) ) ;
#71128 = CARTESIAN_POINT ( 'NONE',  ( -43.17137395567311131, -289.6162505669918801, -347.0784029078412800 ) ) ;
#71129 = CARTESIAN_POINT ( 'NONE',  ( 19.51385372131342422, -287.0712562193587019, -224.5543500988575829 ) ) ;
#71130 = ORIENTED_EDGE ( 'NONE', *, *, #36693, .T. ) ;
#71131 = PLANE ( 'NONE',  #18640 ) ;
#71132 = CARTESIAN_POINT ( 'NONE',  ( -63.81208506680439996, -297.2540805457130659, -341.3514285980028831 ) ) ;
#71133 = CARTESIAN_POINT ( 'NONE',  ( -101.1292185153662047, -295.7965146306008819, -228.0945100987094065 ) ) ;
#71134 = CARTESIAN_POINT ( 'NONE',  ( -103.3482622026562012, -277.1816553580022742, -302.2045485854078493 ) ) ;
#71135 = EDGE_CURVE ( 'NONE', #49439, #52696, #91196, .T. ) ;
#71136 = CARTESIAN_POINT ( 'NONE',  ( -73.91008298179929170, -273.0878264126634463, -202.6093528009212150 ) ) ;
#71137 = CARTESIAN_POINT ( 'NONE',  ( -67.59740104981793252, -293.9363353241926120, -337.5709406013941702 ) ) ;
#71138 = CARTESIAN_POINT ( 'NONE',  ( 36.65556519529913260, -277.2922338544670993, -268.8188029703112534 ) ) ;
#71139 = CARTESIAN_POINT ( 'NONE',  ( -111.5760183017738854, -270.7279678523428856, -267.5675363796792112 ) ) ;
#71140 = CARTESIAN_POINT ( 'NONE',  ( -104.2925540072696293, -297.3527687345801951, -300.5637557906787265 ) ) ;
#71141 = CARTESIAN_POINT ( 'NONE',  ( -107.1594597061730383, -297.3346759082611470, -292.8794707580600516 ) ) ;
#71142 = CARTESIAN_POINT ( 'NONE',  ( 164.2231345125756263, 250.5000000000000568, 22.80382896337008702 ) ) ;
#71143 = CARTESIAN_POINT ( 'NONE',  ( -36.26509739655411835, -296.6390247100388819, -346.5664821968878755 ) ) ;
#71144 = CARTESIAN_POINT ( 'NONE',  ( -111.8392290246089402, -294.4188869387747900, -280.7506060141661237 ) ) ;
#71145 = CARTESIAN_POINT ( 'NONE',  ( -111.6647335822579095, -273.6019179559034455, -250.6574968307645577 ) ) ;
#71146 = CARTESIAN_POINT ( 'NONE',  ( -102.1707620524067295, -288.6545596536325888, -305.2911486288720653 ) ) ;
#71147 = CARTESIAN_POINT ( 'NONE',  ( -72.87722998788049722, -275.5819331601612134, -204.2560866829686574 ) ) ;
#71148 = CARTESIAN_POINT ( 'NONE',  ( -109.1114665446813206, -273.3976083949872873, -242.4903039726218879 ) ) ;
#71149 = CARTESIAN_POINT ( 'NONE',  ( -109.2974171359836788, -297.0493369894550710, -257.9328326343158437 ) ) ;
#71150 = CARTESIAN_POINT ( 'NONE',  ( -53.43434310871793969, -281.8267582749264761, -196.6909084885670040 ) ) ;
#71151 = CARTESIAN_POINT ( 'NONE',  ( 8.266075918669939071, -279.3460740564684670, -208.8686381655618050 ) ) ;
#71152 = EDGE_LOOP ( 'NONE', ( #59709, #70531, #32991, #34083 ) ) ;
#71153 = CARTESIAN_POINT ( 'NONE',  ( 21.52662368116387626, -281.5678167806487409, -319.8367002313106013 ) ) ;
#71154 = CARTESIAN_POINT ( 'NONE',  ( 37.13794643748232716, -275.1405084822180243, -289.4947280554013105 ) ) ;
#71155 = CARTESIAN_POINT ( 'NONE',  ( 12.48460853774552604, -279.1329237015384024, -212.7088901135653600 ) ) ;
#71156 = CARTESIAN_POINT ( 'NONE',  ( -93.57296505719520496, -277.2443382476839702, -220.4805278424888684 ) ) ;
#71157 = EDGE_CURVE ( 'NONE', #70, #46709, #93332, .T. ) ;
#71158 = CARTESIAN_POINT ( 'NONE',  ( -87.72359660053737684, -271.9067572238526509, -216.6533259070059216 ) ) ;
#71159 = CARTESIAN_POINT ( 'NONE',  ( 35.98171872038178520, -277.7555091975439154, -286.1901677788409870 ) ) ;
#71160 = FACE_OUTER_BOUND ( 'NONE', #25072, .T. ) ;
#71161 = CARTESIAN_POINT ( 'NONE',  ( 184.1778392089217107, 3.000000000000000000, 10.00000000000000178 ) ) ;
#71162 = CARTESIAN_POINT ( 'NONE',  ( -100.6923248960869444, -295.3516191973229184, -228.3770683574962845 ) ) ;
#71163 = CARTESIAN_POINT ( 'NONE',  ( 0.8878766968512699087, -290.5791947935748567, -205.3637653945487500 ) ) ;
#71164 = CARTESIAN_POINT ( 'NONE',  ( -95.66091589783415827, -291.2312609012022335, -220.0630462660494970 ) ) ;
#71165 = EDGE_CURVE ( 'NONE', #557, #72022, #56434, .T. ) ;
#71166 = CARTESIAN_POINT ( 'NONE',  ( 2.550636152687149938, -278.5192513579186198, -334.1297771630124203 ) ) ;
#71167 = CARTESIAN_POINT ( 'NONE',  ( -66.56969732517289629, -271.6691758511835815, -201.2906841448159696 ) ) ;
#71168 = DIRECTION ( 'NONE',  ( -1.000000000000000000, 0.000000000000000000, 0.000000000000000000 ) ) ;
#71169 = CARTESIAN_POINT ( 'NONE',  ( -55.33512605364504822, -285.2020442254257659, -343.7474301847148013 ) ) ;
#71170 = DIRECTION ( 'NONE',  ( -0.000000000000000000, -1.000000000000000000, -0.000000000000000000 ) ) ;
#71171 = CARTESIAN_POINT ( 'NONE',  ( -91.23782066981317485, -281.8177728978624259, -322.5895926092773038 ) ) ;
#71172 = CARTESIAN_POINT ( 'NONE',  ( 221.8344101925596306, 15.36528803885690664, 22.50000000000000000 ) ) ;
#71173 = CARTESIAN_POINT ( 'NONE',  ( 19.12882268324476343, -293.0084871546870886, -317.2461961995161346 ) ) ;
#71174 = CARTESIAN_POINT ( 'NONE',  ( 20.49216839403380419, -285.0444886364653598, -223.7994926256597807 ) ) ;
#71175 = DIRECTION ( 'NONE',  ( 0.000000000000000000, -1.000000000000000000, 0.000000000000000000 ) ) ;
#71176 = CARTESIAN_POINT ( 'NONE',  ( -45.32835983327135665, -293.1530363356147291, -344.9865251391520928 ) ) ;
#71177 = CARTESIAN_POINT ( 'NONE',  ( -111.6798620076071984, -283.2493622608496366, -253.1406230943017874 ) ) ;
#71178 = CARTESIAN_POINT ( 'NONE',  ( -72.52888815605126638, -281.1782274276820317, -205.4896896412770104 ) ) ;
#71179 = CARTESIAN_POINT ( 'NONE',  ( -63.08252603085015409, -286.9292845945221302, -198.2125310249039956 ) ) ;
#71180 = CARTESIAN_POINT ( 'NONE',  ( 22.95705254234390935, -279.1668047485427451, -224.1009697138881052 ) ) ;
#71181 = CARTESIAN_POINT ( 'NONE',  ( 33.99600683975054238, -287.3478169724168652, -254.8713934991565395 ) ) ;
#71182 = CARTESIAN_POINT ( 'NONE',  ( -107.6744403733134305, -279.6909400585233811, -292.1806430036223787 ) ) ;
#71183 = CARTESIAN_POINT ( 'NONE',  ( -87.64906402838282418, -280.1309426497939512, -217.1707527470145749 ) ) ;
#71184 = CARTESIAN_POINT ( 'NONE',  ( -96.30940390701977094, -287.1738436537719394, -223.4439919097640370 ) ) ;
#71185 = AXIS2_PLACEMENT_3D ( 'NONE', #33329, #40404, #56059 ) ;
#71186 = ORIENTED_EDGE ( 'NONE', *, *, #6503, .F. ) ;
#71187 = CARTESIAN_POINT ( 'NONE',  ( -89.60674544234061045, -297.1730543878309732, -213.7436443667388914 ) ) ;
#71189 = CARTESIAN_POINT ( 'NONE',  ( 36.59295671128113270, -289.6657690718142248, -280.7263723183225466 ) ) ;
#71188 = VECTOR ( 'NONE', #68372, 1000.000000000000000 ) ;
#71190 = CARTESIAN_POINT ( 'NONE',  ( 169.2744399300530347, -11.64849832608277325, 13.00000000000000178 ) ) ;
#71191 = CARTESIAN_POINT ( 'NONE',  ( 40.65961533371913106, -284.2662352645559167, -288.1317622949166548 ) ) ;
#71192 = ORIENTED_EDGE ( 'NONE', *, *, #89368, .T. ) ;
#71193 = CARTESIAN_POINT ( 'NONE',  ( 32.03159489696659534, -273.1734711455305842, -241.2891532907173371 ) ) ;
#71194 = CARTESIAN_POINT ( 'NONE',  ( 32.59827851968617551, -291.5625646331923235, -240.1147991936883557 ) ) ;
#71195 = CARTESIAN_POINT ( 'NONE',  ( -49.95838822131641876, -297.3944571262421732, -198.3971851894851284 ) ) ;
#71196 = CARTESIAN_POINT ( 'NONE',  ( 22.54379778067782070, -288.4765996302595568, -227.3282294425881958 ) ) ;
#71197 = CARTESIAN_POINT ( 'NONE',  ( 35.56141040672193299, -283.1461264425809077, -257.5896462922316346 ) ) ;
#71198 = CARTESIAN_POINT ( 'NONE',  ( -104.6284536667436669, -291.5056410137439684, -306.5702202861667161 ) ) ;
#71199 = CARTESIAN_POINT ( 'NONE',  ( -98.62400573995364539, -291.2537730180500830, -316.1842751939321943 ) ) ;
#71200 = CARTESIAN_POINT ( 'NONE',  ( -110.3172948394246333, -286.7751970360466771, -252.9978314765042740 ) ) ;
#71201 = CARTESIAN_POINT ( 'NONE',  ( -59.66298242062732271, -277.5001923794367826, -344.0548108015921116 ) ) ;
#71202 = ORIENTED_EDGE ( 'NONE', *, *, #89067, .T. ) ;
#71203 = CARTESIAN_POINT ( 'NONE',  ( -34.92564695030645083, -293.1018725119407691, -345.8824850763513155 ) ) ;
#71204 = CARTESIAN_POINT ( 'NONE',  ( 39.41187872584406193, -281.3084916093469587, -264.2057839050835923 ) ) ;
#71205 = CARTESIAN_POINT ( 'NONE',  ( 19.93705533788776663, -276.7544095775580217, -223.1381399350777883 ) ) ;
#71206 = CARTESIAN_POINT ( 'NONE',  ( -82.08285599513421005, -280.1948066931273615, -326.5171145203363494 ) ) ;
#71207 = CARTESIAN_POINT ( 'NONE',  ( 38.61848655886215909, -273.7665885328542572, -268.3551145334367334 ) ) ;
#71208 = CARTESIAN_POINT ( 'NONE',  ( 215.7837434059060229, -147.7221692137691775, 8.778910157967997563 ) ) ;
#71209 = CARTESIAN_POINT ( 'NONE',  ( 0.4371355078812793060, -280.0775711935852996, -207.7665775492066302 ) ) ;
#71210 = CARTESIAN_POINT ( 'NONE',  ( -91.03969113989829509, -278.9990767769909326, -325.0662779953688073 ) ) ;
#71211 = CARTESIAN_POINT ( 'NONE',  ( -63.49778399579081167, -275.0192065503160848, -201.6663645440007429 ) ) ;
#71212 = CARTESIAN_POINT ( 'NONE',  ( -67.08678917969932343, -284.7303750366101553, -199.5935414335779967 ) ) ;
#71213 = CARTESIAN_POINT ( 'NONE',  ( -109.9281863996342423, -292.1232755092998445, -284.8887651978565714 ) ) ;
#71214 = CARTESIAN_POINT ( 'NONE',  ( -31.34357104310445763, -275.7268071014981956, -194.3844119261464130 ) ) ;
#71215 = CARTESIAN_POINT ( 'NONE',  ( -83.29732934001472699, -274.7527717440063952, -209.1279932916463622 ) ) ;
#71216 = DIRECTION ( 'NONE',  ( 1.000000000000000000, 0.000000000000000000, 0.000000000000000000 ) ) ;
#71217 = CARTESIAN_POINT ( 'NONE',  ( -112.0711609299673910, -298.5015950478284594, -274.3027054896107302 ) ) ;
#71218 = CARTESIAN_POINT ( 'NONE',  ( -109.1583620544447939, -282.2800102413123682, -291.4401240812232459 ) ) ;
#71219 = CARTESIAN_POINT ( 'NONE',  ( -114.1664693979008263, -290.2797717242427211, -265.4929439832420712 ) ) ;
#71220 = CARTESIAN_POINT ( 'NONE',  ( 4.025136767110162772, -274.5119387591219606, -332.4950990723469317 ) ) ;
#71221 = CARTESIAN_POINT ( 'NONE',  ( 9.304787896971838279, -288.2812600259862279, -210.1071092500549753 ) ) ;
#71222 = CARTESIAN_POINT ( 'NONE',  ( -110.5534919926727184, -289.5336725926654822, -265.7023306903804496 ) ) ;
#71223 = ORIENTED_EDGE ( 'NONE', *, *, #15862, .F. ) ;
#71224 = CARTESIAN_POINT ( 'NONE',  ( -104.6456110209736181, -288.6555553013054691, -306.5383189512274384 ) ) ;
#71225 = CARTESIAN_POINT ( 'NONE',  ( -108.4470887267320052, -290.4387262007506365, -253.6900082406413048 ) ) ;
#71226 = VERTEX_POINT ( 'NONE', #75672 ) ;
#71227 = CARTESIAN_POINT ( 'NONE',  ( 39.39339127847529198, -288.6465345582640225, -271.5327885895955546 ) ) ;
#71228 = CARTESIAN_POINT ( 'NONE',  ( -94.81012767768720551, -279.5206241622084917, -225.2913814188073047 ) ) ;
#71229 = ADVANCED_FACE ( 'NONE', ( #55777 ), #92705, .T. ) ;
#71230 = CARTESIAN_POINT ( 'NONE',  ( -84.00804977312975552, -294.5964901115760313, -331.2864785464611828 ) ) ;
#71231 = CARTESIAN_POINT ( 'NONE',  ( -86.03141575334062452, -284.3584066722862644, -329.8810673995528191 ) ) ;
#71232 = CARTESIAN_POINT ( 'NONE',  ( -36.56990796445238345, -286.3948696416265989, -193.3730956640566774 ) ) ;
#71233 = CARTESIAN_POINT ( 'NONE',  ( 22.60455508182450757, -282.4664161788334127, -312.0568488564973109 ) ) ;
#71234 = CARTESIAN_POINT ( 'NONE',  ( -48.27666066358466423, -154.8625263976673807, -365.1983507399203290 ) ) ;
#71235 = CARTESIAN_POINT ( 'NONE',  ( 198.2119960356330068, 289.1949541700149098, -97.17456560034590041 ) ) ;
#71236 = CARTESIAN_POINT ( 'NONE',  ( 137.5249753115113833, 179.0922514384929514, -238.4867443683607462 ) ) ;
#71237 = CARTESIAN_POINT ( 'NONE',  ( -24.55819114827195904, -273.4165044668659448, -198.2734257282029660 ) ) ;
#71238 = CARTESIAN_POINT ( 'NONE',  ( -19.18181074326775715, -273.2115671961610133, -199.2842135568791662 ) ) ;
#71239 = CARTESIAN_POINT ( 'NONE',  ( -65.58674650670324979, -294.9193915616468189, -341.9416917330253796 ) ) ;
#71240 = CARTESIAN_POINT ( 'NONE',  ( 180.4165302251282981, 251.0051037841290054, -164.4917810413223549 ) ) ;
#71241 = CARTESIAN_POINT ( 'NONE',  ( -35.51864135670681577, -272.7593795388713716, -193.8629445613833013 ) ) ;
#71242 = CARTESIAN_POINT ( 'NONE',  ( -106.9725360597648205, -298.7517750038622353, -244.4753471587631566 ) ) ;
#71243 = CARTESIAN_POINT ( 'NONE',  ( -77.43566305231442470, -292.5798602431752897, -208.9876692430420064 ) ) ;
#71244 = VERTEX_POINT ( 'NONE', #34466 ) ;
#71245 = CARTESIAN_POINT ( 'NONE',  ( -105.7425838429125378, -297.0419842968203170, -305.3226787405124583 ) ) ;
#71246 = SHAPE_REPRESENTATION ( 'L sheet band', ( #18940 ), #2252 ) ;
#71247 = CARTESIAN_POINT ( 'NONE',  ( -34.56939098001380017, -289.5088680095021232, -343.4196635109688600 ) ) ;
#71248 = CARTESIAN_POINT ( 'NONE',  ( -3.291124993926298981, -295.4168373338897027, -339.2575993944697643 ) ) ;
#71249 = CARTESIAN_POINT ( 'NONE',  ( -77.04509521186594156, -296.0611028403902765, -336.3258073262312564 ) ) ;
#71250 = CARTESIAN_POINT ( 'NONE',  ( 26.23351112299397769, -293.2265036997508787, -234.3804449044959881 ) ) ;
#71251 = ORIENTED_EDGE ( 'NONE', *, *, #27503, .F. ) ;
#71252 = CARTESIAN_POINT ( 'NONE',  ( 29.28508072594790335, -277.9429568179117496, -306.1113322268128059 ) ) ;
#71253 = ORIENTED_EDGE ( 'NONE', *, *, #54587, .T. ) ;
#71254 = EDGE_CURVE ( 'NONE', #21613, #25416, #63372, .T. ) ;
#71255 = CARTESIAN_POINT ( 'NONE',  ( -114.1490536736508403, -278.1160007762876489, -265.8714248523405672 ) ) ;
#71256 = CARTESIAN_POINT ( 'NONE',  ( 35.58941446579279244, -276.5810874108776716, -277.0290240886006927 ) ) ;
#71257 = CARTESIAN_POINT ( 'NONE',  ( -1.795634698020047493, -276.2766762443887387, -203.2012248316537182 ) ) ;
#71258 = AXIS2_PLACEMENT_3D ( 'NONE', #24238, #2485, #2934 ) ;
#71259 = CARTESIAN_POINT ( 'NONE',  ( 19.56129288270044242, -274.2546427920289034, -319.7816128438179248 ) ) ;
#71260 = CARTESIAN_POINT ( 'NONE',  ( -41.88295005433539586, -298.6448310457113280, -197.4003770499783457 ) ) ;
#71261 = CARTESIAN_POINT ( 'NONE',  ( -108.1748622820848880, -294.8652590384936047, -290.3120091230533149 ) ) ;
#71262 = PLANE ( 'NONE',  #44177 ) ;
#71263 = CARTESIAN_POINT ( 'NONE',  ( -114.0172163562985617, -278.9572510882937308, -277.3317464269327388 ) ) ;
#71264 = CARTESIAN_POINT ( 'NONE',  ( -39.15563525293699598, -277.2422278009347565, -343.3385778170336948 ) ) ;
#71265 = CARTESIAN_POINT ( 'NONE',  ( -36.55358155725070901, -284.7466815336893546, -193.8453704683005867 ) ) ;
#71266 = CARTESIAN_POINT ( 'NONE',  ( -88.38255267908760970, -299.3395460214596824, -215.1103382808467472 ) ) ;
#71267 = CARTESIAN_POINT ( 'NONE',  ( 82.68068823132855982, -297.0576872996817883, -195.5766972444398277 ) ) ;
#71268 = CARTESIAN_POINT ( 'NONE',  ( -3.300329454211856195, -287.7880372195716632, -335.1766745257123148 ) ) ;
#71269 = EDGE_CURVE ( 'NONE', #67510, #13434, #83231, .T. ) ;
#71270 = CARTESIAN_POINT ( 'NONE',  ( -13.96789683373837043, -278.5993066953135440, -200.0812993349136093 ) ) ;
#71271 = CARTESIAN_POINT ( 'NONE',  ( -30.18717691561256444, -278.7190183630609113, -197.0697410520693609 ) ) ;
#71272 = CARTESIAN_POINT ( 'NONE',  ( -80.26349666223615031, -287.4714558594855589, -208.7946902293803362 ) ) ;
#71273 = CARTESIAN_POINT ( 'NONE',  ( -37.79690201333477262, -278.2630203141016523, -343.7693015118818494 ) ) ;
#71274 = CARTESIAN_POINT ( 'NONE',  ( 113.5000000000000568, -296.0521521680024080, -537.7509286889328450 ) ) ;
#71275 = CARTESIAN_POINT ( 'NONE',  ( -108.7917012335690998, -276.4592604694012721, -296.3777157158555724 ) ) ;
#71276 = CARTESIAN_POINT ( 'NONE',  ( 23.87433217131118823, -275.6506605213479020, -230.4050163498186521 ) ) ;
#71277 = CARTESIAN_POINT ( 'NONE',  ( 36.08038257627535472, -283.7593415663213250, -286.5211524010406947 ) ) ;
#71278 = DIRECTION ( 'NONE',  ( 0.000000000000000000, 0.000000000000000000, -1.000000000000000000 ) ) ;
#71279 = CARTESIAN_POINT ( 'NONE',  ( 38.19986181628766531, -289.4510330571735608, -268.6918024929133821 ) ) ;
#71280 = CARTESIAN_POINT ( 'NONE',  ( -37.21641030581353249, -290.0535995824776592, -195.3486460966812501 ) ) ;
#71281 = DIRECTION ( 'NONE',  ( -0.000000000000000000, -0.000000000000000000, -1.000000000000000000 ) ) ;
#71282 = CARTESIAN_POINT ( 'NONE',  ( 17.66572841636178737, -273.5445591991725109, -221.5473438095443726 ) ) ;
#71283 = CARTESIAN_POINT ( 'NONE',  ( 31.00203996097383197, -291.3075500401632212, -241.2467744551517228 ) ) ;
#71284 = CARTESIAN_POINT ( 'NONE',  ( 84.09003387609358526, 83.72762891241104910, -302.5758382668069544 ) ) ;
#71285 = DIRECTION ( 'NONE',  ( 0.000000000000000000, -1.000000000000000000, 0.000000000000000000 ) ) ;
#71286 = CARTESIAN_POINT ( 'NONE',  ( -37.51958215299946175, -287.5341899270762269, -346.6805335928127647 ) ) ;
#71287 = CARTESIAN_POINT ( 'NONE',  ( -92.24673890178284807, -285.4539155900227456, -319.6941935321918891 ) ) ;
#71288 = CARTESIAN_POINT ( 'NONE',  ( 9.207898403482005278, -284.9215312258402832, -210.3019064671752858 ) ) ;
#71289 = CARTESIAN_POINT ( 'NONE',  ( -98.00789117072753243, -285.4011671194150495, -312.1030888942941601 ) ) ;
#71290 = EDGE_CURVE ( 'NONE', #28813, #34201, #11051, .T. ) ;
#71291 = CARTESIAN_POINT ( 'NONE',  ( -42.93508183178217763, -283.9272458198304889, -343.3586650328691121 ) ) ;
#71292 = CARTESIAN_POINT ( 'NONE',  ( -111.0368374297748488, -292.7338024474436224, -254.5701208483027642 ) ) ;
#71293 = CARTESIAN_POINT ( 'NONE',  ( 32.39416771235466541, -273.2534646911319669, -241.1359645824260554 ) ) ;
#71294 = CARTESIAN_POINT ( 'NONE',  ( -41.19595950263610007, -274.3383013758099764, -193.4265667472966186 ) ) ;
#71295 = CARTESIAN_POINT ( 'NONE',  ( -112.2354221227958107, -288.7644722007285054, -259.9667589313752956 ) ) ;
#71296 = CARTESIAN_POINT ( 'NONE',  ( -28.60103679366061868, -276.9443428542415973, -346.9169861407146414 ) ) ;
#71297 = CARTESIAN_POINT ( 'NONE',  ( 13.49307001322679866, -296.3166846005143498, -325.0915939867428506 ) ) ;
#71298 = CARTESIAN_POINT ( 'NONE',  ( -55.80257052418233599, -229.5268262511776527, 22.50000000000000000 ) ) ;
#71299 = CARTESIAN_POINT ( 'NONE',  ( -95.33595429735161986, -283.8690164008716010, -225.1974727807570389 ) ) ;
#71300 = CARTESIAN_POINT ( 'NONE',  ( -72.79708432511026217, -277.5824163068654116, -204.2563438829853908 ) ) ;
#71301 = LINE ( 'NONE', #42389, #4448 ) ;
#71302 = CARTESIAN_POINT ( 'NONE',  ( -64.63385711970310865, -272.1821061786632185, -199.0880557362332866 ) ) ;
#71303 = CARTESIAN_POINT ( 'NONE',  ( -93.68989878019139894, -277.2412800259394885, -316.9508224767259321 ) ) ;
#71304 = CARTESIAN_POINT ( 'NONE',  ( 12.84104884053895468, -295.8569884145592823, -324.3977272391306883 ) ) ;
#71305 = CARTESIAN_POINT ( 'NONE',  ( 18.94268244307061266, -279.7600730235698734, -218.2692684433834529 ) ) ;
#71306 = CARTESIAN_POINT ( 'NONE',  ( 3.958929688774724731, -295.4217909888135978, -330.8397623485831218 ) ) ;
#71307 = CARTESIAN_POINT ( 'NONE',  ( -22.17880000799752693, -296.1770039131457111, -345.3503487520475801 ) ) ;
#71308 = CARTESIAN_POINT ( 'NONE',  ( -97.85833484114162673, -272.7877700927374462, -229.4074339833789509 ) ) ;
#71309 = CARTESIAN_POINT ( 'NONE',  ( -95.86716431267517180, -293.1976446539002836, -223.4389891019135064 ) ) ;
#71310 = CARTESIAN_POINT ( 'NONE',  ( -114.3407763534793133, -284.7235490238601869, -269.9839377611181703 ) ) ;
#71311 = CARTESIAN_POINT ( 'NONE',  ( -63.11429437396755304, -271.8595950360511324, -199.1145119892237858 ) ) ;
#71312 = CARTESIAN_POINT ( 'NONE',  ( 39.09029681861581196, -287.5075871118602322, -280.1252899188548326 ) ) ;
#71313 = CARTESIAN_POINT ( 'NONE',  ( -52.17841053344522351, -281.8413174996396720, -197.1527759572261971 ) ) ;
#71314 = CARTESIAN_POINT ( 'NONE',  ( -70.07688052730672723, -284.6687166075377036, -204.8351735597303218 ) ) ;
#71315 = CARTESIAN_POINT ( 'NONE',  ( -31.99545433121289761, -286.9846679685006166, -345.2215219216343485 ) ) ;
#71316 = CARTESIAN_POINT ( 'NONE',  ( -101.2450674239233592, -254.4445186991787295, -323.9438275447045612 ) ) ;
#71317 = CARTESIAN_POINT ( 'NONE',  ( -25.12536402201791930, -285.7196489527982521, -198.2768005689917175 ) ) ;
#71318 = AXIS2_PLACEMENT_3D ( 'NONE', #93200, #77601, #56297 ) ;
#71319 = CARTESIAN_POINT ( 'NONE',  ( -38.71627898499669129, -284.0102451876064720, -347.1135169473235464 ) ) ;
#71320 = CARTESIAN_POINT ( 'NONE',  ( -112.6395549005616914, -289.4227131745509496, -285.3627656624889255 ) ) ;
#71321 = CARTESIAN_POINT ( 'NONE',  ( -74.63438397662177692, -281.1645436758938672, -203.9104133411500186 ) ) ;
#71322 = CARTESIAN_POINT ( 'NONE',  ( -99.24084800811483831, -279.2666289216291489, -315.3477493140125603 ) ) ;
#71323 = CARTESIAN_POINT ( 'NONE',  ( 19.67734598586952899, -280.7414879347180090, -224.7779151025930275 ) ) ;
#71324 = CARTESIAN_POINT ( 'NONE',  ( 37.64196114685309169, -277.5322144740228509, -268.7954911116262338 ) ) ;
#71325 = CARTESIAN_POINT ( 'NONE',  ( 21.36765032522750829, -294.2237324663467462, -320.1829221384771245 ) ) ;
#71326 = CARTESIAN_POINT ( 'NONE',  ( -15.39151440710578100, -286.7868564360038590, -341.7596160424234881 ) ) ;
#71327 = AXIS2_PLACEMENT_3D ( 'NONE', #31559, #73717, #38169 ) ;
#71328 = CARTESIAN_POINT ( 'NONE',  ( -110.6936164896955859, -295.4581172883108593, -271.4540624634458936 ) ) ;
#71329 = EDGE_LOOP ( 'NONE', ( #6281, #44054, #68369, #3651, #44978 ) ) ;
#71330 = EDGE_LOOP ( 'NONE', ( #84245, #61273, #86327, #60268 ) ) ;
#71331 = CARTESIAN_POINT ( 'NONE',  ( 22.99316106881965638, -284.0706602695782976, -313.9836256508349948 ) ) ;
#71332 = CARTESIAN_POINT ( 'NONE',  ( -66.06536231592032493, -295.1054502257089212, -337.4956003098182578 ) ) ;
#71333 = CARTESIAN_POINT ( 'NONE',  ( 35.15587675956225411, -294.3134460322865493, -245.1885792623658631 ) ) ;
#71334 = CARTESIAN_POINT ( 'NONE',  ( -56.33740688475722891, -283.9548921245145152, -340.9518807824663895 ) ) ;
#71335 = CARTESIAN_POINT ( 'NONE',  ( -31.26669625731216939, -273.1858367891194348, -193.8239296604105277 ) ) ;
#71336 = CARTESIAN_POINT ( 'NONE',  ( -89.41635397459970136, -290.4144857261113657, -326.9432990389424276 ) ) ;
#71337 = CARTESIAN_POINT ( 'NONE',  ( -89.60354244762366704, -281.9186581479480651, -325.2874780045280545 ) ) ;
#71338 = CARTESIAN_POINT ( 'NONE',  ( -103.7780316256559274, -290.3780176433012912, -309.3504474542032199 ) ) ;
#71339 = CARTESIAN_POINT ( 'NONE',  ( 24.25846200230541072, -288.4274304494380772, -309.5721816287082220 ) ) ;
#71340 = DIRECTION ( 'NONE',  ( -1.000000000000000000, -0.000000000000000000, -0.000000000000000000 ) ) ;
#71341 = CARTESIAN_POINT ( 'NONE',  ( 197.7051530045995094, 41.80213891112347824, 12.00000000000000000 ) ) ;
#71342 = CARTESIAN_POINT ( 'NONE',  ( 167.6084280626006944, 229.7879449464658421, -189.9070988384416410 ) ) ;
#71343 = CARTESIAN_POINT ( 'NONE',  ( -54.42813229853333468, -277.3380690714490697, -195.3538533559490702 ) ) ;
#71344 = EDGE_LOOP ( 'NONE', ( #55159, #37901, #80900, #81056 ) ) ;
#71345 = CARTESIAN_POINT ( 'NONE',  ( -11.62187183220122044, -279.3153257988083169, -201.6582016399473503 ) ) ;
#71346 = CARTESIAN_POINT ( 'NONE',  ( 9.500835673342779231, -274.3434189508841428, -209.2749400768466614 ) ) ;
#71347 = CARTESIAN_POINT ( 'NONE',  ( -39.17784308802448834, -279.0754116944869452, -345.1719260844724317 ) ) ;
#71348 = CARTESIAN_POINT ( 'NONE',  ( 186.5835289679585571, 260.6838375247356225, -151.8520429253792088 ) ) ;
#71349 = CARTESIAN_POINT ( 'NONE',  ( -113.1302542624162726, -277.2545904217303132, -260.2278703014147823 ) ) ;
#71350 = CARTESIAN_POINT ( 'NONE',  ( -70.97818951900022455, -281.5182739647821109, -337.0119904641340440 ) ) ;
#71351 = CARTESIAN_POINT ( 'NONE',  ( -103.7068162096752673, -297.8248444825496222, -307.4773476484015191 ) ) ;
#71352 = CARTESIAN_POINT ( 'NONE',  ( -0.7216792812276195956, -295.0443016268835663, -333.6403975773210959 ) ) ;
#71353 = ORIENTED_EDGE ( 'NONE', *, *, #48163, .T. ) ;
#71354 = CARTESIAN_POINT ( 'NONE',  ( -102.0854682574641430, -288.7646402153769145, -305.2467552421152277 ) ) ;
#71355 = CARTESIAN_POINT ( 'NONE',  ( 1.137220292409873545, -275.2032020103217178, -203.7674380173210409 ) ) ;
#71356 = CARTESIAN_POINT ( 'NONE',  ( -107.9400821963975687, -272.7996867053294636, -251.5966473179044840 ) ) ;
#71357 = ORIENTED_EDGE ( 'NONE', *, *, #6382, .F. ) ;
#71358 = SURFACE_STYLE_USAGE ( .BOTH. , #78460 ) ;
#71359 = CARTESIAN_POINT ( 'NONE',  ( 222.8344101925596306, -44.55766379199612004, -21.49999999999998579 ) ) ;
#71360 = ADVANCED_FACE ( 'NONE', ( #85107 ), #20257, .T. ) ;
#71361 = EDGE_CURVE ( 'NONE', #60279, #93705, #15012, .T. ) ;
#71362 = CARTESIAN_POINT ( 'NONE',  ( 184.7149167944524493, 8.542400036368780647, 13.00000000000000178 ) ) ;
#71363 = CARTESIAN_POINT ( 'NONE',  ( -67.44574272812705829, -280.7274322649572582, -203.5045570478806098 ) ) ;
#71364 = CARTESIAN_POINT ( 'NONE',  ( -64.40269168991542870, -281.4640483969555476, -199.3008551396109738 ) ) ;
#71365 = CARTESIAN_POINT ( 'NONE',  ( -92.74496407832654654, -282.9305115132227684, -318.2747440884989487 ) ) ;
#71366 = CARTESIAN_POINT ( 'NONE',  ( -34.28580327928959548, -281.9513627311629875, -196.1760830298977680 ) ) ;
#71367 = CARTESIAN_POINT ( 'NONE',  ( 17.94266555293387100, -274.7215094061202763, -319.1074171479883717 ) ) ;
#71368 = CARTESIAN_POINT ( 'NONE',  ( 180.2296971224742776, 215.0000000000000568, -25.00500000000002387 ) ) ;
#71369 = LINE ( 'NONE', #13606, #87964 ) ;
#71370 = CARTESIAN_POINT ( 'NONE',  ( -96.01924808991735460, -278.6849791212837317, -319.9909397655279690 ) ) ;
#71371 = CARTESIAN_POINT ( 'NONE',  ( 165.0461196878273711, 214.7033826592484616, 22.86486864458202817 ) ) ;
#71372 = ORIENTED_EDGE ( 'NONE', *, *, #21877, .F. ) ;
#71373 = DIRECTION ( 'NONE',  ( -0.000000000000000000, -1.000000000000000000, -0.000000000000000000 ) ) ;
#71374 = CARTESIAN_POINT ( 'NONE',  ( -95.87840379837734872, -285.8814319001881472, -317.8351667553786228 ) ) ;
#71375 = CARTESIAN_POINT ( 'NONE',  ( 18.95080791339541548, -293.4106652269962865, -317.0917852779367649 ) ) ;
#71376 = CARTESIAN_POINT ( 'NONE',  ( 5.493655457592956814, -287.8371250870607696, -334.2238230474468992 ) ) ;
#71377 = CARTESIAN_POINT ( 'NONE',  ( -110.6122710711097739, -282.9280929730704202, -259.9017945200786812 ) ) ;
#71379 = CARTESIAN_POINT ( 'NONE',  ( -85.35925401383246935, -287.9658603153652621, -326.7518551005912855 ) ) ;
#71378 = CARTESIAN_POINT ( 'NONE',  ( -86.10311347677664173, -283.9353757169868118, -215.1776970751005820 ) ) ;
#71380 = CARTESIAN_POINT ( 'NONE',  ( 10.17738979605122829, -283.5850744603056341, -326.3660279873531636 ) ) ;
#71381 = CARTESIAN_POINT ( 'NONE',  ( -11.02489460564906487, -272.3948899110692423, -200.0746247869440708 ) ) ;
#71382 = AXIS2_PLACEMENT_3D ( 'NONE', #59011, #1701, #68806 ) ;
#71383 = CARTESIAN_POINT ( 'NONE',  ( -111.4459895149638413, -282.7270380410681696, -288.1645036816406105 ) ) ;
#71384 = CARTESIAN_POINT ( 'NONE',  ( -108.4414061454866243, -298.2436910454931080, -294.2322815991927882 ) ) ;
#71385 = CARTESIAN_POINT ( 'NONE',  ( -35.17493780986814755, -284.0791100049262923, -195.2128528951598980 ) ) ;
#71386 = AXIS2_PLACEMENT_3D ( 'NONE', #29476, #60214, #89053 ) ;
#71387 = CARTESIAN_POINT ( 'NONE',  ( -109.5159295249515452, -279.3291025618385675, -282.8564870290426825 ) ) ;
#71388 = CARTESIAN_POINT ( 'NONE',  ( 24.36169394290485712, -290.1344191215795263, -313.3774366260588522 ) ) ;
#71389 = CARTESIAN_POINT ( 'NONE',  ( 196.8088576720463436, 292.7107012191569311, -7.905027250450429754 ) ) ;
#71390 = CARTESIAN_POINT ( 'NONE',  ( 113.5000000000000568, -298.0521521680024080, -397.9547385950631337 ) ) ;
#71391 = CARTESIAN_POINT ( 'NONE',  ( 37.39589411695873622, -295.6139983819052759, -281.4789507191275106 ) ) ;
#71392 = AXIS2_PLACEMENT_3D ( 'NONE', #86748, #42730, #71645 ) ;
#71393 = CARTESIAN_POINT ( 'NONE',  ( -97.71778290525287503, -275.9448053321831367, -314.8768026644906399 ) ) ;
#71394 = CARTESIAN_POINT ( 'NONE',  ( -114.0905082423682160, -289.7027993248532312, -274.0731623080545774 ) ) ;
#71395 = CARTESIAN_POINT ( 'NONE',  ( 27.85536805538228222, -292.4192895141347890, -305.0503552548572657 ) ) ;
#71396 = CARTESIAN_POINT ( 'NONE',  ( -68.71874049333912637, -278.3156349909451706, -203.9026736917828373 ) ) ;
#71397 = CARTESIAN_POINT ( 'NONE',  ( -99.02293217888494326, -271.2011532360954220, -228.5949914414455861 ) ) ;
#71398 = CARTESIAN_POINT ( 'NONE',  ( -97.17252897901096276, -292.4606161553429047, -227.5957976191457988 ) ) ;
#71399 = CARTESIAN_POINT ( 'NONE',  ( 35.78497577281001440, -284.2662352645559167, -287.0191576251351080 ) ) ;
#71400 = CARTESIAN_POINT ( 'NONE',  ( -70.52403406787870210, -293.9615079234934569, -339.0896929176657864 ) ) ;
#71401 = CARTESIAN_POINT ( 'NONE',  ( -97.99490420138005220, -291.5725689488497778, -312.4264946828913025 ) ) ;
#71402 = CARTESIAN_POINT ( 'NONE',  ( 31.28061286755202985, -291.3667596246654625, -237.6051557016747608 ) ) ;
#71403 = CARTESIAN_POINT ( 'NONE',  ( -106.5808803370746745, -291.6481052360687158, -295.2872255897697187 ) ) ;
#71404 = EDGE_CURVE ( 'NONE', #29329, #24735, #30122, .T. ) ;
#71405 = FACE_BOUND ( 'NONE', #81663, .T. ) ;
#71406 = CARTESIAN_POINT ( 'NONE',  ( -108.8182862165075449, -291.1487983392687511, -286.0301920086504879 ) ) ;
#71407 = DIRECTION ( 'NONE',  ( 0.000000000000000000, 1.000000000000000000, 0.000000000000000000 ) ) ;
#71408 = CARTESIAN_POINT ( 'NONE',  ( -112.4755151888254119, -291.5686938336393155, -285.3579968711046035 ) ) ;
#71410 = CARTESIAN_POINT ( 'NONE',  ( -1.256675880218204533, -292.5451282510546207, -206.8890109921680676 ) ) ;
#71409 = CARTESIAN_POINT ( 'NONE',  ( 37.99729989076480763, -279.5312607891003154, -267.1530959016654947 ) ) ;
#71411 = CARTESIAN_POINT ( 'NONE',  ( 32.02146675891162886, -281.1218690377303346, -236.8056672198304113 ) ) ;
#71412 = CARTESIAN_POINT ( 'NONE',  ( 32.37143901423192460, -281.6384311189004848, -303.1336246565859369 ) ) ;
#71413 = CARTESIAN_POINT ( 'NONE',  ( -3.674546666726771882, -284.4963017798824580, -203.3422890575180020 ) ) ;
#71414 = CARTESIAN_POINT ( 'NONE',  ( -0.6619558416067039541, -280.6988714198547541, -334.9015071981390292 ) ) ;
#71415 = CARTESIAN_POINT ( 'NONE',  ( -32.41176746138095410, -284.1141308810636588, -195.5104930882962719 ) ) ;
#71416 = CARTESIAN_POINT ( 'NONE',  ( 23.20906207924225484, -279.4067851733914267, -223.9036488897866093 ) ) ;
#71417 = CARTESIAN_POINT ( 'NONE',  ( 7.374898859765222525, -285.5660353292421973, -207.9906607808457295 ) ) ;
#71418 = CARTESIAN_POINT ( 'NONE',  ( 5.262497132025202085, -275.4476596105712360, -210.8217563982392164 ) ) ;
#71419 = DIRECTION ( 'NONE',  ( 0.000000000000000000, 0.000000000000000000, 1.000000000000000000 ) ) ;
#71420 = CARTESIAN_POINT ( 'NONE',  ( -52.55436324774615997, -293.4543107966954949, -198.0935823730684433 ) ) ;
#71421 = CARTESIAN_POINT ( 'NONE',  ( 29.42378339552801592, -276.4907415538869486, -233.0908697664995657 ) ) ;
#71422 = CARTESIAN_POINT ( 'NONE',  ( -108.5078298940611177, -278.0024587740880975, -286.7710388224467124 ) ) ;
#71423 = CARTESIAN_POINT ( 'NONE',  ( -114.3901020438053848, -290.7079543581995722, -271.2308759439659980 ) ) ;
#71424 = CARTESIAN_POINT ( 'NONE',  ( 37.75452565523089277, -279.5196107165972421, -261.5427661957741634 ) ) ;
#71425 = CARTESIAN_POINT ( 'NONE',  ( -56.18673276623513857, -291.6493345696363804, -195.6478503356330236 ) ) ;
#71426 = CARTESIAN_POINT ( 'NONE',  ( -36.19044573032927303, -291.1256462782791345, -197.1223557603116774 ) ) ;
#71427 = CARTESIAN_POINT ( 'NONE',  ( 24.06218792717892541, -292.1369262873832895, -313.4481604880837722 ) ) ;
#71428 = VERTEX_POINT ( 'NONE', #64777 ) ;
#71429 = DIRECTION ( 'NONE',  ( 0.7957555401921969640, 0.6056179655966498210, 0.000000000000000000 ) ) ;
#71430 = CARTESIAN_POINT ( 'NONE',  ( 8.892626217268210453, -292.2136587735435000, -213.7236311021974586 ) ) ;
#71431 = CARTESIAN_POINT ( 'NONE',  ( -113.5000000000000568, -211.8141737103562434, -518.0411269958476623 ) ) ;
#71432 = CARTESIAN_POINT ( 'NONE',  ( -6.998514795304330072, -274.1237833571632905, -333.4427485647536855 ) ) ;
#71433 = CARTESIAN_POINT ( 'NONE',  ( -101.4384328853939650, -295.0526783255725718, -312.6997769162933309 ) ) ;
#71434 = CARTESIAN_POINT ( 'NONE',  ( -110.4597285074341926, -286.1539619006878183, -247.6648574772274287 ) ) ;
#71435 = CARTESIAN_POINT ( 'NONE',  ( -25.13973092812124932, -286.0452636887555400, -198.3368251598397478 ) ) ;
#71436 = CARTESIAN_POINT ( 'NONE',  ( 35.70523211131943242, -276.9450112145505045, -260.6218447678022017 ) ) ;
#71437 = CARTESIAN_POINT ( 'NONE',  ( -4.847791930983072817, -292.6422410391843414, -337.5763733692938899 ) ) ;
#71438 = CARTESIAN_POINT ( 'NONE',  ( -87.15567503646454384, -297.5178172236590513, -325.1017967811174003 ) ) ;
#71439 = CARTESIAN_POINT ( 'NONE',  ( 31.62965106325087206, -274.6814783460080776, -295.6101805169362251 ) ) ;
#71440 = ORIENTED_EDGE ( 'NONE', *, *, #8954, .T. ) ;
#71441 = CARTESIAN_POINT ( 'NONE',  ( 194.2991910711363346, 39.77461757278994980, 14.57244569840369053 ) ) ;
#71442 = CARTESIAN_POINT ( 'NONE',  ( -114.3167787017339663, -296.2284117409971032, -269.5985106030441329 ) ) ;
#71443 = CARTESIAN_POINT ( 'NONE',  ( 34.47759765648295627, -289.7281851577434395, -290.1307548240131950 ) ) ;
#71444 = CARTESIAN_POINT ( 'NONE',  ( -60.24766513392076206, -295.7551677297219612, -198.8907321425861312 ) ) ;
#71445 = CARTESIAN_POINT ( 'NONE',  ( -5.740868647919679546, -289.2766615644503077, -336.2798567322572580 ) ) ;
#71446 = VERTEX_POINT ( 'NONE', #42960 ) ;
#71447 = CARTESIAN_POINT ( 'NONE',  ( -90.88543552336295761, -278.3737213555781977, -215.2789469846213990 ) ) ;
#71448 = CARTESIAN_POINT ( 'NONE',  ( -3.266480344012961723, -295.2654424718415385, -339.3118489323050539 ) ) ;
#71449 = CARTESIAN_POINT ( 'NONE',  ( -90.74498107853588635, -287.9387880582918342, -324.1787346852301539 ) ) ;
#71450 = CARTESIAN_POINT ( 'NONE',  ( -79.46184656144620817, -295.9376861448615159, -334.7943202613432163 ) ) ;
#71452 = CARTESIAN_POINT ( 'NONE',  ( 31.56141735094734813, -294.2087905507810888, -294.6879012307194330 ) ) ;
#71451 = CIRCLE ( 'NONE', #54789, 4.999999999999990230 ) ;
#71453 = CARTESIAN_POINT ( 'NONE',  ( 199.6702811234769683, 65.52214591209386185, -9.100946541886337116 ) ) ;
#71454 = CIRCLE ( 'NONE', #91058, 4.000000000000003553 ) ;
#71455 = FACE_OUTER_BOUND ( 'NONE', #39136, .T. ) ;
#71456 = CARTESIAN_POINT ( 'NONE',  ( 201.2104617360081704, 41.21457449016152452, 9.000000000000000000 ) ) ;
#71457 = CARTESIAN_POINT ( 'NONE',  ( -3.352018646887067632, -290.1317181207722911, -338.6940567775878321 ) ) ;
#71458 = CARTESIAN_POINT ( 'NONE',  ( -37.37352853689063181, -282.5519495502701375, -190.3611179825600175 ) ) ;
#71459 = VERTEX_POINT ( 'NONE', #49133 ) ;
#71460 = ADVANCED_FACE ( 'NONE', ( #78029 ), #29224, .T. ) ;
#71461 = VECTOR ( 'NONE', #2674, 1000.000000000000000 ) ;
#71462 = CARTESIAN_POINT ( 'NONE',  ( -31.07378316378691352, -279.4778324171464305, -193.6663023847335126 ) ) ;
#71463 = CARTESIAN_POINT ( 'NONE',  ( -36.13915126887679463, -285.0371959840802560, -345.1847927563771350 ) ) ;
#71464 = ADVANCED_FACE ( 'NONE', ( #64320 ), #42005, .T. ) ;
#71465 = CARTESIAN_POINT ( 'NONE',  ( 30.90374222105522506, -285.6812455088237925, -235.9930239145242012 ) ) ;
#71467 = CARTESIAN_POINT ( 'NONE',  ( -48.29659045905209780, -287.2723401326873045, -344.0426568705645991 ) ) ;
#71466 = CIRCLE ( 'NONE', #69960, 10.55076157886938937 ) ;
#71468 = CARTESIAN_POINT ( 'NONE',  ( -5.777417045875322010, -278.5019492286043032, -339.2378304280849761 ) ) ;
#71469 = EDGE_LOOP ( 'NONE', ( #31280, #77584, #63229, #72869 ) ) ;
#71471 = CARTESIAN_POINT ( 'NONE',  ( -96.48329329864841952, -278.5012371238213973, -227.3941001007837031 ) ) ;
#71470 = CARTESIAN_POINT ( 'NONE',  ( -109.9661095660103030, -278.6561037714956228, -262.4810183594653950 ) ) ;
#71472 = CARTESIAN_POINT ( 'NONE',  ( 35.43225300282824719, -276.3241071104941398, -245.9978551397829563 ) ) ;
#71473 = CARTESIAN_POINT ( 'NONE',  ( -96.50093552310204359, -278.0043876351865038, -221.6766356938893523 ) ) ;
#71474 = CARTESIAN_POINT ( 'NONE',  ( 23.85752577023820820, -22.80717641334416257, -342.6356047177218329 ) ) ;
#71475 = CARTESIAN_POINT ( 'NONE',  ( -27.03999952409519025, -275.1211835814887081, -194.2375214088650068 ) ) ;
#71476 = CARTESIAN_POINT ( 'NONE',  ( -82.63601058452800885, -298.8723409525148895, -208.7565020164376506 ) ) ;
#71477 = CARTESIAN_POINT ( 'NONE',  ( 21.27581636871892101, -283.4090924074130839, -223.5744983911110353 ) ) ;
#71478 = CARTESIAN_POINT ( 'NONE',  ( 82.66537480607564703, -298.2604009065653372, -193.2156244055160528 ) ) ;
#71479 = CARTESIAN_POINT ( 'NONE',  ( -9.388194383048595881, -287.5059696358736119, -202.5771506798083124 ) ) ;
#71480 = CARTESIAN_POINT ( 'NONE',  ( -0.2309437621850514710, -288.2987939397200989, -204.0381579992571517 ) ) ;
#71481 = CARTESIAN_POINT ( 'NONE',  ( 24.31988302674011493, -287.4428948066425278, -309.6261384327821133 ) ) ;
#71482 = CARTESIAN_POINT ( 'NONE',  ( -69.16672939997172875, -282.9673061595082117, -340.4233221233238282 ) ) ;
#71483 = CARTESIAN_POINT ( 'NONE',  ( 5.402910941885852303, -279.0414961008050909, -210.2001785130106271 ) ) ;
#71484 = CARTESIAN_POINT ( 'NONE',  ( -63.01186688303901917, -287.5748632987310316, -200.6506517138367087 ) ) ;
#71485 = CARTESIAN_POINT ( 'NONE',  ( 35.01869465258602787, -279.8488280918078317, -256.3417356413095831 ) ) ;
#71486 = CARTESIAN_POINT ( 'NONE',  ( -56.71414489996688246, -278.6222334833291825, -341.3079147806263904 ) ) ;
#71487 = AXIS2_PLACEMENT_3D ( 'NONE', #77139, #76670, #40188 ) ;
#71488 = CARTESIAN_POINT ( 'NONE',  ( 32.15865163379631753, -276.3431858935818468, -292.8930851989941289 ) ) ;
#71489 = CARTESIAN_POINT ( 'NONE',  ( -62.64703933424094373, -288.1690947169889796, -342.7196952740434881 ) ) ;
#71490 = CARTESIAN_POINT ( 'NONE',  ( -31.63805241721790651, -283.7847380058757381, -347.0009019828759165 ) ) ;
#71491 = CARTESIAN_POINT ( 'NONE',  ( -112.9389728075479411, -285.2269463557754534, -255.7806732370833629 ) ) ;
#71492 = CARTESIAN_POINT ( 'NONE',  ( 22.11225966026825063, -281.1271147412086293, -228.0028051030079439 ) ) ;
#71493 = ORIENTED_EDGE ( 'NONE', *, *, #52972, .F. ) ;
#71494 = ORIENTED_EDGE ( 'NONE', *, *, #66418, .T. ) ;
#71495 = DIRECTION ( 'NONE',  ( 0.000000000000000000, -0.2502735790305593566, -0.9681751575201846816 ) ) ;
#71496 = CARTESIAN_POINT ( 'NONE',  ( 7.227348878636523644, -290.3128700102743096, -331.6949505549666242 ) ) ;
#71497 = CARTESIAN_POINT ( 'NONE',  ( -102.7852670100547243, -289.7587127178177298, -230.6302618005856289 ) ) ;
#71498 = CARTESIAN_POINT ( 'NONE',  ( -91.28777028412206107, -272.3196671839227179, -220.8124662025029750 ) ) ;
#71499 = CARTESIAN_POINT ( 'NONE',  ( 36.19193832824478108, -292.6178860356962446, -247.8640781329650622 ) ) ;
#71500 = CARTESIAN_POINT ( 'NONE',  ( -98.69857132884716577, -288.4705046532625374, -311.2012787157181606 ) ) ;
#71501 = CARTESIAN_POINT ( 'NONE',  ( 25.72289322775306175, -291.2641713841838396, -231.5232156683388496 ) ) ;
#71502 = CARTESIAN_POINT ( 'NONE',  ( 25.28156110685261027, -288.2326344144817654, -232.0798215491795702 ) ) ;
#71503 = CARTESIAN_POINT ( 'NONE',  ( -110.4683760289727132, -299.2662352645559167, -253.7030783399848985 ) ) ;
#71504 = CARTESIAN_POINT ( 'NONE',  ( -7.686658965846624447, -290.6636682903838391, -339.2631550685158004 ) ) ;
#71505 = CARTESIAN_POINT ( 'NONE',  ( -41.91631914476990062, -289.9944572527207924, -195.3337810406539745 ) ) ;
#71506 = CARTESIAN_POINT ( 'NONE',  ( -61.74178741097976797, -293.7353735401338781, -199.3869965513158888 ) ) ;
#71507 = CARTESIAN_POINT ( 'NONE',  ( -106.7591720747768562, -285.8042952867276654, -246.8650875239355287 ) ) ;
#71508 = CARTESIAN_POINT ( 'NONE',  ( 9.945200732662325294, -294.7015614782469584, -211.8649197382757450 ) ) ;
#71509 = CARTESIAN_POINT ( 'NONE',  ( 199.8839601301601476, 66.89258700487513920, -4.790067391029595001 ) ) ;
#71510 = DIRECTION ( 'NONE',  ( 0.000000000000000000, 1.000000000000000000, 0.000000000000000000 ) ) ;
#71511 = CARTESIAN_POINT ( 'NONE',  ( 29.18144493974218534, -300.7989061242936941, -194.7795398347321054 ) ) ;
#71512 = CARTESIAN_POINT ( 'NONE',  ( -10.92698970840942252, -281.8960514269948590, -338.6413830139247239 ) ) ;
#71513 = CARTESIAN_POINT ( 'NONE',  ( 2.132885978195367294, -280.5238692337476323, -334.1928853213923958 ) ) ;
#71514 = CARTESIAN_POINT ( 'NONE',  ( -74.53717673322763915, -294.7307916537503729, -337.6565279610424568 ) ) ;
#71515 = CARTESIAN_POINT ( 'NONE',  ( 35.62843806190176821, -273.6299134049132249, -257.9029404304777700 ) ) ;
#71516 = CARTESIAN_POINT ( 'NONE',  ( -110.4622936750242133, -276.4506186313086005, -284.3818257799994740 ) ) ;
#71517 = CARTESIAN_POINT ( 'NONE',  ( -110.7332702738969061, -297.8167188634415652, -274.2238771431095188 ) ) ;
#71518 = CARTESIAN_POINT ( 'NONE',  ( 28.00810587870184776, -273.6048782726140871, -230.6618338102382495 ) ) ;
#71519 = CARTESIAN_POINT ( 'NONE',  ( -61.18707176432186401, -296.7930531231925784, -340.0338901139157315 ) ) ;
#71520 = DIRECTION ( 'NONE',  ( 0.000000000000000000, -1.000000000000000000, -0.000000000000000000 ) ) ;
#71521 = CARTESIAN_POINT ( 'NONE',  ( -107.6173160520399676, -297.6234925251642949, -250.0156139653211369 ) ) ;
#71522 = DIRECTION ( 'NONE',  ( 0.000000000000000000, 0.000000000000000000, -1.000000000000000000 ) ) ;
#71523 = AXIS2_PLACEMENT_3D ( 'NONE', #80793, #74624, #9753 ) ;
#71525 = CARTESIAN_POINT ( 'NONE',  ( -92.91240329542510779, -273.0589856134864704, -223.0037098112670719 ) ) ;
#71524 = CARTESIAN_POINT ( 'NONE',  ( -1.724244142619061115, -284.5418719285844986, -203.9547656202849168 ) ) ;
#71526 = VECTOR ( 'NONE', #13143, 1000.000000000000000 ) ;
#71527 = CARTESIAN_POINT ( 'NONE',  ( -52.17328396290285752, -285.8674519637603453, -194.7486434589253292 ) ) ;
#71528 = CARTESIAN_POINT ( 'NONE',  ( 38.53674002151437605, -287.0556566207039850, -257.3140983458358733 ) ) ;
#71529 = CARTESIAN_POINT ( 'NONE',  ( -111.5789622549427378, -298.3630191131977085, -283.5873883096529084 ) ) ;
#71530 = CARTESIAN_POINT ( 'NONE',  ( 27.84374650239059079, -291.0600120212583874, -233.5008489501639701 ) ) ;
#71531 = AXIS2_PLACEMENT_3D ( 'NONE', #50785, #6304, #21433 ) ;
#71532 = CARTESIAN_POINT ( 'NONE',  ( -95.77633964652434884, -278.4239383879316279, -220.4455044279671938 ) ) ;
#71533 = CARTESIAN_POINT ( 'NONE',  ( 35.78497577281001440, -290.8380690714490129, -253.7030783399848985 ) ) ;
#71534 = CIRCLE ( 'NONE', #27723, 24.00000000000000711 ) ;
#71535 = FACE_OUTER_BOUND ( 'NONE', #71329, .T. ) ;
#71536 = CARTESIAN_POINT ( 'NONE',  ( -9.327709826978388463, -285.2215914868312439, -202.5069363119493460 ) ) ;
#71537 = CARTESIAN_POINT ( 'NONE',  ( 197.8646367605500700, 70.82932363588079738, -10.83694520234208269 ) ) ;
#71538 = CARTESIAN_POINT ( 'NONE',  ( -70.88934232706381522, -287.4945361432881441, -337.4540922527011730 ) ) ;
#71539 = CARTESIAN_POINT ( 'NONE',  ( -73.25380238804000044, -299.1675905631590808, -205.8881676291425435 ) ) ;
#71540 = CARTESIAN_POINT ( 'NONE',  ( -73.50293477378076545, -281.0072955818818627, -203.0337893677006491 ) ) ;
#71542 = CARTESIAN_POINT ( 'NONE',  ( 25.55902995322113824, -282.0622058932659115, -307.5082476223877848 ) ) ;
#71541 = CARTESIAN_POINT ( 'NONE',  ( -102.4164048850196451, -295.0786669671501272, -232.2624267701394558 ) ) ;
#71543 = CARTESIAN_POINT ( 'NONE',  ( -96.51005562779111813, -296.0558366839032942, -319.6574316830411249 ) ) ;
#71544 = CARTESIAN_POINT ( 'NONE',  ( -50.09273146737339033, -299.4066023248960278, -197.7793093073375132 ) ) ;
#71545 = CARTESIAN_POINT ( 'NONE',  ( 26.14445379624881483, -283.0143621068036168, -230.3325390352854072 ) ) ;
#71546 = CARTESIAN_POINT ( 'NONE',  ( -77.63145088307130948, -296.5557275530918560, -209.1434650964831690 ) ) ;
#71547 = DIRECTION ( 'NONE',  ( 0.000000000000000000, 1.000000000000000000, 0.000000000000000000 ) ) ;
#71548 = CARTESIAN_POINT ( 'NONE',  ( -74.59631179145532087, -285.5299055823111871, -335.1033982902816319 ) ) ;
#71549 = CARTESIAN_POINT ( 'NONE',  ( -74.94434090351494149, -212.1443419142231051, 25.50000000000000000 ) ) ;
#71550 = CARTESIAN_POINT ( 'NONE',  ( 10.64812456238590777, -290.1952119285920162, -210.2361428286349110 ) ) ;
#71551 = CARTESIAN_POINT ( 'NONE',  ( 36.43371240826417079, -274.4772896611304418, -248.6960973273557727 ) ) ;
#71552 = CARTESIAN_POINT ( 'NONE',  ( 28.73942239600594917, -292.9650167402072611, -239.2210865081845270 ) ) ;
#71553 = CIRCLE ( 'NONE', #71487, 7.500000000000012434 ) ;
#71554 = CARTESIAN_POINT ( 'NONE',  ( 34.43129487909363462, -282.8538656425229760, -253.6475025022920136 ) ) ;
#71555 = CARTESIAN_POINT ( 'NONE',  ( 36.38501525290016048, -277.0963258548464978, -266.0723892975736362 ) ) ;
#71556 = AXIS2_PLACEMENT_3D ( 'NONE', #70612, #77229, #32741 ) ;
#71557 = CARTESIAN_POINT ( 'NONE',  ( -112.5536940831012060, -285.8038529190048962, -284.1331751001197290 ) ) ;
#71558 = CARTESIAN_POINT ( 'NONE',  ( 19.15150624436531857, -279.6859568984608018, -223.4838627648655347 ) ) ;
#71559 = CARTESIAN_POINT ( 'NONE',  ( -88.44004290149497649, -279.7686299967593868, -325.2606627201456035 ) ) ;
#71560 = CARTESIAN_POINT ( 'NONE',  ( -40.44025748586465596, -298.0143435127642420, -193.3713612973597264 ) ) ;
#71561 = CARTESIAN_POINT ( 'NONE',  ( 18.90176012560037222, -276.1027469310284346, -322.9507860096531999 ) ) ;
#71562 = CARTESIAN_POINT ( 'NONE',  ( 19.95686336691050400, -296.1332113089037534, -317.8815222580238924 ) ) ;
#71563 = DIRECTION ( 'NONE',  ( -0.000000000000000000, 1.000000000000000000, -0.000000000000000000 ) ) ;
#71564 = CYLINDRICAL_SURFACE ( 'NONE', #69344, 0.5000000000000004441 ) ;
#71565 = CARTESIAN_POINT ( 'NONE',  ( -96.45877731531432175, -294.0463051459646522, -317.7681185191204349 ) ) ;
#71566 = CARTESIAN_POINT ( 'NONE',  ( -67.07681387855500077, -273.1591948399645844, -203.6105318771257373 ) ) ;
#71567 = CARTESIAN_POINT ( 'NONE',  ( -19.43106419327913770, -296.3460742766268936, -344.5904198241545942 ) ) ;
#71568 = CARTESIAN_POINT ( 'NONE',  ( 24.57444020611981017, -295.3591906175447548, -315.4875457036288822 ) ) ;
#71569 = EDGE_CURVE ( 'NONE', #28384, #33195, #63838, .T. ) ;
#71570 = CARTESIAN_POINT ( 'NONE',  ( -45.53858600060075190, -291.1564417866723034, -344.7441771258927474 ) ) ;
#71571 = CARTESIAN_POINT ( 'NONE',  ( -48.91591296558655699, -275.1996230803521257, -344.3466481428027350 ) ) ;
#71572 = CARTESIAN_POINT ( 'NONE',  ( -100.3818052584677218, -279.9350375895110119, -310.0459813418519275 ) ) ;
#71573 = CARTESIAN_POINT ( 'NONE',  ( -107.3496476419772279, -294.2996964159375466, -295.8150277207770387 ) ) ;
#71574 = CARTESIAN_POINT ( 'NONE',  ( 23.58412914423543683, -282.8042388404967369, -225.3239243514343002 ) ) ;
#71575 = CARTESIAN_POINT ( 'NONE',  ( -67.66305006227771912, -284.5649735396472693, -203.6165166077861670 ) ) ;
#71576 = CARTESIAN_POINT ( 'NONE',  ( 66.80823473016013736, 46.34870276661032307, -317.8007354683743415 ) ) ;
#71577 = VERTEX_POINT ( 'NONE', #49593 ) ;
#71578 = CARTESIAN_POINT ( 'NONE',  ( -108.4468605238712087, -283.9990651714399519, -287.0333342115465030 ) ) ;
#71579 = CARTESIAN_POINT ( 'NONE',  ( 12.77972700939818651, -281.8122921188626719, -212.3151443872760638 ) ) ;
#71580 = CARTESIAN_POINT ( 'NONE',  ( -113.0924092642269727, -283.4947163427395367, -258.6171165374078669 ) ) ;
#71581 = CARTESIAN_POINT ( 'NONE',  ( -113.8435366932767465, -279.4060835758023131, -277.3217065339483725 ) ) ;
#71582 = CARTESIAN_POINT ( 'NONE',  ( -51.16782384255493099, -278.7459310332778841, -345.4047456536860636 ) ) ;
#71583 = CARTESIAN_POINT ( 'NONE',  ( 17.40634833298267736, -296.6948066931273047, -313.9805196606274080 ) ) ;
#71584 = CARTESIAN_POINT ( 'NONE',  ( -111.5685550221716511, -271.9231168036148460, -296.3965291073083108 ) ) ;
#71585 = ORIENTED_EDGE ( 'NONE', *, *, #33448, .T. ) ;
#71586 = AXIS2_PLACEMENT_3D ( 'NONE', #48414, #61715, #25707 ) ;
#71587 = CARTESIAN_POINT ( 'NONE',  ( -70.15493457438154223, -299.6199537748950092, -202.9200896783225403 ) ) ;
#71588 = CARTESIAN_POINT ( 'NONE',  ( -90.63052692306658287, -277.3129362275749941, -218.0179421694803352 ) ) ;
#71589 = CARTESIAN_POINT ( 'NONE',  ( -113.3557315856648557, -292.3371030186479516, -268.4034833780483496 ) ) ;
#71590 = CARTESIAN_POINT ( 'NONE',  ( 33.40894805935678136, -292.6582720755254172, -251.9698578426984739 ) ) ;
#71591 = CARTESIAN_POINT ( 'NONE',  ( -113.0738433005874413, -289.8890167207642889, -284.0064690308841477 ) ) ;
#71592 = DIRECTION ( 'NONE',  ( 0.000000000000000000, 1.000000000000000000, 0.000000000000000000 ) ) ;
#71594 = CARTESIAN_POINT ( 'NONE',  ( -62.82014232609035531, -284.1148769530660161, -201.0441579418894946 ) ) ;
#71593 = CARTESIAN_POINT ( 'NONE',  ( 36.52228909893809572, -292.3736914102457263, -289.9242820855620266 ) ) ;
#71595 = CARTESIAN_POINT ( 'NONE',  ( -1.869711445374419467, -294.3876342644962278, -205.1346956712587541 ) ) ;
#71596 = CARTESIAN_POINT ( 'NONE',  ( -33.18032793264231373, -284.5852370881650018, -196.7350771420746298 ) ) ;
#71597 = CARTESIAN_POINT ( 'NONE',  ( -18.59377739586923894, -284.1209001642205862, -341.4755350446364446 ) ) ;
#71598 = EDGE_LOOP ( 'NONE', ( #84491, #7730, #39263, #82832 ) ) ;
#71599 = CARTESIAN_POINT ( 'NONE',  ( -56.14279642456811814, -292.7570883067071463, -195.8795997177077481 ) ) ;
#71600 = TOROIDAL_SURFACE ( 'NONE', #79095, 8.222204860432958284, 1.000000000000000000 ) ;
#71601 = CARTESIAN_POINT ( 'NONE',  ( -38.36100793374497187, -280.5313865153265169, -197.2942786715137800 ) ) ;
#71602 = CARTESIAN_POINT ( 'NONE',  ( -11.20717829123565501, -293.5140747523427081, -342.4243038314843943 ) ) ;
#71603 = CARTESIAN_POINT ( 'NONE',  ( -8.284700953983888283, -289.4840776078157205, -341.5079751470012184 ) ) ;
#71604 = CARTESIAN_POINT ( 'NONE',  ( -96.33982805634261126, -290.3791504547903628, -319.7652302058426130 ) ) ;
#71605 = CARTESIAN_POINT ( 'NONE',  ( 15.02801775151314168, -286.9835232321754006, -219.5043322631170781 ) ) ;
#71606 = ORIENTED_EDGE ( 'NONE', *, *, #34585, .F. ) ;
#71607 = CARTESIAN_POINT ( 'NONE',  ( 195.5480150185777291, 26.67257684198393974, 13.83492282920820493 ) ) ;
#71608 = CARTESIAN_POINT ( 'NONE',  ( -34.87080899689524216, -296.8818312747065420, -346.0856198296137904 ) ) ;
#71609 = AXIS2_PLACEMENT_3D ( 'NONE', #91391, #11397, #91858 ) ;
#71610 = CARTESIAN_POINT ( 'NONE',  ( -108.4241622780869676, -295.5998369217901995, -241.9242758961994184 ) ) ;
#71611 = CARTESIAN_POINT ( 'NONE',  ( -109.8530493278866800, -277.7505861745600555, -259.7377054285277040 ) ) ;
#71612 = CARTESIAN_POINT ( 'NONE',  ( -46.86716050204879735, -273.4419225846557993, -194.0145888683066175 ) ) ;
#71613 = CARTESIAN_POINT ( 'NONE',  ( -72.47198465341396911, -294.0058772578710204, -335.1564694544476311 ) ) ;
#71614 = CARTESIAN_POINT ( 'NONE',  ( 10.11792469851334708, -276.4766671076706075, -213.5000237227767741 ) ) ;
#71615 = CARTESIAN_POINT ( 'NONE',  ( -97.26463535932182936, -271.2961678713374454, -226.4567184861905673 ) ) ;
#71616 = CARTESIAN_POINT ( 'NONE',  ( 33.68862166955093329, -294.5144608013111451, -251.8726380246564815 ) ) ;
#71617 = CARTESIAN_POINT ( 'NONE',  ( -96.65043022234222292, -297.0310624997503623, -313.4719879698985210 ) ) ;
#71618 = FACE_BOUND ( 'NONE', #45508, .T. ) ;
#71619 = CIRCLE ( 'NONE', #76119, 4.999999999999976907 ) ;
#71620 = CARTESIAN_POINT ( 'NONE',  ( -110.4843634630860549, -294.7739764931605464, -253.0354367145798449 ) ) ;
#71621 = CARTESIAN_POINT ( 'NONE',  ( -37.61563500620392375, -298.7002158081417633, -193.4635383920897880 ) ) ;
#71622 = CARTESIAN_POINT ( 'NONE',  ( -70.25215340441238254, -288.0693311842300091, -336.1951258724580498 ) ) ;
#71623 = CARTESIAN_POINT ( 'NONE',  ( -112.3417001281295029, -274.5519907608264134, -270.3865269787834222 ) ) ;
#71624 = CARTESIAN_POINT ( 'NONE',  ( -67.51728771384556183, -274.1591084404207095, -199.5871056813758457 ) ) ;
#71625 = CARTESIAN_POINT ( 'NONE',  ( -103.9541643660616757, -296.4811144576833044, -300.3990324955398137 ) ) ;
#71626 = CARTESIAN_POINT ( 'NONE',  ( -107.0019747050131826, -280.9052485870719238, -241.6234606999778407 ) ) ;
#71627 = CARTESIAN_POINT ( 'NONE',  ( 35.13647504956216494, -280.5494270097165668, -295.0248807746287412 ) ) ;
#71628 = AXIS2_PLACEMENT_3D ( 'NONE', #55813, #11317, #90358 ) ;
#71629 = CARTESIAN_POINT ( 'NONE',  ( -81.50980137050387953, -282.9840380006575060, -333.3742277718313858 ) ) ;
#71630 = CARTESIAN_POINT ( 'NONE',  ( 38.62820432524579672, -274.7505092193504765, -258.3645751439145783 ) ) ;
#71631 = CARTESIAN_POINT ( 'NONE',  ( -5.262046132045552049, -278.8671928222951237, -201.2428409666093216 ) ) ;
#71632 = CARTESIAN_POINT ( 'NONE',  ( -17.45199622606810763, -278.3080528031024983, -197.8736838824151789 ) ) ;
#71633 = CARTESIAN_POINT ( 'NONE',  ( -105.9591363085006464, -271.4810009299662283, -243.6307527733444829 ) ) ;
#71634 = CARTESIAN_POINT ( 'NONE',  ( 33.41221441907261180, -277.2283432157170182, -245.3296959945814990 ) ) ;
#71635 = CARTESIAN_POINT ( 'NONE',  ( 153.6948129392865781, 20.34864080145124987, 12.70029817130066441 ) ) ;
#71636 = CARTESIAN_POINT ( 'NONE',  ( 28.06086145274387178, -291.0753804406915606, -232.9323624706967450 ) ) ;
#71637 = CARTESIAN_POINT ( 'NONE',  ( -58.93868409273427744, -291.7802225772009024, -196.4519150127638341 ) ) ;
#71638 = CARTESIAN_POINT ( 'NONE',  ( 15.68050772243511481, -278.3045312274953744, -323.7130314501222301 ) ) ;
#71639 = CARTESIAN_POINT ( 'NONE',  ( 0.4838307566632938372, -272.5559825923679682, -205.5832506019904997 ) ) ;
#71640 = DIRECTION ( 'NONE',  ( 0.000000000000000000, 0.000000000000000000, 1.000000000000000000 ) ) ;
#71641 = CARTESIAN_POINT ( 'NONE',  ( -92.72255597985856923, -283.2586749062211311, -219.7101000446822070 ) ) ;
#71642 = LINE ( 'NONE', #71172, #1348 ) ;
#71643 = CARTESIAN_POINT ( 'NONE',  ( 19.99438012179129487, -292.9910809704343819, -316.2036794160327986 ) ) ;
#71644 = CARTESIAN_POINT ( 'NONE',  ( 35.97547383269628085, -285.8437597006701480, -282.0805864867554078 ) ) ;
#71645 = DIRECTION ( 'NONE',  ( -0.9953184226294286008, 0.000000000000000000, 0.09665007798479169354 ) ) ;
#71646 = DIRECTION ( 'NONE',  ( -0.000000000000000000, 0.000000000000000000, -1.000000000000000000 ) ) ;
#71647 = CARTESIAN_POINT ( 'NONE',  ( -85.78893436411632933, -293.7223037626031896, -327.6819781360918569 ) ) ;
#71648 = CARTESIAN_POINT ( 'NONE',  ( -83.47952874564877845, -282.1513635884786595, -331.2058617852938482 ) ) ;
#71649 = CARTESIAN_POINT ( 'NONE',  ( -107.9988771690913865, -280.4313223872106846, -249.0537542717651149 ) ) ;
#71650 = CARTESIAN_POINT ( 'NONE',  ( -113.2039295395671559, -285.6189284043271073, -281.3621415188760011 ) ) ;
#71651 = CARTESIAN_POINT ( 'NONE',  ( -17.23822585400530727, -278.5480334327500600, -197.0820327427349241 ) ) ;
#71652 = CARTESIAN_POINT ( 'NONE',  ( 11.13405799563638432, -286.7454904218800493, -215.7120609333748575 ) ) ;
#71653 = AXIS2_PLACEMENT_3D ( 'NONE', #5942, #86384, #71758 ) ;
#71654 = CARTESIAN_POINT ( 'NONE',  ( -32.36270670230294400, -278.4135632189978651, -343.8320874678398127 ) ) ;
#71655 = CARTESIAN_POINT ( 'NONE',  ( -108.1314139690347105, -279.5989871059999246, -251.8343779645686595 ) ) ;
#71656 = CARTESIAN_POINT ( 'NONE',  ( -103.9893939049711946, -286.9972294998182747, -235.0855380251324789 ) ) ;
#71657 = ORIENTED_EDGE ( 'NONE', *, *, #13861, .T. ) ;
#71658 = AXIS2_PLACEMENT_3D ( 'NONE', #25461, #54805, #82751 ) ;
#71659 = CARTESIAN_POINT ( 'NONE',  ( -80.62326767628746893, -297.3164989121188455, -206.6125872719093763 ) ) ;
#71660 = CARTESIAN_POINT ( 'NONE',  ( -5.058756500323404737, -290.6049254231585905, -337.6638546134918215 ) ) ;
#71661 = LINE ( 'NONE', #57907, #77552 ) ;
#71662 = CARTESIAN_POINT ( 'NONE',  ( -115.3430155898818299, -281.2662352645559167, -252.5904736702033517 ) ) ;
#71663 = ORIENTED_EDGE ( 'NONE', *, *, #85914, .F. ) ;
#71664 = CARTESIAN_POINT ( 'NONE',  ( -64.22014028701661914, -271.7021451115908235, -200.1505636657080913 ) ) ;
#71665 = CARTESIAN_POINT ( 'NONE',  ( 14.90463326366642782, -291.1734704565086531, -214.8200912840153478 ) ) ;
#71666 = CARTESIAN_POINT ( 'NONE',  ( -69.75700534964708766, -294.9986136034382866, -335.8381095846580706 ) ) ;
#71667 = AXIS2_PLACEMENT_3D ( 'NONE', #86391, #34360, #56138 ) ;
#71668 = CARTESIAN_POINT ( 'NONE',  ( 32.49149305582440661, -288.7625260792373751, -246.8232148925967806 ) ) ;
#71669 = CARTESIAN_POINT ( 'NONE',  ( 20.45344296845333076, -282.6679971410620738, -224.1258992502960155 ) ) ;
#71670 = CARTESIAN_POINT ( 'NONE',  ( -109.3044470916250646, -291.6488725461564968, -296.2077444525777423 ) ) ;
#71671 = CARTESIAN_POINT ( 'NONE',  ( -107.2737544383766419, -291.4673105193938341, -301.5204688082704365 ) ) ;
#71672 = CARTESIAN_POINT ( 'NONE',  ( -110.0253345029112779, -286.3146966461031866, -288.8567916984801514 ) ) ;
#71673 = CARTESIAN_POINT ( 'NONE',  ( -96.14781653577701093, -278.0489294418554778, -320.0890195875368818 ) ) ;
#71674 = CARTESIAN_POINT ( 'NONE',  ( 24.52136526099614144, -292.2169197850424780, -313.7688859149677683 ) ) ;
#71675 = CARTESIAN_POINT ( 'NONE',  ( 29.28764477213070094, -280.8835762765841082, -231.7666831161311052 ) ) ;
#71676 = AXIS2_PLACEMENT_3D ( 'NONE', #59649, #59165, #32140 ) ;
#71677 = CARTESIAN_POINT ( 'NONE',  ( -93.86949603807366316, -275.0857538483523399, -222.2221177736223297 ) ) ;
#71678 = AXIS2_PLACEMENT_3D ( 'NONE', #21599, #43374, #72269 ) ;
#71679 = EDGE_CURVE ( 'NONE', #42461, #31710, #14133, .T. ) ;
#71680 = CARTESIAN_POINT ( 'NONE',  ( 21.27581636871892101, -295.4090924074130839, -223.5744983911110353 ) ) ;
#71681 = CARTESIAN_POINT ( 'NONE',  ( 23.67967844883697026, -273.1819578725408633, -225.0801576086992384 ) ) ;
#71682 = DIRECTION ( 'NONE',  ( 0.000000000000000000, 0.000000000000000000, 1.000000000000000000 ) ) ;
#71683 = CARTESIAN_POINT ( 'NONE',  ( -4.314145064791616413, -280.0073286965790089, -205.1769067137720697 ) ) ;
#71684 = CIRCLE ( 'NONE', #88266, 204.0731808058633590 ) ;
#71685 = CARTESIAN_POINT ( 'NONE',  ( 24.05863392048273397, -277.3696781411160828, -316.1651319809926690 ) ) ;
#71686 = CARTESIAN_POINT ( 'NONE',  ( -98.95074209796707976, -298.5317832405259537, -230.0233642950922217 ) ) ;
#71687 = CARTESIAN_POINT ( 'NONE',  ( -47.23793639681001366, -282.2337233190768870, -346.4852581763551029 ) ) ;
#71688 = CARTESIAN_POINT ( 'NONE',  ( -110.4160519150708240, -292.1583542538229494, -282.1928394263150039 ) ) ;
#71689 = CARTESIAN_POINT ( 'NONE',  ( -91.61372663536592142, -274.8946426137387107, -216.8729178494533585 ) ) ;
#71690 = CARTESIAN_POINT ( 'NONE',  ( -55.23463433823114599, -275.1418104653753858, -195.9760309235535090 ) ) ;
#71691 = CARTESIAN_POINT ( 'NONE',  ( 196.7510731661265595, -141.7221692137691775, 21.50000000000000000 ) ) ;
#71692 = CARTESIAN_POINT ( 'NONE',  ( 9.392485132521358082, -296.4087377666173211, -328.8738142022788224 ) ) ;
#71693 = CARTESIAN_POINT ( 'NONE',  ( -71.06332043049040692, -281.4980089476669036, -337.1802455307663990 ) ) ;
#71694 = CARTESIAN_POINT ( 'NONE',  ( -113.3398548395350076, -290.0656463711811739, -282.6095779671533137 ) ) ;
#71695 = CARTESIAN_POINT ( 'NONE',  ( 35.17864991614144543, -273.8010451705940227, -288.0966731952875648 ) ) ;
#71696 = CARTESIAN_POINT ( 'NONE',  ( 13.69578042214607549, -288.3530144382849016, -213.7075207084152453 ) ) ;
#71697 = AXIS2_PLACEMENT_3D ( 'NONE', #50575, #21224, #71911 ) ;
#71698 = CARTESIAN_POINT ( 'NONE',  ( -109.0098733389127403, -289.6750882933995968, -254.9371423846353935 ) ) ;
#71699 = EDGE_LOOP ( 'NONE', ( #11954, #23131, #52211, #50794, #85870 ) ) ;
#71700 = CARTESIAN_POINT ( 'NONE',  ( -96.99211262239884945, -289.7715144920263697, -222.6072219637948422 ) ) ;
#71701 = CARTESIAN_POINT ( 'NONE',  ( -107.0205207128411189, -290.5087291010706849, -248.4798317883383163 ) ) ;
#71702 = ORIENTED_EDGE ( 'NONE', *, *, #11258, .F. ) ;
#71703 = CARTESIAN_POINT ( 'NONE',  ( 38.66707351460367903, -288.5036681321446395, -260.1552942077444754 ) ) ;
#71704 = CARTESIAN_POINT ( 'NONE',  ( 20.85634145735024347, -276.5050219194279180, -314.4641274317513648 ) ) ;
#71705 = ADVANCED_FACE ( 'NONE', ( #78489, #6987, #50051, #93145, #14096 ), #6052, .F. ) ;
#71706 = CARTESIAN_POINT ( 'NONE',  ( -24.97127819426458828, -293.8183886548726491, -346.1015899336565553 ) ) ;
#71707 = CARTESIAN_POINT ( 'NONE',  ( -55.66983819907394349, -283.9335075615382493, -345.0430578416849130 ) ) ;
#71708 = CARTESIAN_POINT ( 'NONE',  ( -97.56651273162216853, -285.5274993009537070, -222.4161887559072568 ) ) ;
#71709 = CARTESIAN_POINT ( 'NONE',  ( -36.18894229743908397, -283.3705864035105151, -343.3731624427013571 ) ) ;
#71710 = CARTESIAN_POINT ( 'NONE',  ( 203.5338562182569149, 295.8836489450777094, -54.00000000004095568 ) ) ;
#71711 = CARTESIAN_POINT ( 'NONE',  ( 201.9871130242204345, 295.7236060444520263, -68.57413240043143787 ) ) ;
#71712 = CARTESIAN_POINT ( 'NONE',  ( 152.0738250329050345, 205.6678486289000602, -214.6699954404999175 ) ) ;
#71713 = CARTESIAN_POINT ( 'NONE',  ( -11.42347044757535102, -273.5956507169744327, -201.8902325781756986 ) ) ;
#71714 = CARTESIAN_POINT ( 'NONE',  ( 22.54124422908810388, -273.8844686918206435, -228.0515702116383068 ) ) ;
#71715 = CARTESIAN_POINT ( 'NONE',  ( -109.3821301432877817, -295.7161436859888681, -297.5244840198336647 ) ) ;
#71716 = CARTESIAN_POINT ( 'NONE',  ( 203.1406098482175082, 291.9636561924038460, -68.25767031306274646 ) ) ;
#71717 = CARTESIAN_POINT ( 'NONE',  ( -64.70794031982967454, -272.3870210641824769, -198.9020305056669145 ) ) ;
#71718 = CARTESIAN_POINT ( 'NONE',  ( -104.8515973134611556, -298.8234751508008458, -239.3620821199822046 ) ) ;
#71719 = CARTESIAN_POINT ( 'NONE',  ( 29.88288232784202592, -289.2658341984018762, -300.1875965994962030 ) ) ;
#71720 = CARTESIAN_POINT ( 'NONE',  ( -75.15076886893835706, -292.6155511243106275, -207.4949966826860930 ) ) ;
#71721 = ORIENTED_EDGE ( 'NONE', *, *, #9205, .T. ) ;
#71722 = CARTESIAN_POINT ( 'NONE',  ( -105.0517392887751527, -297.9634991113347837, -234.0796786594165155 ) ) ;
#71723 = CARTESIAN_POINT ( 'NONE',  ( -12.00651713241685670, -286.8833571480352020, -201.8328979252069928 ) ) ;
#71724 = CARTESIAN_POINT ( 'NONE',  ( 39.34175060679670111, -294.4258670534229623, -276.0170551198291378 ) ) ;
#71725 = CARTESIAN_POINT ( 'NONE',  ( -86.35129232163889412, -296.2041091161521535, -329.6703649519598116 ) ) ;
#71726 = CARTESIAN_POINT ( 'NONE',  ( 33.30766822546267747, -293.4762330291529793, -251.9854069548942448 ) ) ;
#71727 = VERTEX_POINT ( 'NONE', #78946 ) ;
#71728 = CARTESIAN_POINT ( 'NONE',  ( -31.39818384300815168, -276.0467811391014834, -195.0222009776275911 ) ) ;
#71729 = ORIENTED_EDGE ( 'NONE', *, *, #44269, .T. ) ;
#71730 = CARTESIAN_POINT ( 'NONE',  ( -73.73099912836624981, -279.0899859423332714, -202.5571996825050860 ) ) ;
#71731 = CARTESIAN_POINT ( 'NONE',  ( 22.94600557011623110, -273.3640957574764911, -227.7736029834128999 ) ) ;
#71732 = CARTESIAN_POINT ( 'NONE',  ( -68.42610636966820437, -274.7136067350936059, -203.9546977671403170 ) ) ;
#71733 = CIRCLE ( 'NONE', #86835, 0.5000000000000129896 ) ;
#71734 = CARTESIAN_POINT ( 'NONE',  ( 35.83769547813096779, -276.5453796724441986, -274.3134172970944746 ) ) ;
#71735 = CARTESIAN_POINT ( 'NONE',  ( 36.29758806142450567, -277.0746468417739266, -251.6200067206809763 ) ) ;
#71736 = CARTESIAN_POINT ( 'NONE',  ( 38.06127762496454636, -273.5827152938435347, -271.1794932906690860 ) ) ;
#71737 = CARTESIAN_POINT ( 'NONE',  ( -110.2000743452557572, -297.1172064540436963, -276.9170275267924239 ) ) ;
#71738 = CARTESIAN_POINT ( 'NONE',  ( -26.13544043930307126, -293.4814049398514157, -343.0920925375120873 ) ) ;
#71739 = DIRECTION ( 'NONE',  ( 0.000000000000000000, -0.000000000000000000, 1.000000000000000000 ) ) ;
#71740 = CARTESIAN_POINT ( 'NONE',  ( -77.46577931404308970, -280.0217816100312689, -204.6520080396967671 ) ) ;
#71741 = CARTESIAN_POINT ( 'NONE',  ( 32.09883516742757337, -276.0175712705664068, -292.8780463338557638 ) ) ;
#71742 = TOROIDAL_SURFACE ( 'NONE', #30888, 5.343514653206205445, 1.000000000000000000 ) ;
#71743 = CARTESIAN_POINT ( 'NONE',  ( -1.187718770075380625, -285.2064826773611230, -202.9356932109756713 ) ) ;
#71744 = CARTESIAN_POINT ( 'NONE',  ( -37.28125707365905583, -300.0530651684923669, -195.1936765916527463 ) ) ;
#71745 = CARTESIAN_POINT ( 'NONE',  ( 82.62898823957701211, -301.1181951566114208, -197.3182997069781948 ) ) ;
#71746 = AXIS2_PLACEMENT_3D ( 'NONE', #56748, #21669, #35876 ) ;
#71747 = CARTESIAN_POINT ( 'NONE',  ( 31.99688712007001001, -286.4399460987569910, -247.0209799082480515 ) ) ;
#71748 = AXIS2_PLACEMENT_3D ( 'NONE', #43163, #71117, #78223 ) ;
#71749 = CARTESIAN_POINT ( 'NONE',  ( -84.06025536891111472, -277.6401271231392798, -212.8896557090281760 ) ) ;
#71750 = CARTESIAN_POINT ( 'NONE',  ( -71.19671980122386401, -278.1708654903962383, -205.0077067614502937 ) ) ;
#71751 = CARTESIAN_POINT ( 'NONE',  ( -36.52480683115501847, -285.0420590774318157, -345.3692216833477460 ) ) ;
#71752 = CARTESIAN_POINT ( 'NONE',  ( -89.35644591605554865, -279.0094471131884575, -322.2174095497524036 ) ) ;
#71753 = DIRECTION ( 'NONE',  ( 0.000000000000000000, 0.000000000000000000, 1.000000000000000000 ) ) ;
#71755 = CARTESIAN_POINT ( 'NONE',  ( 14.32561868106340519, -274.7405479958995898, -326.4412052992155395 ) ) ;
#71754 = AXIS2_PLACEMENT_3D ( 'NONE', #47338, #40694, #92310 ) ;
#71756 = CARTESIAN_POINT ( 'NONE',  ( 5.229381813058770589, -275.2962646132127134, -210.8713289407209004 ) ) ;
#71757 = CARTESIAN_POINT ( 'NONE',  ( 27.68744924600936130, -283.0500678239332046, -232.6618055744356184 ) ) ;
#71758 = DIRECTION ( 'NONE',  ( -0.8435586647355751699, 0.000000000000000000, -0.5370370370370497470 ) ) ;
#71759 = CARTESIAN_POINT ( 'NONE',  ( 35.40480076664930209, -289.7337065991507643, -290.8355867802104626 ) ) ;
#71760 = CARTESIAN_POINT ( 'NONE',  ( 36.88031470064380102, -291.6914703853266815, -281.2241205064065639 ) ) ;
#71761 = CIRCLE ( 'NONE', #38461, 4.103083949679980691 ) ;
#71762 = CARTESIAN_POINT ( 'NONE',  ( 82.14511625994450128, -299.8483204291535458, -197.3559792037316356 ) ) ;
#71763 = CARTESIAN_POINT ( 'NONE',  ( -3.865200399341448101, -273.1881556656844054, -204.9209433488237835 ) ) ;
#71764 = CARTESIAN_POINT ( 'NONE',  ( 31.99032694162384161, -291.3432971920728392, -243.8293351380426657 ) ) ;
#71765 = CARTESIAN_POINT ( 'NONE',  ( 180.5468918863934960, 256.3577768311903355, -167.2605672291198857 ) ) ;
#71766 = FACE_OUTER_BOUND ( 'NONE', #78746, .T. ) ;
#71767 = CARTESIAN_POINT ( 'NONE',  ( -113.4228607040191719, -288.9498270393111170, -276.8749633338974832 ) ) ;
#71768 = CARTESIAN_POINT ( 'NONE',  ( -93.15089247011005114, -285.4714811356282098, -318.6687930223515082 ) ) ;
#71769 = CARTESIAN_POINT ( 'NONE',  ( -10.33289605331482086, -284.6395534953461492, -199.2804243918201053 ) ) ;
#71770 = CARTESIAN_POINT ( 'NONE',  ( -13.32001105019807419, -284.1593826679187487, -339.9732896615436744 ) ) ;
#71771 = CARTESIAN_POINT ( 'NONE',  ( -110.5519284178350432, -285.3476241554911894, -270.9207150378398978 ) ) ;
#71772 = CARTESIAN_POINT ( 'NONE',  ( -94.43165724661248817, -293.2108330865286234, -221.1565965264391593 ) ) ;
#71773 = CARTESIAN_POINT ( 'NONE',  ( -0.05940419736651295773, -274.8675158897616484, -202.9979689485211907 ) ) ;
#71774 = CARTESIAN_POINT ( 'NONE',  ( -105.2306614181790394, -288.1965610808502447, -303.6524513911197687 ) ) ;
#71775 = CARTESIAN_POINT ( 'NONE',  ( -93.33399293753780057, -277.8297409066191790, -323.2946352185534238 ) ) ;
#71776 = CARTESIAN_POINT ( 'NONE',  ( 25.83246074067539766, -296.0702777093330269, -310.2184456057734110 ) ) ;
#71777 = CARTESIAN_POINT ( 'NONE',  ( -48.18343439339134449, -258.6462052220593932, -448.1683005986229205 ) ) ;
#71778 = CARTESIAN_POINT ( 'NONE',  ( -106.6379572354042296, -298.6233781216988632, -303.7686719486574702 ) ) ;
#71779 = CARTESIAN_POINT ( 'NONE',  ( -89.25441501243226128, -282.4860578409909522, -322.4548065540936932 ) ) ;
#71780 = CARTESIAN_POINT ( 'NONE',  ( -38.12284122492987848, -278.0422048612285266, -195.3651816150428147 ) ) ;
#71781 = CARTESIAN_POINT ( 'NONE',  ( 18.67717997959611509, -297.1422734259927552, -194.1760574865865578 ) ) ;
#71782 = CARTESIAN_POINT ( 'NONE',  ( 16.60077602297621624, -275.6076851503423200, -319.7164042526050594 ) ) ;
#71783 = CARTESIAN_POINT ( 'NONE',  ( -36.21476309781461111, -293.5866219212883266, -196.6638040726873271 ) ) ;
#71784 = CARTESIAN_POINT ( 'NONE',  ( 32.85116189184988400, -294.2157563226932098, -249.2969822167947314 ) ) ;
#71785 = CARTESIAN_POINT ( 'NONE',  ( -90.35819045901187962, -297.0984566409026115, -325.5933545764800101 ) ) ;
#71786 = CARTESIAN_POINT ( 'NONE',  ( -84.47972061007992295, -295.5554891598225709, -326.1680224458586963 ) ) ;
#71787 = CARTESIAN_POINT ( 'NONE',  ( -12.60483822100766638, -290.7306689651027227, -341.1642839473477125 ) ) ;
#71788 = CARTESIAN_POINT ( 'NONE',  ( -94.39772701254746323, -284.0162330430446787, -322.0876337816351906 ) ) ;
#71789 = CARTESIAN_POINT ( 'NONE',  ( 20.91651007074587199, -273.0296657700174023, -221.9226371214035964 ) ) ;
#71790 = CARTESIAN_POINT ( 'NONE',  ( 39.70243564528419711, -287.4003836784361283, -271.5534072559087804 ) ) ;
#71791 = CARTESIAN_POINT ( 'NONE',  ( -39.17341128849477627, -279.0551466767266220, -344.9834446690304617 ) ) ;
#71792 = EDGE_CURVE ( 'NONE', #84462, #25231, #7892, .T. ) ;
#71793 = CARTESIAN_POINT ( 'NONE',  ( -6.907823991882188430, -285.5203864706758168, -203.7351273666220948 ) ) ;
#71794 = CARTESIAN_POINT ( 'NONE',  ( -5.213529017842083668, -286.6291991916397706, -338.1452803980457134 ) ) ;
#71795 = CARTESIAN_POINT ( 'NONE',  ( 6.757860130087521178, -59.91093500391586701, -350.7441993381422094 ) ) ;
#71796 = CARTESIAN_POINT ( 'NONE',  ( -39.96985841273527740, -285.5258924766216069, -197.3468644025854815 ) ) ;
#71797 = CARTESIAN_POINT ( 'NONE',  ( -58.41062556564010322, -284.2591540747295653, -344.2332485280205105 ) ) ;
#71798 = CARTESIAN_POINT ( 'NONE',  ( -77.03729641764570601, -290.5931043268431040, -204.5953297476051773 ) ) ;
#71799 = CARTESIAN_POINT ( 'NONE',  ( -56.37671641447296622, -281.4111123504840180, -196.5224822393548152 ) ) ;
#71800 = CARTESIAN_POINT ( 'NONE',  ( -102.9970570815455062, -280.3839199487563860, -230.9812036140839666 ) ) ;
#71801 = CARTESIAN_POINT ( 'NONE',  ( -11.74115963651981431, -280.2281699228663001, -201.9438366833783789 ) ) ;
#71802 = CARTESIAN_POINT ( 'NONE',  ( -66.47790118651256819, -275.6485854813661831, -201.6375514828009159 ) ) ;
#71803 = CARTESIAN_POINT ( 'NONE',  ( -33.43483734184238187, -295.0042770022172363, -347.2750593515710307 ) ) ;
#71804 = CARTESIAN_POINT ( 'NONE',  ( -37.29166841799597165, -287.0716328945454734, -345.0059055043241187 ) ) ;
#71805 =( BOUNDED_SURFACE ( )  B_SPLINE_SURFACE ( 3, 2, ( 
 ( #1400, #10234, #39102 ),
 ( #80940, #53808, #80464 ),
 ( #68956, #30287, #89769 ),
 ( #4087, #59174, #76049 ),
 ( #90233, #65845, #39559 ),
 ( #61851, #75124, #68014 ),
 ( #88019, #82676, #3143 ),
 ( #17825, #32958, #83132 ),
 ( #8499, #32025, #60922 ),
 ( #18283, #75581, #8036 ),
 ( #36931, #24931, #29831 ),
 ( #72910, #46678, #68481 ),
 ( #3617, #25382, #46220 ),
 ( #22256, #23175, #15613 ),
 ( #51129, #73389, #52057 ),
 ( #32504, #37377, #61401 ),
 ( #54262, #47139, #953 ),
 ( #11180, #58714, #80012 ),
 ( #44012, #87558, #22704 ),
 ( #51578, #44484, #66287 ),
 ( #62319, #20636, #49506 ),
 ( #83599, #56639, #34372 ),
 ( #33902, #5021, #25842 ),
 ( #41915, #26798, #84073 ),
 ( #63277, #48081, #76523 ),
 ( #55684, #54723, #92110 ),
 ( #70828, #27264, #19682 ),
 ( #18762, #4542, #91644 ),
 ( #41442, #69411, #12115 ),
 ( #56151, #13079, #34834 ),
 ( #47620, #70374, #5499 ),
 ( #84535, #85006, #55219 ) ),
 .UNSPECIFIED., .F., .F., .F. ) 
 B_SPLINE_SURFACE_WITH_KNOTS ( ( 4, 2, 2, 2, 2, 2, 2, 2, 2, 2, 2, 2, 2, 2, 2, 4 ),
 ( 3, 3 ),
 ( 0.000000000000000000, 0.005866952128964776289, 0.008800428193447163566, 0.01173390425792955258, 0.01760085638689432713, 0.01906759441913552164, 0.02053433245137671614, 0.02346780851585910516, 0.02933476064482387971, 0.03080149867706507422, 0.03226823670930626525, 0.03520171277378865426, 0.03813518883827104328, 0.03960192687051224125, 0.04106866490275343229, 0.04693561703171821031 ),
 ( 0.000000000000000000, 1.000000000000000000 ),
 .UNSPECIFIED. ) 
 GEOMETRIC_REPRESENTATION_ITEM ( )  RATIONAL_B_SPLINE_SURFACE ( (
 ( 1.000000000000000000, 0.7071067811865480168, 1.000000000000000000),
 ( 1.000000000000000000, 0.7090210024396556010, 1.000000000000000000),
 ( 1.000000000000000000, 0.7108407973597864471, 1.000000000000000000),
 ( 1.000000000000000000, 0.7134470143025161137, 1.000000000000000000),
 ( 1.000000000000000000, 0.7142951270337911662, 1.000000000000000000),
 ( 1.000000000000000000, 0.7159522736098768991, 1.000000000000000000),
 ( 1.000000000000000000, 0.7167636429391108788, 1.000000000000000000),
 ( 1.000000000000000000, 0.7190918835810566900, 1.000000000000000000),
 ( 1.000000000000000000, 0.7205207347168143261, 1.000000000000000000),
 ( 1.000000000000000000, 0.7221727232895018833, 1.000000000000000000),
 ( 1.000000000000000000, 0.7224963568879022580, 1.000000000000000000),
 ( 1.000000000000000000, 0.7231303645827314996, 1.000000000000000000),
 ( 1.000000000000000000, 0.7234414309858798742, 1.000000000000000000),
 ( 1.000000000000000000, 0.7243500205383740509, 1.000000000000000000),
 ( 1.000000000000000000, 0.7249196227328268405, 1.000000000000000000),
 ( 1.000000000000000000, 0.7265289715998781706, 1.000000000000000000),
 ( 1.000000000000000000, 0.7274702368494421201, 1.000000000000000000),
 ( 1.000000000000000000, 0.7284953164274693416, 1.000000000000000000),
 ( 1.000000000000000000, 0.7286931934763172247, 1.000000000000000000),
 ( 1.000000000000000000, 0.7290707267997620367, 1.000000000000000000),
 ( 1.000000000000000000, 0.7292503229930066277, 1.000000000000000000),
 ( 1.000000000000000000, 0.7297626290626116896, 1.000000000000000000),
 ( 1.000000000000000000, 0.7300689337816327340, 1.000000000000000000),
 ( 1.000000000000000000, 0.7306145467741796962, 1.000000000000000000),
 ( 1.000000000000000000, 0.7308538497138195034, 1.000000000000000000),
 ( 1.000000000000000000, 0.7311633277236124773, 1.000000000000000000),
 ( 1.000000000000000000, 0.7312582226261189478, 1.000000000000000000),
 ( 1.000000000000000000, 0.7314313872177583553, 1.000000000000000000),
 ( 1.000000000000000000, 0.7315097857000790738, 1.000000000000000000),
 ( 1.000000000000000000, 0.7318569749151436765, 1.000000000000000000),
 ( 1.000000000000000000, 0.7319944972810035200, 1.000000000000000000),
 ( 1.000000000000000000, 0.7319951502423088785, 1.000000000000000000) ) ) 
 REPRESENTATION_ITEM ( '' )  SURFACE ( )  );
#71806 = CARTESIAN_POINT ( 'NONE',  ( -94.12886339872447650, -292.8486873343707089, -219.5510943273570774 ) ) ;
#71807 = CARTESIAN_POINT ( 'NONE',  ( -88.33090852815483629, -296.2379229793014019, -217.6183804543549059 ) ) ;
#71808 = CARTESIAN_POINT ( 'NONE',  ( 19.61157610432797682, -284.1401972384553574, -318.3146023257164074 ) ) ;
#71809 = CARTESIAN_POINT ( 'NONE',  ( -95.62377097541222781, -295.6008385683056190, -314.3736224449548331 ) ) ;
#71810 = CARTESIAN_POINT ( 'NONE',  ( -19.47219931230847934, -293.3563255569554826, -195.7265381718005415 ) ) ;
#71811 = CIRCLE ( 'NONE', #760, 25.00000000000000355 ) ;
#71812 = CARTESIAN_POINT ( 'NONE',  ( -6.734302065397562487, -281.1162920441148572, -203.9616130972737267 ) ) ;
#71813 = ADVANCED_FACE ( 'NONE', ( #72315 ), #21653, .T. ) ;
#71814 = CARTESIAN_POINT ( 'NONE',  ( -3.917687623041965495, -273.5410258234661001, -201.2405341016468867 ) ) ;
#71815 = CARTESIAN_POINT ( 'NONE',  ( -78.07536641740080086, -290.2354931316477291, -335.6465472546024671 ) ) ;
#71816 = CARTESIAN_POINT ( 'NONE',  ( -103.3526660253210565, -282.2001359180881082, -307.6542321543950607 ) ) ;
#71817 = CARTESIAN_POINT ( 'NONE',  ( -113.6457656654463761, -291.0175439808587612, -259.8004684760299483 ) ) ;
#71818 = CARTESIAN_POINT ( 'NONE',  ( 22.76971771980765169, -288.4628996621580654, -311.8404260667226708 ) ) ;
#71819 = LINE ( 'NONE', #20676, #628 ) ;
#71820 = CARTESIAN_POINT ( 'NONE',  ( 178.1189667068858000, 253.6096096343568718, -165.4786255472319851 ) ) ;
#71821 = CARTESIAN_POINT ( 'NONE',  ( 160.8675658356268343, 217.7272039891784061, -202.3614854212502507 ) ) ;
#71822 = AXIS2_PLACEMENT_3D ( 'NONE', #88427, #404, #1791 ) ;
#71823 = CARTESIAN_POINT ( 'NONE',  ( 21.31550574532286291, -278.4094976428775681, -223.6242672951989618 ) ) ;
#71824 = CARTESIAN_POINT ( 'NONE',  ( -109.0434605104278916, -277.9415497043815435, -255.7566106584714305 ) ) ;
#71825 = EDGE_LOOP ( 'NONE', ( #61244, #80508, #85673, #30336 ) ) ;
#71826 = CARTESIAN_POINT ( 'NONE',  ( -94.17147791813980007, -278.1252562387663261, -224.0512655645141251 ) ) ;
#71827 = CARTESIAN_POINT ( 'NONE',  ( 26.12953847396074636, -274.6436266326655868, -226.7815111782266229 ) ) ;
#71828 = CARTESIAN_POINT ( 'NONE',  ( 200.6534333971687545, 286.0685513885803175, -96.65979452701760977 ) ) ;
#71829 = CARTESIAN_POINT ( 'NONE',  ( -88.52321589316306927, -277.9255405016471059, -213.6243685558584389 ) ) ;
#71830 = CARTESIAN_POINT ( 'NONE',  ( 10.95412489501575237, -280.4006190535507699, -327.3444478219906841 ) ) ;
#71831 = CARTESIAN_POINT ( 'NONE',  ( -102.9858506830102982, -298.8180980861067155, -231.9844126909268596 ) ) ;
#71832 = AXIS2_PLACEMENT_3D ( 'NONE', #6958, #93572, #28729 ) ;
#71833 = CARTESIAN_POINT ( 'NONE',  ( 20.22751120956337090, -293.4106919018047392, -225.3544864841448430 ) ) ;
#71834 = VERTEX_POINT ( 'NONE', #6522 ) ;
#71835 = CARTESIAN_POINT ( 'NONE',  ( 16.35993724086789669, -286.9544814030525686, -320.6090373511225380 ) ) ;
#71836 = CARTESIAN_POINT ( 'NONE',  ( 37.84397290280745096, -276.0006901711001888, -254.1611371329152576 ) ) ;
#71837 = CARTESIAN_POINT ( 'NONE',  ( -109.5827616559154478, -272.6952085234271408, -259.5166644620624652 ) ) ;
#71838 = ORIENTED_EDGE ( 'NONE', *, *, #71165, .T. ) ;
#71839 = CARTESIAN_POINT ( 'NONE',  ( 156.0793278192250284, 19.94580804510101402, 11.55434249967772331 ) ) ;
#71840 = CARTESIAN_POINT ( 'NONE',  ( 23.93337300590344796, -282.0751160316062851, -230.0254482823178250 ) ) ;
#71841 = CARTESIAN_POINT ( 'NONE',  ( -42.38547125463780674, -281.7494994651199818, -194.5420281233098763 ) ) ;
#71842 = CARTESIAN_POINT ( 'NONE',  ( -109.2127080932688727, -283.4258861820418929, -284.4311806257383068 ) ) ;
#71843 = CARTESIAN_POINT ( 'NONE',  ( 36.66240991557043571, -283.4965634792587252, -276.8356852629276545 ) ) ;
#71844 = CARTESIAN_POINT ( 'NONE',  ( -8.484855210382525215, -275.1473203404668766, -338.1832693540746391 ) ) ;
#71845 = CARTESIAN_POINT ( 'NONE',  ( 175.2296996224750103, 247.0000000000001137, -8.550761578869359170 ) ) ;
#71846 = DIRECTION ( 'NONE',  ( 1.000000000000000000, 0.000000000000000000, 0.000000000000000000 ) ) ;
#71847 = CARTESIAN_POINT ( 'NONE',  ( -9.261289996373720967, -277.4970613775752781, -341.8848859715651543 ) ) ;
#71848 = CARTESIAN_POINT ( 'NONE',  ( 183.0442525570908288, 300.2961574867697436, 7.500000000000000000 ) ) ;
#71849 = CARTESIAN_POINT ( 'NONE',  ( -95.71092465805593008, -276.4572345150953083, -319.6929802806191105 ) ) ;
#71850 = VERTEX_POINT ( 'NONE', #28300 ) ;
#71851 = CARTESIAN_POINT ( 'NONE',  ( 165.2494399300530290, 8.542400036368780647, 10.00000000000000000 ) ) ;
#71852 = CARTESIAN_POINT ( 'NONE',  ( -94.07932934483878284, -285.8466524513269746, -319.9519259584895963 ) ) ;
#71853 = CARTESIAN_POINT ( 'NONE',  ( 34.87498181864536662, -292.5940224921241111, -258.5629605926766317 ) ) ;
#71854 = CARTESIAN_POINT ( 'NONE',  ( -9.607842461548836255, -288.0477173232401356, -342.0838195875194856 ) ) ;
#71855 = CARTESIAN_POINT ( 'NONE',  ( -11.64949625698807267, -284.6312320025913891, -200.9501341726753481 ) ) ;
#71857 = CARTESIAN_POINT ( 'NONE',  ( -69.21438447158695340, -287.7171972962955806, -337.1601150514024425 ) ) ;
#71856 = CARTESIAN_POINT ( 'NONE',  ( -84.00762512323545650, -283.9713642507327904, -213.3944268964577304 ) ) ;
#71858 = CARTESIAN_POINT ( 'NONE',  ( 34.03990156219499852, -282.9820533688626369, -287.4967131971842491 ) ) ;
#71859 = CARTESIAN_POINT ( 'NONE',  ( -49.37264000728440294, -271.8987596729892857, -196.2799532956359769 ) ) ;
#71860 = CARTESIAN_POINT ( 'NONE',  ( -111.7483806585477737, -282.7443390403341255, -286.7954208593439489 ) ) ;
#71861 = CARTESIAN_POINT ( 'NONE',  ( -94.95819166640239928, -297.8890205352169005, -318.3950405513293163 ) ) ;
#71862 = CARTESIAN_POINT ( 'NONE',  ( -88.61657461520258039, -283.3351405280789095, -215.3274922950619725 ) ) ;
#71863 = CARTESIAN_POINT ( 'NONE',  ( -95.80680844947880814, -280.1111808145026316, -226.2354279263412877 ) ) ;
#71864 = CARTESIAN_POINT ( 'NONE',  ( 33.35702277406612382, -289.8843162584950619, -296.0414864011003147 ) ) ;
#71865 = DIRECTION ( 'NONE',  ( -0.000000000000000000, 1.000000000000000000, -0.000000000000000000 ) ) ;
#71866 = CARTESIAN_POINT ( 'NONE',  ( 201.2104617360081704, 250.0000000000000568, 15.00000000000000000 ) ) ;
#71867 = CARTESIAN_POINT ( 'NONE',  ( 37.19001511173541985, -295.6316360208157903, -282.8629346609000095 ) ) ;
#71868 = CARTESIAN_POINT ( 'NONE',  ( -94.26065944382695250, -275.8752571861291472, -319.1999623771977781 ) ) ;
#71869 = CARTESIAN_POINT ( 'NONE',  ( -109.7169137284815292, -289.4211266837438643, -296.3256483703961521 ) ) ;
#71870 = CARTESIAN_POINT ( 'NONE',  ( -53.34246703258771305, -293.6605142541033615, -342.4582160637586981 ) ) ;
#71871 = CARTESIAN_POINT ( 'NONE',  ( -83.73617232210561667, -278.0850227333908720, -213.2970478755840986 ) ) ;
#71872 = CARTESIAN_POINT ( 'NONE',  ( -44.66779988183058947, -296.0981804581261940, -196.4370623990203057 ) ) ;
#71873 = CARTESIAN_POINT ( 'NONE',  ( -14.71034408175546204, -293.6668524809140308, -200.4392673152705697 ) ) ;
#71874 = CARTESIAN_POINT ( 'NONE',  ( -20.25526795762937127, -282.7662352645559736, -195.3538533559490702 ) ) ;
#71875 = CARTESIAN_POINT ( 'NONE',  ( -55.92037789959892535, -293.7670642906631429, -344.3715259207385770 ) ) ;
#71876 = CARTESIAN_POINT ( 'NONE',  ( -45.43010981144384886, -290.7564741773368837, -343.7165407087683775 ) ) ;
#71877 = CARTESIAN_POINT ( 'NONE',  ( -66.60422421857569475, -289.9139373957862631, -200.2349552563926238 ) ) ;
#71878 = ADVANCED_FACE ( 'NONE', ( #57190, #43420, #7436 ), #36318, .F. ) ;
#71879 = CARTESIAN_POINT ( 'NONE',  ( -64.01769526253177389, -290.8321761863759889, -338.9997427166684361 ) ) ;
#71880 = FACE_OUTER_BOUND ( 'NONE', #48159, .T. ) ;
#71881 = CARTESIAN_POINT ( 'NONE',  ( -21.08353462347372442, -289.6409983149790150, -341.6932550656483727 ) ) ;
#71882 = LINE ( 'NONE', #7451, #21845 ) ;
#71883 = CARTESIAN_POINT ( 'NONE',  ( -87.11472619302482201, -290.9323324330699734, -328.6601051939372269 ) ) ;
#71885 = CARTESIAN_POINT ( 'NONE',  ( -108.4274720254899762, -290.7719533778829373, -253.6989850963954893 ) ) ;
#71884 = CARTESIAN_POINT ( 'NONE',  ( 34.04266256342511809, -279.8848159900762198, -294.6618718617010018 ) ) ;
#71886 = CARTESIAN_POINT ( 'NONE',  ( -88.92042349984600946, -279.6838108229380850, -213.2176180303639228 ) ) ;
#71887 = CARTESIAN_POINT ( 'NONE',  ( 28.28475668372531615, -281.7458690025740111, -310.6978371835860457 ) ) ;
#71888 = AXIS2_PLACEMENT_3D ( 'NONE', #51172, #80059, #15199 ) ;
#71889 = CARTESIAN_POINT ( 'NONE',  ( 23.63203378177306035, -284.9568857978640608, -226.6019693509999797 ) ) ;
#71890 = FACE_OUTER_BOUND ( 'NONE', #24481, .T. ) ;
#71891 = CARTESIAN_POINT ( 'NONE',  ( -4.298279218856092321, -280.7514058464799405, -336.8366609902617483 ) ) ;
#71892 = CARTESIAN_POINT ( 'NONE',  ( -109.0071855195683952, -282.8391623291549877, -248.0718385701079001 ) ) ;
#71893 = CARTESIAN_POINT ( 'NONE',  ( 208.4306832106270519, 1.063508326895939771, 7.500000000000014211 ) ) ;
#71894 = CARTESIAN_POINT ( 'NONE',  ( -99.90821221285212062, -276.4493755390499814, -314.0433720304047824 ) ) ;
#71895 = AXIS2_PLACEMENT_3D ( 'NONE', #3686, #33479, #62382 ) ;
#71896 = CARTESIAN_POINT ( 'NONE',  ( -102.6620246555613676, -282.9451772856358502, -310.5450415452747848 ) ) ;
#71897 = CARTESIAN_POINT ( 'NONE',  ( -81.17591050855962465, -274.2422788104820484, -211.7214055761884879 ) ) ;
#71898 = CARTESIAN_POINT ( 'NONE',  ( 60.83509176750334291, -250.0104861964972258, 21.50000000000000000 ) ) ;
#71899 = CARTESIAN_POINT ( 'NONE',  ( -97.42440885179496490, -292.7455245028399986, -227.4201435665535200 ) ) ;
#71900 = CARTESIAN_POINT ( 'NONE',  ( -13.26548193127009867, -275.7841581728339406, -197.8425547780395277 ) ) ;
#71901 = CARTESIAN_POINT ( 'NONE',  ( -3.861551987416893095, -276.2643958327149107, -335.2546243397504213 ) ) ;
#71902 = CARTESIAN_POINT ( 'NONE',  ( 17.64225064007190014, -296.2658354164618117, -321.3686253435952267 ) ) ;
#71903 = CARTESIAN_POINT ( 'NONE',  ( -73.17198516148800991, -289.6804673459489550, -338.5315099698282211 ) ) ;
#71904 = CARTESIAN_POINT ( 'NONE',  ( 36.14210674182381666, -279.8568528140182821, -288.0072607088792438 ) ) ;
#71905 = CARTESIAN_POINT ( 'NONE',  ( -53.38724561063450835, -291.6852795057395156, -194.9969898139930820 ) ) ;
#71906 = CARTESIAN_POINT ( 'NONE',  ( -90.92318618272561537, -290.3266465976862492, -220.4183092012162319 ) ) ;
#71907 = CARTESIAN_POINT ( 'NONE',  ( -66.17960405431155380, -293.4294178791556078, -339.6091639940609639 ) ) ;
#71908 = ORIENTED_EDGE ( 'NONE', *, *, #20685, .F. ) ;
#71909 = DIRECTION ( 'NONE',  ( -1.000000000000000000, 0.000000000000000000, 0.000000000000000000 ) ) ;
#71910 = CARTESIAN_POINT ( 'NONE',  ( -72.65119488294536154, -291.0791912782864301, -206.3415606011172088 ) ) ;
#71911 = DIRECTION ( 'NONE',  ( -1.000000000000000000, 0.000000000000000000, 0.000000000000000000 ) ) ;
#71912 = CARTESIAN_POINT ( 'NONE',  ( 27.36219212280433055, -272.6237833571633473, -239.2376011013261916 ) ) ;
#71913 = CARTESIAN_POINT ( 'NONE',  ( -113.4210998570117681, -295.4776246276126130, -280.9853841982642848 ) ) ;
#71914 = CARTESIAN_POINT ( 'NONE',  ( -105.3381240462962722, -285.4110999573703111, -305.5449446909397011 ) ) ;
#71915 = CARTESIAN_POINT ( 'NONE',  ( 13.14108632914916264, -286.6147167758442720, -217.5610405691734570 ) ) ;
#71916 = CARTESIAN_POINT ( 'NONE',  ( 33.57026393535169007, -277.3354534249484118, -290.4622935678258386 ) ) ;
#71917 = CARTESIAN_POINT ( 'NONE',  ( -12.48374081865526541, -292.7475294770085839, -340.7997187035144293 ) ) ;
#71918 = CARTESIAN_POINT ( 'NONE',  ( -10.09641221913822129, -296.4516487380982426, -339.1773101233405328 ) ) ;
#71919 = CARTESIAN_POINT ( 'NONE',  ( -39.18302286459971384, -275.8706939163810716, -343.7350918185940145 ) ) ;
#71920 = EDGE_LOOP ( 'NONE', ( #45353, #33237 ) ) ;
#71921 = DIRECTION ( 'NONE',  ( 0.000000000000000000, -0.000000000000000000, 1.000000000000000000 ) ) ;
#71922 = CARTESIAN_POINT ( 'NONE',  ( -108.3571779278150160, -295.8393694218985956, -300.2067756596275103 ) ) ;
#71923 = CARTESIAN_POINT ( 'NONE',  ( 2.094785200861719154, -290.4398222184229894, -333.4965107657784529 ) ) ;
#71924 = CARTESIAN_POINT ( 'NONE',  ( 17.06571399127465583, -89.54582641780471874, 21.50000000000000000 ) ) ;
#71925 = CARTESIAN_POINT ( 'NONE',  ( -113.4697727941914422, -273.8642838345909922, -261.8449410113341855 ) ) ;
#71926 = CARTESIAN_POINT ( 'NONE',  ( 2.495627169251863009, -287.2532947722501149, -209.0677250120993449 ) ) ;
#71927 = ORIENTED_EDGE ( 'NONE', *, *, #84467, .T. ) ;
#71928 = CARTESIAN_POINT ( 'NONE',  ( -11.57700185046107499, -279.4382840174307603, -197.9934747404690825 ) ) ;
#71929 = CARTESIAN_POINT ( 'NONE',  ( 28.02365960625705910, -294.7351142535849249, -310.9665138797749933 ) ) ;
#71930 = CARTESIAN_POINT ( 'NONE',  ( -31.93890055105967107, -287.1243899591129320, -345.9847521395220724 ) ) ;
#71931 = CARTESIAN_POINT ( 'NONE',  ( -47.62454736191332216, -295.5127642150984002, -346.6500906078986191 ) ) ;
#71932 = CARTESIAN_POINT ( 'NONE',  ( 35.64232835602799554, -293.8547356705887523, -268.0332277545080046 ) ) ;
#71933 = CARTESIAN_POINT ( 'NONE',  ( 196.1375241020610076, 72.62792297770094763, -11.78658572562475904 ) ) ;
#71934 = CARTESIAN_POINT ( 'NONE',  ( 206.6195589736935005, 30.30844190587212594, 15.00000000000000000 ) ) ;
#71935 = CARTESIAN_POINT ( 'NONE',  ( 4.780671393231641808, -288.1295972354226933, -206.6710476202246696 ) ) ;
#71936 = CARTESIAN_POINT ( 'NONE',  ( 13.79469577742117181, -285.9094976428776249, -334.5364918783848793 ) ) ;
#71937 = ORIENTED_EDGE ( 'NONE', *, *, #8361, .T. ) ;
#71938 = CARTESIAN_POINT ( 'NONE',  ( -50.91348084202865465, -279.2316788741146070, -194.6701703431777730 ) ) ;
#71939 = CARTESIAN_POINT ( 'NONE',  ( -94.81413068156820145, -285.8888655477211955, -318.2876049841835311 ) ) ;
#71940 = CARTESIAN_POINT ( 'NONE',  ( -113.0184284125890315, -282.9890047163514168, -281.3014110167351873 ) ) ;
#71941 = CARTESIAN_POINT ( 'NONE',  ( 25.43995515728951062, -286.1743585002390660, -310.3583423453236492 ) ) ;
#71942 = CARTESIAN_POINT ( 'NONE',  ( 22.55632473083532474, -278.0423500418750109, -316.7775556500084235 ) ) ;
#71943 = CARTESIAN_POINT ( 'NONE',  ( -103.2259789066393694, -273.3111256698079501, -238.8754181093392788 ) ) ;
#71945 = ORIENTED_EDGE ( 'NONE', *, *, #32453, .F. ) ;
#71944 = EDGE_CURVE ( 'NONE', #78471, #60166, #43871, .T. ) ;
#71947 = CARTESIAN_POINT ( 'NONE',  ( -85.54518307666643295, -278.7128038947416258, -215.4037081136465304 ) ) ;
#71946 = CARTESIAN_POINT ( 'NONE',  ( -109.0432837039744527, -278.3704622780569480, -284.1342045455916150 ) ) ;
#71948 = CARTESIAN_POINT ( 'NONE',  ( 23.37963922902225988, -276.0038610314780385, -223.4952015767635487 ) ) ;
#71949 = CARTESIAN_POINT ( 'NONE',  ( -79.67848275044005391, -278.2889930618100607, -206.4570263846184162 ) ) ;
#71950 = CARTESIAN_POINT ( 'NONE',  ( -100.0119297896911377, -246.0268988372215802, -332.0617019485725336 ) ) ;
#71951 = EDGE_CURVE ( 'NONE', #71100, #34180, #2665, .T. ) ;
#71952 = CARTESIAN_POINT ( 'NONE',  ( -97.77916941543628582, -298.6065970111420143, -223.5861859380696899 ) ) ;
#71953 = CARTESIAN_POINT ( 'NONE',  ( 31.95455697924148097, -283.6233781216988064, -236.9535640164627637 ) ) ;
#71954 = EDGE_LOOP ( 'NONE', ( #31799, #21853, #38211, #83295 ) ) ;
#71955 = CARTESIAN_POINT ( 'NONE',  ( 161.2244399300530233, 8.542400036368780647, -9.000000000000001776 ) ) ;
#71956 = CARTESIAN_POINT ( 'NONE',  ( -87.91765652325517522, -286.4041919975886685, -217.2923069180827440 ) ) ;
#71957 = CARTESIAN_POINT ( 'NONE',  ( -77.99943868372949396, -287.2738242607385928, -206.1667077263731471 ) ) ;
#71958 = CARTESIAN_POINT ( 'NONE',  ( 34.62057467902984342, -287.0701160298207810, -283.2189433421929152 ) ) ;
#71959 = CARTESIAN_POINT ( 'NONE',  ( -114.2648508637497287, -284.1004888162801763, -267.1107478745750541 ) ) ;
#71960 = CARTESIAN_POINT ( 'NONE',  ( 21.98409525709180556, -279.3430133537986535, -226.4434813437808884 ) ) ;
#71961 = CARTESIAN_POINT ( 'NONE',  ( 5.417824719659231292, -288.4977835412642548, -209.6147155440238237 ) ) ;
#71962 = CARTESIAN_POINT ( 'NONE',  ( -6.461383909828068539, -278.9451089280148608, -203.4361030857936612 ) ) ;
#71963 = CARTESIAN_POINT ( 'NONE',  ( -96.47993366906230506, -279.2596039383150242, -314.0160555217643150 ) ) ;
#71964 = CARTESIAN_POINT ( 'NONE',  ( 30.33739946726818815, -276.4144734333676183, -298.0189885474565017 ) ) ;
#71965 = CARTESIAN_POINT ( 'NONE',  ( 16.39641102352779001, -287.1045198474900531, -325.0262930092932834 ) ) ;
#71966 = AXIS2_PLACEMENT_3D ( 'NONE', #15443, #29667, #58547 ) ;
#71967 = CARTESIAN_POINT ( 'NONE',  ( -79.06345468238039587, -284.4024513556360603, -334.8859505441761257 ) ) ;
#71968 = CARTESIAN_POINT ( 'NONE',  ( 11.45841264937041082, -282.8888217031168324, -329.9117917402192006 ) ) ;
#71969 = ORIENTED_EDGE ( 'NONE', *, *, #60435, .T. ) ;
#71970 = EDGE_LOOP ( 'NONE', ( #16907, #26273 ) ) ;
#71971 = CARTESIAN_POINT ( 'NONE',  ( 209.6287663260175975, 29.00782453271232697, 12.09245862095555601 ) ) ;
#71972 = CARTESIAN_POINT ( 'NONE',  ( -41.66599189590501595, -290.9664623462520012, -346.0154262564238365 ) ) ;
#71973 = CARTESIAN_POINT ( 'NONE',  ( -113.8750804876521130, -289.2622826738865456, -268.3508496036086513 ) ) ;
#71974 = CARTESIAN_POINT ( 'NONE',  ( -46.19537902311201805, -272.9958229657343622, -197.6629693275739612 ) ) ;
#71975 = CARTESIAN_POINT ( 'NONE',  ( 35.35896607655254797, -292.5826404289562674, -245.1414319223741529 ) ) ;
#71976 = CARTESIAN_POINT ( 'NONE',  ( -110.8155546239507601, -288.9495792697245520, -276.6701798364307479 ) ) ;
#71977 = CARTESIAN_POINT ( 'NONE',  ( 21.81708044103580235, -291.1760203637315954, -225.8840149151220942 ) ) ;
#71978 = CARTESIAN_POINT ( 'NONE',  ( 12.43630700787172749, -289.5455572973409062, -324.3679410442289281 ) ) ;
#71979 = CARTESIAN_POINT ( 'NONE',  ( -54.42813229853333468, -291.7662352645558599, -345.3683826091709648 ) ) ;
#71980 = CARTESIAN_POINT ( 'NONE',  ( -48.54443258265927597, -291.1948055562469335, -344.5722688021063504 ) ) ;
#71981 = CARTESIAN_POINT ( 'NONE',  ( -93.32835501897923791, -289.2489799189719974, -220.2061291768349065 ) ) ;
#71982 = B_SPLINE_CURVE_WITH_KNOTS ( 'NONE', 3,
 ( #67200, #10805, #24553, #66724, #9881, #46321 ),
 .UNSPECIFIED., .F., .F.,
 ( 4, 2, 4 ),
 ( 0.002739916521960775609, 0.004109700271224535871, 0.005479484020488295699 ),
 .UNSPECIFIED. ) ;
#71983 = CARTESIAN_POINT ( 'NONE',  ( -40.01351806051105342, -294.0187654585725454, -195.3961402325638517 ) ) ;
#71984 = CARTESIAN_POINT ( 'NONE',  ( -110.5448710370901040, -285.5219295795045582, -268.1921974500549481 ) ) ;
#71985 = CARTESIAN_POINT ( 'NONE',  ( 7.730752589637974737, -294.6656197581439187, -210.1421827852705633 ) ) ;
#71986 = CARTESIAN_POINT ( 'NONE',  ( 197.5277731218624524, 69.98851376389092138, -11.59179972303952866 ) ) ;
#71987 = LINE ( 'NONE', #14683, #67036 ) ;
#71988 = CARTESIAN_POINT ( 'NONE',  ( -92.94891957850609288, -275.2389527599934809, -219.4869315965473220 ) ) ;
#71989 = CARTESIAN_POINT ( 'NONE',  ( 33.11219503982915313, -281.0093767456083924, -290.0804075981376968 ) ) ;
#71990 = CARTESIAN_POINT ( 'NONE',  ( -32.02876435720155257, -280.9849457034831062, -345.1727037359891028 ) ) ;
#71991 = CARTESIAN_POINT ( 'NONE',  ( -53.26578666536293127, -294.4483887895736416, -345.5859034630552173 ) ) ;
#71992 = CARTESIAN_POINT ( 'NONE',  ( 5.785153532394141429, -272.8850983219649606, -210.1475440307942222 ) ) ;
#71993 = CARTESIAN_POINT ( 'NONE',  ( -97.26648212413840611, -276.0247988262237300, -314.5450866642938763 ) ) ;
#71994 = CARTESIAN_POINT ( 'NONE',  ( -63.26901759104931955, -299.0224993134086162, -201.5394178659348086 ) ) ;
#71995 = CARTESIAN_POINT ( 'NONE',  ( -29.87824091759911127, -272.7196098822664680, -194.3157166157376992 ) ) ;
#71996 = CARTESIAN_POINT ( 'NONE',  ( 35.87970261879645761, -294.8748380253817913, -262.5212469478725552 ) ) ;
#71997 = DIRECTION ( 'NONE',  ( 0.000000000000000000, 0.000000000000000000, 1.000000000000000000 ) ) ;
#71998 = CARTESIAN_POINT ( 'NONE',  ( 10.40461484679384263, -295.1757085248730164, -325.7947822380005505 ) ) ;
#71999 = FACE_OUTER_BOUND ( 'NONE', #27902, .T. ) ;
#72001 = CARTESIAN_POINT ( 'NONE',  ( -96.10032005947223865, -297.1595038245295086, -227.0222975241949541 ) ) ;
#72000 = CARTESIAN_POINT ( 'NONE',  ( -18.56692111267556200, -284.3127753800040409, -197.3283248519107929 ) ) ;
#72002 = CARTESIAN_POINT ( 'NONE',  ( -99.34424074211752043, -285.1597386703469397, -224.6150375898039329 ) ) ;
#72003 = CARTESIAN_POINT ( 'NONE',  ( 32.69455555656799106, -286.8089138047854476, -238.2849010246100363 ) ) ;
#72004 = CARTESIAN_POINT ( 'NONE',  ( 25.16186041069929047, -296.0986839325759092, -312.4528240888232062 ) ) ;
#72005 = CARTESIAN_POINT ( 'NONE',  ( 35.08894215874857991, -291.3097428907472590, -251.5507355454824108 ) ) ;
#72006 = EDGE_CURVE ( 'NONE', #54877, #83549, #57994, .T. ) ;
#72007 = CARTESIAN_POINT ( 'NONE',  ( -94.83416476701385989, -278.4414727312155833, -219.3829331338753263 ) ) ;
#72008 = ADVANCED_FACE ( 'NONE', ( #45720 ), #74630, .T. ) ;
#72009 = CARTESIAN_POINT ( 'NONE',  ( -37.30987171927208834, -283.5523547857346784, -195.3611179825600175 ) ) ;
#72010 = CARTESIAN_POINT ( 'NONE',  ( 208.4306832106270804, -125.2391364535880882, 0.000000000000000000 ) ) ;
#72011 = CARTESIAN_POINT ( 'NONE',  ( 25.29754418281599371, -285.8228712985219317, -232.1059800730079132 ) ) ;
#72012 = CARTESIAN_POINT ( 'NONE',  ( 199.5538737146232506, 67.40778408939276289, -8.432808456659151020 ) ) ;
#72013 = CARTESIAN_POINT ( 'NONE',  ( 215.9306832106270804, -148.7221692137691491, 9.184850993605173582E-16 ) ) ;
#72014 = CARTESIAN_POINT ( 'NONE',  ( -111.0395096149018315, -298.1016273590528272, -274.2435515210606809 ) ) ;
#72015 = CARTESIAN_POINT ( 'NONE',  ( -25.50490493817391169, -281.6254462949252115, -194.8727309868217503 ) ) ;
#72017 = CARTESIAN_POINT ( 'NONE',  ( 35.03278949103064832, -281.4214001322674221, -260.4493991356154083 ) ) ;
#72016 = CARTESIAN_POINT ( 'NONE',  ( -73.83245331181514359, -293.5539221253186497, -336.3500708814008817 ) ) ;
#72018 = CARTESIAN_POINT ( 'NONE',  ( -81.86997073787379975, -295.8067354970518181, -333.2452900623168830 ) ) ;
#72019 = CARTESIAN_POINT ( 'NONE',  ( -101.2383276382620636, -274.4748131363380139, -233.7538662865325136 ) ) ;
#72020 = CARTESIAN_POINT ( 'NONE',  ( -66.60618896100223196, -281.6689944610478733, -201.3061373944859156 ) ) ;
#72021 = CARTESIAN_POINT ( 'NONE',  ( -109.5056735946826336, -295.7750097042693369, -257.8803575086465116 ) ) ;
#72022 = VERTEX_POINT ( 'NONE', #1264 ) ;
#72023 = FACE_OUTER_BOUND ( 'NONE', #19612, .T. ) ;
#72024 = CARTESIAN_POINT ( 'NONE',  ( -34.76506622459292828, -284.9995455357266110, -344.9741545967229399 ) ) ;
#72025 = CARTESIAN_POINT ( 'NONE',  ( 160.5350683151633291, 276.0000000000000568, 24.72542485937379197 ) ) ;
#72026 = CARTESIAN_POINT ( 'NONE',  ( -69.85430415644619018, -283.1237833571632336, -202.7746430608542312 ) ) ;
#72027 = CARTESIAN_POINT ( 'NONE',  ( 32.41078021772341344, -274.3346903715184908, -238.0047266940846953 ) ) ;
#72028 = CARTESIAN_POINT ( 'NONE',  ( -28.10424422201742800, -292.0058468812596857, -197.8971842642352783 ) ) ;
#72029 = CARTESIAN_POINT ( 'NONE',  ( 28.78165832251644218, -283.5103397503215774, -303.0101868851732547 ) ) ;
#72030 = VECTOR ( 'NONE', #46261, 1000.000000000000114 ) ;
#72031 = CARTESIAN_POINT ( 'NONE',  ( 35.41089927456891218, -276.9896402802463058, -257.8966782738378356 ) ) ;
#72032 = CARTESIAN_POINT ( 'NONE',  ( 32.83718764427325709, -283.5356054391248222, -300.1837324166258441 ) ) ;
#72033 = CARTESIAN_POINT ( 'NONE',  ( 19.65070171970234014, -280.9981525836967649, -316.6302118931899940 ) ) ;
#72034 = CARTESIAN_POINT ( 'NONE',  ( -109.9141424287481215, -280.7961214337716456, -251.3833419120509802 ) ) ;
#72035 = CARTESIAN_POINT ( 'NONE',  ( -30.48458194015535838, -298.1357836350427419, -193.3611176790317074 ) ) ;
#72036 = CARTESIAN_POINT ( 'NONE',  ( 39.55446787631457539, -275.3239508089454830, -265.4418929110120189 ) ) ;
#72037 = CARTESIAN_POINT ( 'NONE',  ( 35.35080722273567488, -295.2641107008909103, -254.2675017003034839 ) ) ;
#72038 = DIRECTION ( 'NONE',  ( 0.000000000000000000, 0.000000000000000000, 1.000000000000000000 ) ) ;
#72039 = DIRECTION ( 'NONE',  ( 0.000000000000000000, 0.000000000000000000, 1.000000000000000000 ) ) ;
#72040 = CARTESIAN_POINT ( 'NONE',  ( -5.050829660353836736, -292.7712104210492612, -338.9144308581992959 ) ) ;
#72041 = CARTESIAN_POINT ( 'NONE',  ( -46.18001305785128352, -273.4446554223143835, -197.8361383814520309 ) ) ;
#72042 = CARTESIAN_POINT ( 'NONE',  ( -14.09625302340793418, -293.8683044725487434, -197.6258270216233939 ) ) ;
#72044 = CARTESIAN_POINT ( 'NONE',  ( -58.84201449618048230, -292.9851042784021615, -196.8373449585159278 ) ) ;
#72043 = CARTESIAN_POINT ( 'NONE',  ( 21.27581636871892101, -283.4090924074130839, -223.5744983911110353 ) ) ;
#72045 = CARTESIAN_POINT ( 'NONE',  ( -34.48307862508264776, -291.0164376147766347, -345.1906619236081042 ) ) ;
#72046 = CARTESIAN_POINT ( 'NONE',  ( -88.36366393943762887, -275.7689532936446426, -325.1040411158176653 ) ) ;
#72047 = CARTESIAN_POINT ( 'NONE',  ( -35.04926656989797351, -278.9432927561168185, -344.7658150714715930 ) ) ;
#72048 = CARTESIAN_POINT ( 'NONE',  ( 15.31800204115145547, -292.3814875157432311, -323.0479202010999416 ) ) ;
#72049 = CARTESIAN_POINT ( 'NONE',  ( 14.91893594893046426, -284.1850968029752380, -325.2166682538226610 ) ) ;
#72050 = CARTESIAN_POINT ( 'NONE',  ( -109.9163088430971129, -283.6084530073849237, -260.0096811946550019 ) ) ;
#72051 = ORIENTED_EDGE ( 'NONE', *, *, #64191, .F. ) ;
#72052 = CARTESIAN_POINT ( 'NONE',  ( 7.803703418024110050, -282.0829779783930462, -327.8188973778915738 ) ) ;
#72053 = CARTESIAN_POINT ( 'NONE',  ( -8.988225947576655273, -281.4941050074010036, -199.1040270246605814 ) ) ;
#72054 = CARTESIAN_POINT ( 'NONE',  ( -106.6529233668657497, -282.9271153624624162, -302.9795644600513356 ) ) ;
#72055 = CARTESIAN_POINT ( 'NONE',  ( -108.2997405067442429, -279.8667756047477724, -241.0732925599855321 ) ) ;
#72056 = CARTESIAN_POINT ( 'NONE',  ( -25.85505919037385425, -278.4285036815351759, -345.7982761425820968 ) ) ;
#72057 = CARTESIAN_POINT ( 'NONE',  ( -82.08285599513421005, -298.1948066931273615, -326.5171145203363494 ) ) ;
#72058 = VERTEX_POINT ( 'NONE', #59975 ) ;
#72059 = CARTESIAN_POINT ( 'NONE',  ( -94.32598840690097575, -275.2254758088072890, -221.8354602036058338 ) ) ;
#72060 = CARTESIAN_POINT ( 'NONE',  ( -93.99100174651738371, -275.8955222071638218, -318.9687658516154443 ) ) ;
#72061 = CARTESIAN_POINT ( 'NONE',  ( -105.1106540324819036, -292.7619993617021805, -235.8743658751812973 ) ) ;
#72062 = CARTESIAN_POINT ( 'NONE',  ( 24.50908012278991777, -293.4393963967647210, -309.4225019919180681 ) ) ;
#72063 = CARTESIAN_POINT ( 'NONE',  ( -75.63849464279904566, -289.0566755653645714, -337.0910395556628032 ) ) ;
#72064 = DIRECTION ( 'NONE',  ( -0.000000000000000000, -1.000000000000000000, -0.000000000000000000 ) ) ;
#72066 = CARTESIAN_POINT ( 'NONE',  ( -19.60405935796048027, -284.6839469424128879, -198.7244198946049210 ) ) ;
#72065 = CARTESIAN_POINT ( 'NONE',  ( 38.23108079138106064, -292.2691119007565135, -281.6465544832571481 ) ) ;
#72067 = CARTESIAN_POINT ( 'NONE',  ( -58.02137488133270438, -293.6427136461132363, -199.0106616299309223 ) ) ;
#72068 = CARTESIAN_POINT ( 'NONE',  ( -35.90068164768727144, -284.5504271968976582, -196.6818724648418026 ) ) ;
#72069 = CARTESIAN_POINT ( 'NONE',  ( 14.28293525582184564, -283.6235352786957264, -322.7409180634737709 ) ) ;
#72070 = CARTESIAN_POINT ( 'NONE',  ( -59.94651908012836117, -290.2793647248366824, -343.7221592277097102 ) ) ;
#72071 = CARTESIAN_POINT ( 'NONE',  ( 31.12577768059959737, -281.7029552731623880, -244.7171264559154338 ) ) ;
#72072 = CARTESIAN_POINT ( 'NONE',  ( 19.22604116101428673, -293.0537110175874318, -322.0920100187227604 ) ) ;
#72073 = CARTESIAN_POINT ( 'NONE',  ( -23.33132271493577647, -289.6803567608358208, -345.9655546087703328 ) ) ;
#72074 = ADVANCED_FACE ( 'NONE', ( #39078 ), #3562, .F. ) ;
#72075 = CARTESIAN_POINT ( 'NONE',  ( -82.81122626075774917, -290.1479625329168925, -332.4259961048541072 ) ) ;
#72076 = CARTESIAN_POINT ( 'NONE',  ( -108.3660055645780744, -284.9420133606111563, -253.4387241064036118 ) ) ;
#72077 = ORIENTED_EDGE ( 'NONE', *, *, #92813, .T. ) ;
#72078 = CARTESIAN_POINT ( 'NONE',  ( 195.9076712334997694, 25.46858585516271845, 12.18710226207752712 ) ) ;
#72079 = CARTESIAN_POINT ( 'NONE',  ( 20.44122463352771035, -296.0838475890648169, -319.3655982784746925 ) ) ;
#72080 = CARTESIAN_POINT ( 'NONE',  ( -104.1802850471923989, -294.7500243254506245, -307.6971628235469893 ) ) ;
#72081 = CARTESIAN_POINT ( 'NONE',  ( -96.58902260927307282, -278.2114451816100882, -227.3127355810333938 ) ) ;
#72082 = CARTESIAN_POINT ( 'NONE',  ( -78.80311177904566478, -273.0169954203856832, -205.5500213474510929 ) ) ;
#72083 = CARTESIAN_POINT ( 'NONE',  ( -80.57704693125474193, -294.1303770366412778, -330.0386894608332113 ) ) ;
#72084 = CARTESIAN_POINT ( 'NONE',  ( 31.22514465699807573, -277.6820633777243188, -298.3644491461026291 ) ) ;
#72085 = CARTESIAN_POINT ( 'NONE',  ( -108.3715727417624777, -270.9747709077365130, -248.6069281272188505 ) ) ;
#72086 = CARTESIAN_POINT ( 'NONE',  ( 31.91983378390802173, -295.0804446200519919, -294.8026977361891454 ) ) ;
#72087 = CARTESIAN_POINT ( 'NONE',  ( -71.06079061321462120, -296.5877362488466815, -335.4693154410733200 ) ) ;
#72088 = CARTESIAN_POINT ( 'NONE',  ( -108.1158907659633996, -294.8793984399376882, -245.0423035400979472 ) ) ;
#72089 = CARTESIAN_POINT ( 'NONE',  ( 53.42971810148159761, -299.8120856905852065, -193.4532684622509180 ) ) ;
#72090 = CARTESIAN_POINT ( 'NONE',  ( -33.97572615395107931, -276.0946628083879659, -195.4366835832176150 ) ) ;
#72091 = CARTESIAN_POINT ( 'NONE',  ( -74.82606945250284980, -290.5056965738940562, -333.2911152893400413 ) ) ;
#72092 = CARTESIAN_POINT ( 'NONE',  ( -108.0234513516876405, -273.4334574445227872, -239.8352910743383575 ) ) ;
#72093 = CARTESIAN_POINT ( 'NONE',  ( -26.19999564173576800, -295.2396752348956284, -342.5272451326647456 ) ) ;
#72094 = EDGE_CURVE ( 'NONE', #4814, #48695, #59477, .T. ) ;
#72095 = CARTESIAN_POINT ( 'NONE',  ( -112.5703135575944316, -280.5878421184739864, -265.9950531963937692 ) ) ;
#72096 = CARTESIAN_POINT ( 'NONE',  ( -69.73821498184940992, -278.3193582752171551, -201.0376299117948804 ) ) ;
#72097 = CARTESIAN_POINT ( 'NONE',  ( -47.25145265047196119, -282.5235153986121759, -346.6179838461253553 ) ) ;
#72098 = CARTESIAN_POINT ( 'NONE',  ( 22.68399703883054030, -274.2558517652779528, -222.2753977917737416 ) ) ;
#72099 = CARTESIAN_POINT ( 'NONE',  ( -84.06021005979886240, -277.8224186699837333, -210.0961750148686349 ) ) ;
#72100 = CARTESIAN_POINT ( 'NONE',  ( -36.74099793837045524, -278.0595291237798392, -195.1841118836794067 ) ) ;
#72101 = CARTESIAN_POINT ( 'NONE',  ( -34.43878961313275511, -296.7740619526214232, -196.8686294547052569 ) ) ;
#72102 = CARTESIAN_POINT ( 'NONE',  ( 37.17243969616534827, -277.4372861856307395, -261.4024133701462915 ) ) ;
#72103 = DIRECTION ( 'NONE',  ( -1.000000000000000000, -0.000000000000000000, -0.000000000000000000 ) ) ;
#72104 = CARTESIAN_POINT ( 'NONE',  ( -9.103671700846375003, -290.4396919338562952, -200.4968169823320352 ) ) ;
#72105 = CARTESIAN_POINT ( 'NONE',  ( -69.62316028454603156, -291.6388648731768285, -200.4403581354582968 ) ) ;
#72106 = CARTESIAN_POINT ( 'NONE',  ( -68.11731033356453224, -275.6491723209145448, -201.7694409521948558 ) ) ;
#72107 = CARTESIAN_POINT ( 'NONE',  ( -109.8677007266892076, -270.7998507818898588, -251.0577745248691599 ) ) ;
#72108 = EDGE_CURVE ( 'NONE', #84479, #5104, #83085, .T. ) ;
#72109 = CARTESIAN_POINT ( 'NONE',  ( -113.3261760821276596, -283.8968945801153723, -258.5861112596620046 ) ) ;
#72110 = CARTESIAN_POINT ( 'NONE',  ( 209.9779462868543760, 37.90836112277824554, 13.95111757441427258 ) ) ;
#72111 = CARTESIAN_POINT ( 'NONE',  ( -86.78430732134359005, -283.3648139544016544, -213.8977631919859448 ) ) ;
#72112 = DIRECTION ( 'NONE',  ( -1.000000000000000000, 0.000000000000000000, 0.000000000000000000 ) ) ;
#72113 = CARTESIAN_POINT ( 'NONE',  ( -12.10936487513805560, -291.1827287707544656, -201.3833634643218602 ) ) ;
#72114 = CARTESIAN_POINT ( 'NONE',  ( -52.31531814145177606, -283.9979545309563491, -197.6517221586202595 ) ) ;
#72115 = DIRECTION ( 'NONE',  ( 0.000000000000000000, 1.000000000000000000, 0.000000000000000000 ) ) ;
#72116 = CARTESIAN_POINT ( 'NONE',  ( 113.5000000000000568, -212.3147208684173677, -516.1047766808072765 ) ) ;
#72117 = CARTESIAN_POINT ( 'NONE',  ( 22.91862670923142886, -292.1613886544911907, -315.0119148497878996 ) ) ;
#72118 = CARTESIAN_POINT ( 'NONE',  ( -113.1287578992756266, -283.1442229707908496, -261.4712571083671264 ) ) ;
#72119 = CARTESIAN_POINT ( 'NONE',  ( -95.06616654416247059, -279.5097037708815151, -316.3631023532406630 ) ) ;
#72120 = CARTESIAN_POINT ( 'NONE',  ( -108.9263851094585362, -285.4085708248432525, -297.7786406815976079 ) ) ;
#72121 = CARTESIAN_POINT ( 'NONE',  ( 33.38856281973362883, -287.3131462519596084, -252.2488282641054980 ) ) ;
#72122 = CARTESIAN_POINT ( 'NONE',  ( -85.47706236587302442, -279.1580606253975247, -326.0915339580321870 ) ) ;
#72123 = CARTESIAN_POINT ( 'NONE',  ( -100.9572441311622981, -279.8487660301154847, -234.2271410665883877 ) ) ;
#72124 = CARTESIAN_POINT ( 'NONE',  ( -21.35796284116707966, -288.2360637772588916, -196.7205928480166790 ) ) ;
#72125 = VERTEX_POINT ( 'NONE', #52836 ) ;
#72126 = CARTESIAN_POINT ( 'NONE',  ( 7.991229253068932614, -298.4383658456491730, -193.3623461297880226 ) ) ;
#72127 = CARTESIAN_POINT ( 'NONE',  ( -20.73952784644652070, -290.8178684932008196, -343.1362145134649495 ) ) ;
#72128 = CARTESIAN_POINT ( 'NONE',  ( 197.3235832258322375, 41.90495390785805796, 12.40447841451800848 ) ) ;
#72129 = CARTESIAN_POINT ( 'NONE',  ( -115.3430155898818299, -287.2662352645559167, -252.5904736702033517 ) ) ;
#72130 = ORIENTED_EDGE ( 'NONE', *, *, #81029, .F. ) ;
#72131 = CARTESIAN_POINT ( 'NONE',  ( 20.74446902344014632, -292.6238628041645029, -319.6808642372171789 ) ) ;
#72132 = CARTESIAN_POINT ( 'NONE',  ( 11.58000868160295127, -288.2653677199208460, -215.1801947130151405 ) ) ;
#72133 = CARTESIAN_POINT ( 'NONE',  ( -19.30906643256497546, -282.0473460733831530, -198.5251132865508623 ) ) ;
#72134 = CARTESIAN_POINT ( 'NONE',  ( 25.05338678105322359, -288.3889508617324395, -226.2312038807338013 ) ) ;
#72135 = CARTESIAN_POINT ( 'NONE',  ( 32.42209717841763705, -289.2710504435426628, -301.7667043778193943 ) ) ;
#72136 = CARTESIAN_POINT ( 'NONE',  ( -67.33667069520981840, -285.4456307096435808, -339.1158932400369395 ) ) ;
#72137 = CARTESIAN_POINT ( 'NONE',  ( -109.7360357469265182, -278.3857713052277632, -296.7479835589050481 ) ) ;
#72138 = EDGE_LOOP ( 'NONE', ( #77767, #51765, #79912, #14666 ) ) ;
#72139 = CARTESIAN_POINT ( 'NONE',  ( 16.51762841623082068, -292.3741761567443973, -323.4306708985980663 ) ) ;
#72140 = CARTESIAN_POINT ( 'NONE',  ( 19.16160386343882038, -280.6729170352049891, -218.0507304620034006 ) ) ;
#72141 = CARTESIAN_POINT ( 'NONE',  ( -86.13965362379038027, -275.2278293405495333, -214.3495325486017293 ) ) ;
#72142 = CARTESIAN_POINT ( 'NONE',  ( 10.64812456238590066, -290.9090924074130839, -330.4860931364851808 ) ) ;
#72143 = CARTESIAN_POINT ( 'NONE',  ( -5.517966667665570313, -272.7049106162600651, -201.3594947734044638 ) ) ;
#72144 = FACE_OUTER_BOUND ( 'NONE', #71344, .T. ) ;
#72145 = CARTESIAN_POINT ( 'NONE',  ( -22.17551659206192838, -279.7592038649978576, -198.8391152777686557 ) ) ;
#72146 = CARTESIAN_POINT ( 'NONE',  ( 37.55390969369304344, -276.5542630946214331, -254.2163673217129372 ) ) ;
#72147 = CARTESIAN_POINT ( 'NONE',  ( -82.31847732346159319, -298.8501617088954276, -212.0516574874254445 ) ) ;
#72148 = CARTESIAN_POINT ( 'NONE',  ( -13.50640716079615267, -281.8088008064682981, -343.3316532805359316 ) ) ;
#72149 = CARTESIAN_POINT ( 'NONE',  ( -93.33763987949404850, -292.9924453883014621, -221.9624739252059271 ) ) ;
#72150 = CARTESIAN_POINT ( 'NONE',  ( -92.60614567709042433, -274.8769020882753011, -217.8798799866181923 ) ) ;
#72151 = CARTESIAN_POINT ( 'NONE',  ( -20.63312189431888299, -299.4620382776674319, -193.7548524899362974 ) ) ;
#72152 = CARTESIAN_POINT ( 'NONE',  ( 36.71857844773398227, -295.4142531729041821, -259.6324850765803376 ) ) ;
#72153 = CARTESIAN_POINT ( 'NONE',  ( -106.9278959403439870, -282.1911459951321035, -298.0302777590979986 ) ) ;
#72154 = CARTESIAN_POINT ( 'NONE',  ( -101.6639569753313310, -290.7760345106847808, -227.9760924588899798 ) ) ;
#72155 = CARTESIAN_POINT ( 'NONE',  ( -93.23337476386113565, -271.2636306261364325, -220.8841788005876197 ) ) ;
#72156 = CARTESIAN_POINT ( 'NONE',  ( -40.80076927130045306, -287.6095817238835366, -194.1880173347707341 ) ) ;
#72157 = CARTESIAN_POINT ( 'NONE',  ( -75.12719568111137391, -290.4565565351510941, -207.4808241759919269 ) ) ;
#72158 = VERTEX_POINT ( 'NONE', #23027 ) ;
#72159 = CARTESIAN_POINT ( 'NONE',  ( -93.17475775510396829, -288.4093747830734742, -322.6032448801970531 ) ) ;
#72160 = CARTESIAN_POINT ( 'NONE',  ( -61.26594495987933442, -289.0382953878480521, -339.3518274728278357 ) ) ;
#72161 = ORIENTED_EDGE ( 'NONE', *, *, #28909, .F. ) ;
#72162 = CARTESIAN_POINT ( 'NONE',  ( -64.45083892249839153, -286.7861564909559320, -198.6072883698452927 ) ) ;
#72163 = CARTESIAN_POINT ( 'NONE',  ( -93.61961422051079751, -278.2258150813962629, -316.9090201112134650 ) ) ;
#72164 = CARTESIAN_POINT ( 'NONE',  ( 10.93491539985237893, -291.6222251664050304, -210.7036837983360726 ) ) ;
#72165 = CARTESIAN_POINT ( 'NONE',  ( -95.25249656028125855, -284.5183881449053160, -320.9541258333605356 ) ) ;
#72166 = CARTESIAN_POINT ( 'NONE',  ( -113.7991315765020772, -284.9973273255151298, -261.4165404187135664 ) ) ;
#72167 = CARTESIAN_POINT ( 'NONE',  ( -62.32016810646861416, -280.0515117301268901, -201.6916843282011484 ) ) ;
#72168 = CARTESIAN_POINT ( 'NONE',  ( -12.65737504837112404, -91.72627791072594050, -360.1682197548814202 ) ) ;
#72169 = CARTESIAN_POINT ( 'NONE',  ( 137.7092865063222575, 180.7388654737660829, -240.7682804503873797 ) ) ;
#72170 = CARTESIAN_POINT ( 'NONE',  ( 44.12421593066579106, 11.81245027319820196, -328.6256852122805867 ) ) ;
#72171 = CARTESIAN_POINT ( 'NONE',  ( -83.28406724776048975, -272.6009407282153916, -213.4234272157443115 ) ) ;
#72172 = CARTESIAN_POINT ( 'NONE',  ( 21.73841949090026660, -273.8669598924385014, -226.9587500736770096 ) ) ;
#72173 = CARTESIAN_POINT ( 'NONE',  ( -61.57813148803720082, -294.8663075684704040, -343.4381965951935740 ) ) ;
#72174 = CARTESIAN_POINT ( 'NONE',  ( -92.86534849868182562, -239.6190322135574604, -339.0248232835550652 ) ) ;
#72175 = CARTESIAN_POINT ( 'NONE',  ( -21.44083504604207135, -272.9367847985587332, -195.5248917209902118 ) ) ;
#72176 = CARTESIAN_POINT ( 'NONE',  ( -36.48891269409420346, -299.9233529725826770, -196.1256365755298248 ) ) ;
#72177 = CARTESIAN_POINT ( 'NONE',  ( -3.121925690105149975, -289.9057000701648690, -335.4578648123214180 ) ) ;
#72178 = ORIENTED_EDGE ( 'NONE', *, *, #32846, .F. ) ;
#72179 = CARTESIAN_POINT ( 'NONE',  ( 21.19602096002916269, -295.1648322703576923, -320.0215189419722037 ) ) ;
#72180 = CARTESIAN_POINT ( 'NONE',  ( -60.00366422690770918, -286.2427252602014960, -200.9030455593933482 ) ) ;
#72181 = CARTESIAN_POINT ( 'NONE',  ( -100.9444605425184704, -272.0403866702864093, -227.4159127912577958 ) ) ;
#72182 = CARTESIAN_POINT ( 'NONE',  ( 38.65834229362575059, -294.4968572137112801, -281.6815584508277652 ) ) ;
#72183 = CARTESIAN_POINT ( 'NONE',  ( -105.9000167581246927, -296.5931517407428828, -305.3967080702572616 ) ) ;
#72184 = CARTESIAN_POINT ( 'NONE',  ( -108.7110157719450001, -290.9212379986113319, -255.0176897782157539 ) ) ;
#72185 = ORIENTED_EDGE ( 'NONE', *, *, #46507, .T. ) ;
#72186 = CARTESIAN_POINT ( 'NONE',  ( -84.92079890458373370, -275.3217943752956671, -211.6623653999179453 ) ) ;
#72187 = CARTESIAN_POINT ( 'NONE',  ( 34.82171282160243919, -274.6748853042140013, -296.2166109889252539 ) ) ;
#72188 = ORIENTED_EDGE ( 'NONE', *, *, #55616, .F. ) ;
#72189 = CARTESIAN_POINT ( 'NONE',  ( -109.6810496182796300, -277.7268502464187918, -296.7190168683673619 ) ) ;
#72190 = CARTESIAN_POINT ( 'NONE',  ( 36.14881875116507359, -274.0401164478188321, -277.1127140063403544 ) ) ;
#72191 = CARTESIAN_POINT ( 'NONE',  ( -64.69684565372234886, -274.7660610395514595, -202.3334482827306715 ) ) ;
#72192 = CARTESIAN_POINT ( 'NONE',  ( 25.47149148025363985, -275.9759358689927922, -232.6077533692073871 ) ) ;
#72193 = CARTESIAN_POINT ( 'NONE',  ( 35.60663071739295304, -277.0398496886527369, -248.9050339979837361 ) ) ;
#72194 = CARTESIAN_POINT ( 'NONE',  ( 32.64702206594044043, -273.9359372376582655, -298.4299030441207492 ) ) ;
#72195 = CARTESIAN_POINT ( 'NONE',  ( -5.489605120973596541, -295.2731202430690587, -336.1726441367379152 ) ) ;
#72196 = CARTESIAN_POINT ( 'NONE',  ( -35.65516140443621396, -293.6053406829528285, -343.9436173441469009 ) ) ;
#72197 = CARTESIAN_POINT ( 'NONE',  ( 0.000000000000000000, 3.000000000000000000, -9.000000000000001776 ) ) ;
#72198 = CARTESIAN_POINT ( 'NONE',  ( -82.20805887752608498, -279.9503500644127030, -207.8588239795570587 ) ) ;
#72199 = CARTESIAN_POINT ( 'NONE',  ( 0.8732352476282526643, -276.6939008672684395, -332.6187364180840405 ) ) ;
#72200 = CARTESIAN_POINT ( 'NONE',  ( -46.43019579271401653, -284.6239346561618504, -194.3960107384411629 ) ) ;
#72201 = CARTESIAN_POINT ( 'NONE',  ( -71.22427780113663687, -297.4985909101912966, -337.4580580063670254 ) ) ;
#72202 = DIRECTION ( 'NONE',  ( 0.000000000000000000, 0.000000000000000000, 1.000000000000000000 ) ) ;
#72203 = CARTESIAN_POINT ( 'NONE',  ( 35.71455348921347195, -286.6864663648976261, -265.5863291493671454 ) ) ;
#72204 = EDGE_CURVE ( 'NONE', #63355, #6488, #2081, .T. ) ;
#72205 = CARTESIAN_POINT ( 'NONE',  ( -69.71460270213881927, -275.7241295772534500, -336.9331624954579638 ) ) ;
#72206 = CARTESIAN_POINT ( 'NONE',  ( -110.9816351847938307, -277.1234559487222668, -270.6221747619007942 ) ) ;
#72207 = CARTESIAN_POINT ( 'NONE',  ( -111.9586348641968243, -286.4487947236958689, -278.4235455609854171 ) ) ;
#72208 = CARTESIAN_POINT ( 'NONE',  ( -32.37846152274660483, -278.1934021981566616, -343.6404262525761055 ) ) ;
#72209 = FACE_OUTER_BOUND ( 'NONE', #83422, .T. ) ;
#72210 = CARTESIAN_POINT ( 'NONE',  ( 23.71430784749315279, -274.5649275561231661, -315.9528311257732867 ) ) ;
#72211 = CARTESIAN_POINT ( 'NONE',  ( 35.12045750345512118, -276.0764425751135036, -260.7108133468422011 ) ) ;
#72212 = CARTESIAN_POINT ( 'NONE',  ( 26.28556427364415526, -283.0143621062061356, -230.2436344752042032 ) ) ;
#72213 = DIRECTION ( 'NONE',  ( -0.000000000000000000, -0.000000000000000000, -1.000000000000000000 ) ) ;
#72214 = CARTESIAN_POINT ( 'NONE',  ( 9.357531784683576603, -290.3366721901008987, -329.8288423934346838 ) ) ;
#72215 = CARTESIAN_POINT ( 'NONE',  ( 13.21780444310662261, -290.7583603155152332, -214.8954347324663274 ) ) ;
#72216 = DIRECTION ( 'NONE',  ( 0.000000000000000000, 1.000000000000000000, 0.000000000000000000 ) ) ;
#72217 = CARTESIAN_POINT ( 'NONE',  ( -107.6635277046676578, -271.5199248403631032, -248.8308006682090365 ) ) ;
#72218 = CARTESIAN_POINT ( 'NONE',  ( -108.5739573580552957, -288.9641819618393583, -249.4155292926967320 ) ) ;
#72219 = CARTESIAN_POINT ( 'NONE',  ( -92.95696114837319612, -243.2523998898738569, -344.1903318997441374 ) ) ;
#72220 = DIRECTION ( 'NONE',  ( 1.000000000000000000, 0.000000000000000000, 0.000000000000000000 ) ) ;
#72221 = CARTESIAN_POINT ( 'NONE',  ( -111.8921524909754339, -288.8266219521386233, -286.6380282534744879 ) ) ;
#72222 = CARTESIAN_POINT ( 'NONE',  ( -109.7606390010757025, -285.9668556064560789, -284.5715968414907024 ) ) ;
#72223 = CARTESIAN_POINT ( 'NONE',  ( -113.3273347366348816, -282.7970378597454442, -269.9644513511321406 ) ) ;
#72224 = EDGE_CURVE ( 'NONE', #26503, #23662, #91675, .T. ) ;
#72225 = CARTESIAN_POINT ( 'NONE',  ( 12.32765385669209302, -283.7694257046418329, -324.6596464212620390 ) ) ;
#72226 = CARTESIAN_POINT ( 'NONE',  ( -100.5354780182555459, -284.8501155841900072, -307.2277446602610098 ) ) ;
#72227 = CARTESIAN_POINT ( 'NONE',  ( -103.1853014058950606, -293.0174815337820178, -233.7137855962563719 ) ) ;
#72228 = CARTESIAN_POINT ( 'NONE',  ( 7.219291916388593577, -274.9740221839773540, -207.5257884956481576 ) ) ;
#72229 = CARTESIAN_POINT ( 'NONE',  ( -110.9095401712133935, -288.8516815247767227, -253.1249027969321048 ) ) ;
#72230 = CARTESIAN_POINT ( 'NONE',  ( -87.09519316048870508, -277.7227055379217973, -329.1981338466251827 ) ) ;
#72231 = CARTESIAN_POINT ( 'NONE',  ( -12.43620591708766909, -296.7066756333763919, -340.7829283047855711 ) ) ;
#72232 = DIRECTION ( 'NONE',  ( 0.000000000000000000, 0.000000000000000000, 1.000000000000000000 ) ) ;
#72233 = CARTESIAN_POINT ( 'NONE',  ( -95.95921662488163406, -298.4090924074130271, -317.1477375740089997 ) ) ;
#72234 = CARTESIAN_POINT ( 'NONE',  ( -93.81167255414798944, -282.5740673866115458, -317.3971222088090371 ) ) ;
#72235 = CARTESIAN_POINT ( 'NONE',  ( -94.36808371056892497, -277.2268040624016407, -221.6280328345879980 ) ) ;
#72236 = CARTESIAN_POINT ( 'NONE',  ( -93.62070480235979630, -271.7395035847036411, -218.8114385640503201 ) ) ;
#72237 = CARTESIAN_POINT ( 'NONE',  ( 22.54457857065109039, -275.4856188734532907, -312.3708708256971249 ) ) ;
#72238 = CARTESIAN_POINT ( 'NONE',  ( -65.61065908443198680, -293.1957805189775286, -202.2918073840752982 ) ) ;
#72239 = CARTESIAN_POINT ( 'NONE',  ( 34.94425714589072385, -294.3378254519152506, -258.5291048010317354 ) ) ;
#72240 = CARTESIAN_POINT ( 'NONE',  ( 15.15256291725693139, -295.6446606146163276, -326.0176595489072611 ) ) ;
#72241 = CARTESIAN_POINT ( 'NONE',  ( -103.7177047210294774, -296.7967053436346987, -239.8548220827740352 ) ) ;
#72242 = CARTESIAN_POINT ( 'NONE',  ( -34.47676895978258926, -291.0164376166588340, -345.3573223174328177 ) ) ;
#72243 = CARTESIAN_POINT ( 'NONE',  ( -24.53149152632248686, -283.0598036046549737, -346.3421632552261826 ) ) ;
#72244 = CARTESIAN_POINT ( 'NONE',  ( -46.70449181843956410, -272.0740742925664222, -195.1770531096858861 ) ) ;
#72245 = CARTESIAN_POINT ( 'NONE',  ( 39.60421368790518670, -287.4362975898073387, -274.4250517750303402 ) ) ;
#72246 = CARTESIAN_POINT ( 'NONE',  ( -88.19814173176044392, -279.7483649707896234, -325.0005647948572118 ) ) ;
#72247 = CARTESIAN_POINT ( 'NONE',  ( -62.63291473737278636, -284.7736471099571531, -201.5774035098777972 ) ) ;
#72248 = CARTESIAN_POINT ( 'NONE',  ( -0.2914747910911555939, -286.5597075694872728, -335.6293159690200696 ) ) ;
#72249 = CARTESIAN_POINT ( 'NONE',  ( 168.1488725781630649, 234.1813984995739588, -193.4213935641190858 ) ) ;
#72250 = CARTESIAN_POINT ( 'NONE',  ( -107.8221751442056444, -283.8051593440850979, -289.6565123486637390 ) ) ;
#72251 = CARTESIAN_POINT ( 'NONE',  ( 21.65503192903580754, -282.0969594670625611, -221.5001486240920769 ) ) ;
#72252 = CARTESIAN_POINT ( 'NONE',  ( -9.659396615061330849, -287.7579253121039642, -341.9607708109615487 ) ) ;
#72253 = CARTESIAN_POINT ( 'NONE',  ( -69.64200290103747193, -281.2341882915895326, -201.3314374808650769 ) ) ;
#72254 = CARTESIAN_POINT ( 'NONE',  ( -109.1491771156735240, -280.2048636172129932, -243.8076120735747168 ) ) ;
#72255 = CARTESIAN_POINT ( 'NONE',  ( -85.48258965898659767, -279.1974590404680612, -215.4843946869900151 ) ) ;
#72256 = CARTESIAN_POINT ( 'NONE',  ( -57.32568297988208883, -275.7730335748682364, -198.3872028591245567 ) ) ;
#72257 = CARTESIAN_POINT ( 'NONE',  ( 38.32523786283130107, -293.3737380188479733, -256.0952673216502262 ) ) ;
#72258 = CARTESIAN_POINT ( 'NONE',  ( 34.66194084949533760, -285.8287690258733846, -290.2331922916596909 ) ) ;
#72259 = CARTESIAN_POINT ( 'NONE',  ( 8.354722956675544765, -294.2656520259033073, -209.3175969661433271 ) ) ;
#72260 = CARTESIAN_POINT ( 'NONE',  ( -93.32732666391014220, -294.8025412396413572, -317.7074719879774989 ) ) ;
#72261 = CARTESIAN_POINT ( 'NONE',  ( -36.14635901347068625, -284.9572025038203833, -344.7915241410474891 ) ) ;
#72262 = CARTESIAN_POINT ( 'NONE',  ( -53.15809115742599289, -294.9271576280351610, -341.7007697881484205 ) ) ;
#72263 = CARTESIAN_POINT ( 'NONE',  ( -95.43579444196572581, -292.3107578065699954, -220.2753969559761629 ) ) ;
#72264 = CARTESIAN_POINT ( 'NONE',  ( 11.36757677955011836, -281.4003875513156459, -215.8514948777255995 ) ) ;
#72265 = CARTESIAN_POINT ( 'NONE',  ( -112.2111373206284384, -271.8235697714506500, -253.4086081768912493 ) ) ;
#72266 = CARTESIAN_POINT ( 'NONE',  ( -34.66205487393217766, -289.6707164229902673, -347.2124828903785101 ) ) ;
#72267 = CARTESIAN_POINT ( 'NONE',  ( -109.0631639589167037, -282.3790468691072419, -294.7811324298340878 ) ) ;
#72268 = CARTESIAN_POINT ( 'NONE',  ( 17.78936521832414641, -287.2030237710941947, -222.4794605279162738 ) ) ;
#72269 = DIRECTION ( 'NONE',  ( 0.000000000000000000, -0.000000000000000000, 1.000000000000000000 ) ) ;
#72270 = CARTESIAN_POINT ( 'NONE',  ( -23.57028549459368350, -107.7374504296638662, -360.4863739655157815 ) ) ;
#72271 = CARTESIAN_POINT ( 'NONE',  ( 25.36017924250387878, -24.03642681077339915, -341.3531356295546288 ) ) ;
#72272 = CARTESIAN_POINT ( 'NONE',  ( -106.5942687000072056, -278.0640325335781995, -246.6114683452737495 ) ) ;
#72273 = CARTESIAN_POINT ( 'NONE',  ( 7.341573138019706235, -279.5977177848541260, -212.1794895625533002 ) ) ;
#72274 = CARTESIAN_POINT ( 'NONE',  ( 38.47202511600811903, -275.0510172371289173, -256.9432352617927222 ) ) ;
#72275 = CARTESIAN_POINT ( 'NONE',  ( -109.2277675425154229, -270.7592608887684946, -295.7727018951397326 ) ) ;
#72276 = CARTESIAN_POINT ( 'NONE',  ( -31.10362161087083166, -278.7040981735294736, -194.1531172460235837 ) ) ;
#72277 = CARTESIAN_POINT ( 'NONE',  ( -59.45901281187757093, -281.3599024980197782, -341.7083188862335419 ) ) ;
#72278 = CARTESIAN_POINT ( 'NONE',  ( -80.07392774482289610, -299.2430099015089695, -207.4652815461180069 ) ) ;
#72279 = CARTESIAN_POINT ( 'NONE',  ( -2.415528882757435269, -293.0197865345959372, -206.1740899343403157 ) ) ;
#72280 = CARTESIAN_POINT ( 'NONE',  ( 21.55874294835324889, -286.8498353832324028, -314.3364873346901049 ) ) ;
#72281 = CARTESIAN_POINT ( 'NONE',  ( -36.94859426095777621, -274.7083943921225568, -193.4510206035448334 ) ) ;
#72282 = CARTESIAN_POINT ( 'NONE',  ( -78.85507156741245183, -273.4755238091127580, -210.2527338886961275 ) ) ;
#72283 = ORIENTED_EDGE ( 'NONE', *, *, #26014, .F. ) ;
#72284 = CARTESIAN_POINT ( 'NONE',  ( 139.6925840978351516, -0.9999999999999991118, 22.50000000000000000 ) ) ;
#72285 = CARTESIAN_POINT ( 'NONE',  ( -106.1187317843155995, -280.8812939402719167, -238.9455336487226305 ) ) ;
#72286 = CARTESIAN_POINT ( 'NONE',  ( 30.30144955051550681, -282.2543290918661683, -242.1010688962793438 ) ) ;
#72287 = CARTESIAN_POINT ( 'NONE',  ( -47.99912488591811410, -281.6786475190534134, -195.0723948610824152 ) ) ;
#72289 = VECTOR ( 'NONE', #45428, 1000.000000000000000 ) ;
#72288 = CARTESIAN_POINT ( 'NONE',  ( -56.39161494658031160, -282.3624832654638794, -341.0753965466946624 ) ) ;
#72290 = CARTESIAN_POINT ( 'NONE',  ( -111.3987606656840370, -280.3368417084622592, -276.1992221695654166 ) ) ;
#72291 = CARTESIAN_POINT ( 'NONE',  ( -92.52461752139608109, -271.7233265820392489, -221.5189908646295578 ) ) ;
#72292 = CARTESIAN_POINT ( 'NONE',  ( 209.8744251295252354, 28.03846817292548366, 12.09245862095555601 ) ) ;
#72293 = CARTESIAN_POINT ( 'NONE',  ( 158.6539576904058606, 293.9636489450775230, 0.000000000000000000 ) ) ;
#72294 = CARTESIAN_POINT ( 'NONE',  ( 32.40218928169948498, -275.9400971503192181, -237.9862127939964012 ) ) ;
#72295 = DIRECTION ( 'NONE',  ( 0.000000000000000000, 0.000000000000000000, 1.000000000000000000 ) ) ;
#72296 = CARTESIAN_POINT ( 'NONE',  ( 19.32627761765927232, -278.2340522669654206, -319.5104013540642427 ) ) ;
#72297 = CARTESIAN_POINT ( 'NONE',  ( -17.52831131349818605, -275.3761079486423000, -344.1583802288861307 ) ) ;
#72298 = ORIENTED_EDGE ( 'NONE', *, *, #26752, .F. ) ;
#72299 = DIRECTION ( 'NONE',  ( -0.000000000000000000, -1.000000000000000000, -0.000000000000000000 ) ) ;
#72300 = CARTESIAN_POINT ( 'NONE',  ( -60.69740747673365178, -285.3334311645833736, -342.0599896476688855 ) ) ;
#72301 = CARTESIAN_POINT ( 'NONE',  ( 4.604573070467113283, -291.8313952696607885, -210.3564378658357725 ) ) ;
#72302 = CARTESIAN_POINT ( 'NONE',  ( -60.47134776451586191, -285.1085826269522272, -196.9685044823650060 ) ) ;
#72303 = EDGE_CURVE ( 'NONE', #37982, #28339, #9758, .T. ) ;
#72304 = CARTESIAN_POINT ( 'NONE',  ( -111.3215431993391888, -282.8209711353330817, -268.1347240019587161 ) ) ;
#72306 = CARTESIAN_POINT ( 'NONE',  ( 35.99018845063282157, -285.4626873220703374, -257.2733993661242948 ) ) ;
#72305 = CARTESIAN_POINT ( 'NONE',  ( -92.11566487178816942, -282.4290034838576844, -319.5246440141611970 ) ) ;
#72307 = CARTESIAN_POINT ( 'NONE',  ( -21.28649211525090479, -284.0468304549337972, -342.0329719214699367 ) ) ;
#72308 = CARTESIAN_POINT ( 'NONE',  ( 14.65917142435139020, -272.7842003548737466, -216.3156740968620682 ) ) ;
#72309 = CARTESIAN_POINT ( 'NONE',  ( -113.5406754944499994, -282.9570249480919983, -269.9654331216248124 ) ) ;
#72310 = CARTESIAN_POINT ( 'NONE',  ( -80.69432203633989786, -297.6399208043936255, -331.6254403074904076 ) ) ;
#72311 = CARTESIAN_POINT ( 'NONE',  ( -1.813072759501491493, -284.5216069130643746, -204.1210616263202269 ) ) ;
#72312 = CARTESIAN_POINT ( 'NONE',  ( -107.3379690782405049, -279.2069978524250473, -292.0698910013197178 ) ) ;
#72313 = CARTESIAN_POINT ( 'NONE',  ( 35.37740486799152251, -289.7962630883467341, -289.3863695722653802 ) ) ;
#72314 = DIRECTION ( 'NONE',  ( -0.9565177946839410472, -1.517921082078008940E-15, 0.2916739763039721267 ) ) ;
#72315 = FACE_OUTER_BOUND ( 'NONE', #73290, .T. ) ;
#72316 = CARTESIAN_POINT ( 'NONE',  ( 8.060766910421152787, -296.3569860463745158, -330.7592154862559823 ) ) ;
#72317 = CARTESIAN_POINT ( 'NONE',  ( -110.4411794156051343, -276.3358494383647326, -287.1950874932304600 ) ) ;
#72318 = CARTESIAN_POINT ( 'NONE',  ( -98.03835466682205890, -289.1187727297029824, -317.4787892858459486 ) ) ;
#72319 = CARTESIAN_POINT ( 'NONE',  ( -23.38732462683824309, -293.2707813432017474, -342.8820085607288206 ) ) ;
#72320 = CARTESIAN_POINT ( 'NONE',  ( -32.91669927876350954, -278.7938902948168334, -197.0013003295241276 ) ) ;
#72321 = CARTESIAN_POINT ( 'NONE',  ( -73.42692764383861004, -295.7076050945018437, -205.4864554666810932 ) ) ;
#72322 = CARTESIAN_POINT ( 'NONE',  ( -60.42967334378176503, -293.0616995951370427, -200.5353064467257695 ) ) ;
#72323 = CARTESIAN_POINT ( 'NONE',  ( -95.99890600148557951, -281.6948066931273615, -223.6242672951989618 ) ) ;
#72324 = CARTESIAN_POINT ( 'NONE',  ( 21.73743018943032368, -292.6864266111173265, -318.6761792991862876 ) ) ;
#72325 = CARTESIAN_POINT ( 'NONE',  ( -83.02569930113418195, -291.2896577480779001, -328.3215582203089298 ) ) ;
#72326 = CARTESIAN_POINT ( 'NONE',  ( -103.7138287943378714, -289.2780502935710842, -233.3649756436069538 ) ) ;
#72327 = ADVANCED_FACE ( 'NONE', ( #45250 ), #9271, .T. ) ;
#72328 = CARTESIAN_POINT ( 'NONE',  ( 31.96035507837568446, -289.3043318698337885, -295.1118767721363270 ) ) ;
#72329 = CARTESIAN_POINT ( 'NONE',  ( 152.4536156746142410, 129.7208004331680797, -12.50000000000000000 ) ) ;
#72330 = CARTESIAN_POINT ( 'NONE',  ( -86.83110237122282626, -290.5643688097696895, -324.3130494404123283 ) ) ;
#72331 = CARTESIAN_POINT ( 'NONE',  ( 199.0061125298537377, 276.0000000000000568, -7.725424859374024678 ) ) ;
#72332 = CIRCLE ( 'NONE', #48101, 5.841085083515828558 ) ;
#72333 = CARTESIAN_POINT ( 'NONE',  ( -17.81068312611191118, -290.0107717184785088, -344.4323545887829141 ) ) ;
#72334 = CARTESIAN_POINT ( 'NONE',  ( -38.12692121901730502, -278.0624698668577253, -195.0100049518649143 ) ) ;
#72335 = CARTESIAN_POINT ( 'NONE',  ( -101.8758126719622936, -279.4378021132837375, -228.2992820170711923 ) ) ;
#72336 = CARTESIAN_POINT ( 'NONE',  ( 37.17027205420120595, -281.4608930582771791, -289.6927059440723724 ) ) ;
#72337 = CARTESIAN_POINT ( 'NONE',  ( 25.91180322605778130, -286.0943649804596589, -310.6599388254431346 ) ) ;
#72338 = CARTESIAN_POINT ( 'NONE',  ( 197.1983186874051341, 40.91381848194614435, 12.13059964849341021 ) ) ;
#72339 = CARTESIAN_POINT ( 'NONE',  ( -1.858755135424154492, -280.7165115041714216, -335.5816749656914340 ) ) ;
#72340 = CARTESIAN_POINT ( 'NONE',  ( -110.2802654800144637, -282.3270707908436634, -287.8788439460030304 ) ) ;
#72341 = CARTESIAN_POINT ( 'NONE',  ( 202.9738562182569694, 291.9636489450776367, -53.99999999998589573 ) ) ;
#72342 = CARTESIAN_POINT ( 'NONE',  ( -98.01320858352929122, -277.6548301704020787, -224.0615960724933871 ) ) ;
#72343 =( BOUNDED_SURFACE ( )  B_SPLINE_SURFACE ( 3, 2, ( 
 ( #37391, #16553, #9432 ),
 ( #36944, #30772, #44497 ),
 ( #17019, #73402, #15167 ),
 ( #66300, #30301, #2364 ) ),
 .UNSPECIFIED., .F., .F., .F. ) 
 B_SPLINE_SURFACE_WITH_KNOTS ( ( 4, 4 ),
 ( 3, 3 ),
 ( 1.570796326794896558, 2.004620063563922638 ),
 ( 0.000000000000000000, 1.000000000000000000 ),
 .UNSPECIFIED. ) 
 GEOMETRIC_REPRESENTATION_ITEM ( )  RATIONAL_B_SPLINE_SURFACE ( (
 ( 1.000000000000000000, 0.7071067811865475727, 1.000000000000000000),
 ( 1.000000000000000000, 0.7478056585118711963, 1.000000000000000000),
 ( 1.000000000000000000, 0.7849082635113622253, 1.000000000000000000),
 ( 1.000000000000000000, 0.8168508380123946644, 1.000000000000000000) ) ) 
 REPRESENTATION_ITEM ( '' )  SURFACE ( )  );
#72344 = CARTESIAN_POINT ( 'NONE',  ( -87.53719931808655019, -284.2913338563616321, -212.3088931166980160 ) ) ;
#72345 = CARTESIAN_POINT ( 'NONE',  ( -41.89490681170891406, -298.9346230229483581, -197.2675015902693474 ) ) ;
#72346 = CARTESIAN_POINT ( 'NONE',  ( -103.1318838608503370, -292.6028230561269083, -236.8100478987950055 ) ) ;
#72347 = CARTESIAN_POINT ( 'NONE',  ( 39.03532149031855880, -277.0232541309891303, -273.9976813426529816 ) ) ;
#72348 = CARTESIAN_POINT ( 'NONE',  ( 35.04202796950075083, -275.0919070058828879, -260.7338965005125715 ) ) ;
#72349 = CARTESIAN_POINT ( 'NONE',  ( -48.05419328290528114, -297.1884613256227681, -344.6448126325227008 ) ) ;
#72350 = CARTESIAN_POINT ( 'NONE',  ( 12.41744354550193030, -288.5476419365103879, -329.1235858115808810 ) ) ;
#72351 =( BOUNDED_CURVE ( )  B_SPLINE_CURVE ( 3, ( #77849, #33817, #27180, #12998 ),
 .UNSPECIFIED., .F., .F. ) 
 B_SPLINE_CURVE_WITH_KNOTS ( ( 4, 4 ),
 ( 4.712388980384689674, 6.283185307179586232 ),
 .UNSPECIFIED. ) 
 CURVE ( )  GEOMETRIC_REPRESENTATION_ITEM ( )  RATIONAL_B_SPLINE_CURVE ( ( 1.000000000000000000, 0.8047378541243649375, 0.8047378541243649375, 1.000000000000000000 ) ) 
 REPRESENTATION_ITEM ( '' )  );
#72352 = CARTESIAN_POINT ( 'NONE',  ( 35.22376406062967646, -279.3623275507391668, -249.2536355017128642 ) ) ;
#72353 = CARTESIAN_POINT ( 'NONE',  ( -47.74129086144256462, -291.7568585391829856, -194.0128379952026876 ) ) ;
#72354 = CARTESIAN_POINT ( 'NONE',  ( -49.71672652828929984, -290.9493209418427568, -198.1274475385925768 ) ) ;
#72355 = CARTESIAN_POINT ( 'NONE',  ( 7.684596219073196011, -292.4373024779761749, -330.3413920984033325 ) ) ;
#72356 = ORIENTED_EDGE ( 'NONE', *, *, #84148, .T. ) ;
#72357 = CARTESIAN_POINT ( 'NONE',  ( 197.2510236111309609, 71.96844395090404589, 11.91691450877446279 ) ) ;
#72358 = CARTESIAN_POINT ( 'NONE',  ( -89.85619900138516414, -290.7932219936263323, -219.5652928614318000 ) ) ;
#72359 = CARTESIAN_POINT ( 'NONE',  ( 140.6539576904058606, 275.0000000000000568, -10.49999999999999822 ) ) ;
#72360 = CARTESIAN_POINT ( 'NONE',  ( -60.45054442856106647, -286.7009913387566939, -197.1018731090796337 ) ) ;
#72361 = CARTESIAN_POINT ( 'NONE',  ( 30.89617123739170168, -273.2666405000204009, -285.9686137636504668 ) ) ;
#72362 = CARTESIAN_POINT ( 'NONE',  ( -34.87424860828389939, -294.0806163091604049, -347.0861588532150677 ) ) ;
#72363 = CARTESIAN_POINT ( 'NONE',  ( -111.2492318530325690, -286.1187586573374233, -250.3887463344401851 ) ) ;
#72364 = CARTESIAN_POINT ( 'NONE',  ( -77.04728420643806430, -285.3374312969164066, -209.0437629944918854 ) ) ;
#72365 = CARTESIAN_POINT ( 'NONE',  ( 30.80869125610385950, -276.6984068812309943, -242.1873839013264558 ) ) ;
#72366 = CARTESIAN_POINT ( 'NONE',  ( -6.098930381301286729, -292.6596313054743064, -338.1529769696238645 ) ) ;
#72367 = CARTESIAN_POINT ( 'NONE',  ( 35.32346731477522894, -295.4952606656176499, -284.4233886388359451 ) ) ;
#72368 = CARTESIAN_POINT ( 'NONE',  ( -24.27390023893061155, -275.6766422279484345, -342.6372412801852647 ) ) ;
#72369 = ORIENTED_EDGE ( 'NONE', *, *, #79409, .F. ) ;
#72370 = CARTESIAN_POINT ( 'NONE',  ( 195.0647618973419242, 40.86965449270967099, 13.52197506507135571 ) ) ;
#72371 = CARTESIAN_POINT ( 'NONE',  ( -56.06924778861748138, -294.9537140593471349, -345.0271962916477264 ) ) ;
#72372 = CARTESIAN_POINT ( 'NONE',  ( 34.04407598824657555, -289.1979204152081593, -249.2120527142809010 ) ) ;
#72373 = CARTESIAN_POINT ( 'NONE',  ( -37.76724320851720051, -296.0466686025325771, -195.3609641834697754 ) ) ;
#72374 = CARTESIAN_POINT ( 'NONE',  ( -70.60744661030534530, -298.7033710379445210, -201.2605924963585835 ) ) ;
#72375 = CARTESIAN_POINT ( 'NONE',  ( 4.777335013650172435, -287.2889754373408095, -210.5507093577442674 ) ) ;
#72376 = EDGE_LOOP ( 'NONE', ( #81238, #3701 ) ) ;
#72377 = CARTESIAN_POINT ( 'NONE',  ( -100.0498363963993285, -278.1986015786310986, -226.0834728447778730 ) ) ;
#72378 = CARTESIAN_POINT ( 'NONE',  ( 32.14148067564948263, -294.6277154756776895, -303.4306896044388395 ) ) ;
#72379 = CARTESIAN_POINT ( 'NONE',  ( -8.722035735439540360, -286.8212591130728129, -340.5265630167794484 ) ) ;
#72380 = CARTESIAN_POINT ( 'NONE',  ( -39.10310031736396752, -295.4069700298720704, -347.3198196412745915 ) ) ;
#72381 = CARTESIAN_POINT ( 'NONE',  ( -14.84391723107736638, -292.6851178169182504, -200.8921518794097949 ) ) ;
#72382 = DIRECTION ( 'NONE',  ( -1.000000000000000000, 0.000000000000000000, 0.000000000000000000 ) ) ;
#72383 = DIRECTION ( 'NONE',  ( 0.000000000000000000, 1.000000000000000000, 0.000000000000000000 ) ) ;
#72384 = CARTESIAN_POINT ( 'NONE',  ( -110.6395504404451202, -271.5021484970271217, -270.3477489206637756 ) ) ;
#72385 = CARTESIAN_POINT ( 'NONE',  ( 15.80231778419920197, -288.3086272243522785, -215.6032773406455760 ) ) ;
#72386 = CARTESIAN_POINT ( 'NONE',  ( -55.63300648810263738, -292.7666405000204577, -350.3538533559490702 ) ) ;
#72387 = ORIENTED_EDGE ( 'NONE', *, *, #39617, .T. ) ;
#72388 = CARTESIAN_POINT ( 'NONE',  ( -108.4152802970828589, -278.2743668322917188, -241.0036830082741233 ) ) ;
#72389 = CARTESIAN_POINT ( 'NONE',  ( -62.11828371793386339, -285.3750885773587811, -341.0283543836637250 ) ) ;
#72390 = CARTESIAN_POINT ( 'NONE',  ( -75.79438099187554201, -284.1244679167076583, -204.2699171581229507 ) ) ;
#72391 = CARTESIAN_POINT ( 'NONE',  ( 13.11422935688720237, -286.4208306744771448, -325.1624225558999228 ) ) ;
#72392 = CARTESIAN_POINT ( 'NONE',  ( 21.69369989309521074, -278.0595462401945497, -317.8698256562278175 ) ) ;
#72393 = CARTESIAN_POINT ( 'NONE',  ( -47.28732485252812978, -298.4148558079792792, -197.9284228179813283 ) ) ;
#72394 = ORIENTED_EDGE ( 'NONE', *, *, #56360, .F. ) ;
#72395 = CARTESIAN_POINT ( 'NONE',  ( 34.54647888706180225, -292.4379195302273615, -285.6966662491015541 ) ) ;
#72397 = CARTESIAN_POINT ( 'NONE',  ( -49.15021637553330436, -279.2462641699862047, -198.2192327012321016 ) ) ;
#72396 = CARTESIAN_POINT ( 'NONE',  ( -96.09300449106507358, -277.9446425157504450, -313.7097088486643770 ) ) ;
#72398 = CARTESIAN_POINT ( 'NONE',  ( 7.044840683782811475, -275.7202922558966520, -207.7553474174759742 ) ) ;
#72399 = CARTESIAN_POINT ( 'NONE',  ( -71.44579397653382102, -276.4123722067806170, -339.0517526711394112 ) ) ;
#72400 = CARTESIAN_POINT ( 'NONE',  ( 151.8322611248232761, 206.3920080503552299, -215.3183130715498237 ) ) ;
#72401 = EDGE_CURVE ( 'NONE', #3540, #29794, #66598, .T. ) ;
#72402 = CARTESIAN_POINT ( 'NONE',  ( -93.24590105861459222, -297.2616604054534264, -322.4699851835310938 ) ) ;
#72403 = CARTESIAN_POINT ( 'NONE',  ( 164.2231345125756263, 300.2961574867697436, 4.888549259831427740 ) ) ;
#72404 = EDGE_LOOP ( 'NONE', ( #48714, #33937, #91193, #74675 ) ) ;
#72405 = VECTOR ( 'NONE', #72669, 1000.000000000000000 ) ;
#72406 = CARTESIAN_POINT ( 'NONE',  ( 82.62533370646633557, -301.4052215159320554, -193.6716506432818505 ) ) ;
#72407 = CARTESIAN_POINT ( 'NONE',  ( -73.72092288612660127, -286.6367395514758414, -206.7008348303947116 ) ) ;
#72408 = CARTESIAN_POINT ( 'NONE',  ( -30.99117931021702077, -287.8914667457218002, -194.6271629235722003 ) ) ;
#72409 = CARTESIAN_POINT ( 'NONE',  ( 8.036741488494483221, -287.7612405829243585, -327.6733305055087726 ) ) ;
#72410 = CARTESIAN_POINT ( 'NONE',  ( -0.4104896363085420719, -282.0823907548179363, -337.8713228869076488 ) ) ;
#72411 = CARTESIAN_POINT ( 'NONE',  ( -104.0847441641706723, -277.3743710621465084, -238.7481140434367433 ) ) ;
#72412 = CARTESIAN_POINT ( 'NONE',  ( -111.3248661378664366, -286.3332882958701475, -276.4731246619610943 ) ) ;
#72413 = CARTESIAN_POINT ( 'NONE',  ( -72.44307058668638888, -278.0584812247415698, -205.5645012077888509 ) ) ;
#72414 = CARTESIAN_POINT ( 'NONE',  ( -78.89714023838975265, -278.9401774919166996, -331.0398147248430973 ) ) ;
#72415 = CARTESIAN_POINT ( 'NONE',  ( 35.43892178647172386, -275.9528650136715555, -263.4086585093682515 ) ) ;
#72416 = CARTESIAN_POINT ( 'NONE',  ( 22.96531292912590416, -286.9819393652680901, -317.6164683223841507 ) ) ;
#72417 = CARTESIAN_POINT ( 'NONE',  ( -4.224152200932622669, -283.4294509516602147, -339.7108995702823222 ) ) ;
#72418 = CARTESIAN_POINT ( 'NONE',  ( -13.43510110557483195, -283.2421690279384165, -343.4911489294484568 ) ) ;
#72419 = ORIENTED_EDGE ( 'NONE', *, *, #19910, .T. ) ;
#72420 = ORIENTED_EDGE ( 'NONE', *, *, #65268, .T. ) ;
#72421 = CARTESIAN_POINT ( 'NONE',  ( 123.4306832106270946, -134.2391364535880882, 0.000000000000000000 ) ) ;
#72422 = CARTESIAN_POINT ( 'NONE',  ( -45.86293297917267608, -291.0193708864263726, -345.6974809327636535 ) ) ;
#72423 = CARTESIAN_POINT ( 'NONE',  ( -96.91669144151408943, -288.5891781684961188, -318.3830196501817227 ) ) ;
#72424 = CARTESIAN_POINT ( 'NONE',  ( -54.25427897830437729, -272.8882896585868139, -199.1054296201107547 ) ) ;
#72425 = CARTESIAN_POINT ( 'NONE',  ( 27.97017481252142446, -292.3679205973182889, -229.6689625656405838 ) ) ;
#72426 = CARTESIAN_POINT ( 'NONE',  ( -42.73378834055788644, -287.6011457977434702, -343.9080062660941053 ) ) ;
#72427 = CARTESIAN_POINT ( 'NONE',  ( -0.7362689309894312473, -290.7852711599860527, -206.0190237905486583 ) ) ;
#72428 = CARTESIAN_POINT ( 'NONE',  ( 30.85981004913265124, -289.1198039435548708, -297.6217723295335986 ) ) ;
#72429 = CARTESIAN_POINT ( 'NONE',  ( -20.25526795762937127, -294.7662352645559167, -195.3538533559490702 ) ) ;
#72430 = CARTESIAN_POINT ( 'NONE',  ( 6.779081402897817021, -290.4525920728215738, -331.0746385504962745 ) ) ;
#72431 = CARTESIAN_POINT ( 'NONE',  ( -66.28539371404242786, -289.6739569138085244, -200.9904395240850761 ) ) ;
#72432 = CARTESIAN_POINT ( 'NONE',  ( -112.3718944099562691, -292.5751568835734133, -268.5823054727151202 ) ) ;
#72433 = CARTESIAN_POINT ( 'NONE',  ( -110.2298382067374689, -285.5936551189691386, -262.7374332444052243 ) ) ;
#72434 = CARTESIAN_POINT ( 'NONE',  ( 23.31948440883498108, -294.9485837904136929, -225.9736296617211906 ) ) ;
#72435 = FACE_OUTER_BOUND ( 'NONE', #25061, .T. ) ;
#72436 = CARTESIAN_POINT ( 'NONE',  ( -91.01558547671376687, -275.2743451916153390, -217.4695228705287775 ) ) ;
#72437 = CARTESIAN_POINT ( 'NONE',  ( 34.49474068519236170, -280.5660015079667460, -256.4340652475358411 ) ) ;
#72438 = CARTESIAN_POINT ( 'NONE',  ( -26.47756707605085680, -280.9138818161818563, -344.6227910774465499 ) ) ;
#72439 = CARTESIAN_POINT ( 'NONE',  ( -47.62011244711185043, -294.3768334893219958, -346.5090861784170784 ) ) ;
#72440 = CARTESIAN_POINT ( 'NONE',  ( -27.12847242738258302, -272.4234578560213436, -197.0042323288284933 ) ) ;
#72441 = CARTESIAN_POINT ( 'NONE',  ( -107.6318756588853347, -276.3104907502766423, -295.0248476005363045 ) ) ;
#72442 = CARTESIAN_POINT ( 'NONE',  ( -92.22424347755826091, -298.5615567458141868, -221.4821867932911630 ) ) ;
#72443 = CARTESIAN_POINT ( 'NONE',  ( -6.501571968834195303, -296.0642447797637828, -337.1762466134138663 ) ) ;
#72444 = LINE ( 'NONE', #65363, #36905 ) ;
#72445 = CARTESIAN_POINT ( 'NONE',  ( 20.65745723903233255, -294.9814197655427392, -314.9764700530721484 ) ) ;
#72446 = CARTESIAN_POINT ( 'NONE',  ( 200.3424981856614693, 61.71662552184319139, 9.000000000000000000 ) ) ;
#72448 = CARTESIAN_POINT ( 'NONE',  ( -91.84489242409644305, -297.2465951656284915, -221.7977364122492645 ) ) ;
#72447 = CARTESIAN_POINT ( 'NONE',  ( 35.54690944578270972, -285.8168539298790733, -289.4832883625795716 ) ) ;
#72449 = CARTESIAN_POINT ( 'NONE',  ( -114.2083498269823281, -284.4851597106874692, -275.7177805342258807 ) ) ;
#72450 = CARTESIAN_POINT ( 'NONE',  ( 38.76531059052156536, -287.0732505586276488, -258.7205217537386375 ) ) ;
#72451 = CARTESIAN_POINT ( 'NONE',  ( -3.993769976123546783, -290.4927471217835091, -203.3547228439092009 ) ) ;
#72452 = CARTESIAN_POINT ( 'NONE',  ( -40.99047764218310874, -279.2045355661306871, -193.5961081341890235 ) ) ;
#72453 = CARTESIAN_POINT ( 'NONE',  ( -4.771743288812454686, -277.9809262143061233, -202.8022627189028810 ) ) ;
#72454 = PLANE ( 'NONE',  #45389 ) ;
#72455 = CARTESIAN_POINT ( 'NONE',  ( 33.41612651763995245, -286.0907303174925573, -250.8557219609286904 ) ) ;
#72456 = ADVANCED_FACE ( 'NONE', ( #2203 ), #76158, .T. ) ;
#72458 = CARTESIAN_POINT ( 'NONE',  ( 129.4467878515196162, -299.5541904835127980, -195.3611179825600175 ) ) ;
#72457 = CARTESIAN_POINT ( 'NONE',  ( -98.78974503100785398, -288.8593147845825797, -316.2699865052107953 ) ) ;
#72459 = CARTESIAN_POINT ( 'NONE',  ( -97.82749601706665032, -297.5690545741524033, -312.6447899086027178 ) ) ;
#72460 = CARTESIAN_POINT ( 'NONE',  ( -35.36956734517416123, -281.5016849120055440, -193.9627623263442047 ) ) ;
#72462 = CARTESIAN_POINT ( 'NONE',  ( 23.70253940223141953, -280.6623913137541422, -230.1988833781170172 ) ) ;
#72461 = CARTESIAN_POINT ( 'NONE',  ( -111.2700146654799198, -294.7596233637084424, -255.6999702150303904 ) ) ;
#72463 = CARTESIAN_POINT ( 'NONE',  ( -16.50483899443910474, -294.9569303705647485, -344.5434395678910278 ) ) ;
#72464 = CARTESIAN_POINT ( 'NONE',  ( 25.94527036239873752, -285.0793805991111185, -229.0806920683648400 ) ) ;
#72465 = EDGE_CURVE ( 'NONE', #64288, #90166, #37692, .T. ) ;
#72466 = CARTESIAN_POINT ( 'NONE',  ( -78.82630241131643345, -281.4937130287340210, -207.8165809848790389 ) ) ;
#72468 = CARTESIAN_POINT ( 'NONE',  ( -107.0970534282177908, -295.3140784668618721, -292.8323044787042591 ) ) ;
#72467 = AXIS2_PLACEMENT_3D ( 'NONE', #15844, #9650, #31902 ) ;
#72469 = ORIENTED_EDGE ( 'NONE', *, *, #30878, .T. ) ;
#72470 = PLANE ( 'NONE',  #60497 ) ;
#72471 = CARTESIAN_POINT ( 'NONE',  ( -70.93302701220437712, -285.4774176831608656, -337.0347642082821267 ) ) ;
#72472 = CARTESIAN_POINT ( 'NONE',  ( 143.6449502718966755, -26.00396092263537540, 21.50000000000000000 ) ) ;
#72473 = CARTESIAN_POINT ( 'NONE',  ( -4.829096099716524648, -292.1237833571632905, -337.9475929042657754 ) ) ;
#72474 = CARTESIAN_POINT ( 'NONE',  ( -7.743308129422456609, -273.6273474602290321, -199.3955810154421613 ) ) ;
#72475 = CARTESIAN_POINT ( 'NONE',  ( -98.29836869864304560, -290.9436200617894315, -230.1035884041222914 ) ) ;
#72476 = CARTESIAN_POINT ( 'NONE',  ( 33.99955040372994830, -283.3144039726696519, -288.8812401604149613 ) ) ;
#72477 = CARTESIAN_POINT ( 'NONE',  ( -34.02489317914503175, -275.6946953407403385, -196.6356867657671330 ) ) ;
#72478 = CARTESIAN_POINT ( 'NONE',  ( 29.07472106646553911, -283.6432110681266749, -307.8224134474925791 ) ) ;
#72479 = CARTESIAN_POINT ( 'NONE',  ( -1.069050037832547373, -281.3541058323182256, -334.1688397771936252 ) ) ;
#72480 = CARTESIAN_POINT ( 'NONE',  ( -111.4649080150244771, -280.4054939245332889, -281.7957453037777782 ) ) ;
#72481 = CARTESIAN_POINT ( 'NONE',  ( -35.82814869556214887, -298.0706118946271772, -193.3611179679607517 ) ) ;
#72482 = CARTESIAN_POINT ( 'NONE',  ( -38.35528272054697396, -273.8730960703282449, -193.3677893438971012 ) ) ;
#72483 = CARTESIAN_POINT ( 'NONE',  ( 35.89559336655222666, -295.2989859739282679, -256.9632095782571355 ) ) ;
#72484 = CARTESIAN_POINT ( 'NONE',  ( 215.7837434059060229, -142.7221692137691775, 8.778910157967997563 ) ) ;
#72485 = CARTESIAN_POINT ( 'NONE',  ( 154.7659666677267865, 20.47222690886501439, 12.53936336329526391 ) ) ;
#72486 = CARTESIAN_POINT ( 'NONE',  ( 25.47419231884276769, -292.2589954653012114, -312.7222928556045645 ) ) ;
#72487 = CARTESIAN_POINT ( 'NONE',  ( 9.529357840163710236, -274.2245411284644661, -214.2494125576347130 ) ) ;
#72488 = CARTESIAN_POINT ( 'NONE',  ( -69.35014769092640563, -293.1587404554376235, -201.0781015635876372 ) ) ;
#72490 = CARTESIAN_POINT ( 'NONE',  ( -50.51324527192370795, -293.0926039505428662, -194.8990804000737569 ) ) ;
#72489 = CARTESIAN_POINT ( 'NONE',  ( -69.91165696735023971, -276.1233781216988064, -202.8022627189028810 ) ) ;
#72491 = CARTESIAN_POINT ( 'NONE',  ( 6.949720710678732871, -290.4483194737858867, -330.7440225901233930 ) ) ;
#72492 = CARTESIAN_POINT ( 'NONE',  ( -74.95628212740679430, -275.5542320899593278, -335.0540205912255374 ) ) ;
#72493 = CARTESIAN_POINT ( 'NONE',  ( -98.82466471295813903, -279.8997062925695900, -312.3272860733979996 ) ) ;
#72494 = CARTESIAN_POINT ( 'NONE',  ( 32.18184845277908579, -291.2835686890792886, -243.7567877200997373 ) ) ;
#72495 = CARTESIAN_POINT ( 'NONE',  ( 20.67961527332043659, -284.0792396965493367, -319.0831093466072730 ) ) ;
#72496 = ORIENTED_EDGE ( 'NONE', *, *, #52934, .T. ) ;
#72497 = CARTESIAN_POINT ( 'NONE',  ( -92.57790451437017509, -283.5383840610160746, -318.1404784485881123 ) ) ;
#72498 = CARTESIAN_POINT ( 'NONE',  ( -3.805246342170619744, -281.5639037684901496, -201.3771099570574847 ) ) ;
#72499 = CARTESIAN_POINT ( 'NONE',  ( -90.17544299733241076, -282.5738928029912813, -325.9010110979442629 ) ) ;
#72500 = CARTESIAN_POINT ( 'NONE',  ( -84.43207734220997907, -280.3633900977930011, -209.6694526033395789 ) ) ;
#72501 =( LENGTH_UNIT ( ) NAMED_UNIT ( * ) SI_UNIT ( .MILLI., .METRE. ) );
#72502 = CARTESIAN_POINT ( 'NONE',  ( 37.23225998466632092, -277.2770902609273094, -286.5911028344676197 ) ) ;
#72503 = CARTESIAN_POINT ( 'NONE',  ( -102.0172624299486870, -292.6233781216987495, -301.5434626090942061 ) ) ;
#72504 = VERTEX_POINT ( 'NONE', #15469 ) ;
#72505 = CARTESIAN_POINT ( 'NONE',  ( -71.39786857046402702, -299.6026364355964233, -203.5248355771068987 ) ) ;
#72506 = CARTESIAN_POINT ( 'NONE',  ( -112.0379594211455299, -276.5689253040086442, -270.6191293348912268 ) ) ;
#72507 = CARTESIAN_POINT ( 'NONE',  ( -109.4761318875154927, -292.6188475049196995, -246.3091178506803374 ) ) ;
#72508 = CARTESIAN_POINT ( 'NONE',  ( 34.42286396606191090, -293.0840961461039456, -284.2801699919195926 ) ) ;
#72509 = CARTESIAN_POINT ( 'NONE',  ( -74.40318166068551875, -289.0390548109408542, -337.7999947942155359 ) ) ;
#72510 = CARTESIAN_POINT ( 'NONE',  ( 153.2628468892384603, 20.37991841447902175, -11.93555113919331134 ) ) ;
#72512 = CARTESIAN_POINT ( 'NONE',  ( -104.2016957520456657, -283.3707929919136177, -238.9961436908962753 ) ) ;
#72511 = CARTESIAN_POINT ( 'NONE',  ( 39.12199617771334204, -292.1264693963765922, -270.3284663171629063 ) ) ;
#72513 = CARTESIAN_POINT ( 'NONE',  ( -103.9433589941564975, -291.9756494575484567, -303.1495994008913044 ) ) ;
#72514 = CARTESIAN_POINT ( 'NONE',  ( -37.26085850520976805, -284.5330222512640148, -196.6552701262254175 ) ) ;
#72515 = CARTESIAN_POINT ( 'NONE',  ( 8.112016673473407380, -283.7311679443093908, -328.1773409008856106 ) ) ;
#72516 = CARTESIAN_POINT ( 'NONE',  ( -110.5538003603362540, -291.2004684704143074, -293.6173345970029231 ) ) ;
#72517 = CARTESIAN_POINT ( 'NONE',  ( -54.51332980933040062, -280.3179963928682241, -199.2939224595110375 ) ) ;
#72518 = CARTESIAN_POINT ( 'NONE',  ( 37.37742595089603981, -292.1341660051416511, -253.4185054195157250 ) ) ;
#72519 = CARTESIAN_POINT ( 'NONE',  ( 20.45819815466221669, -289.0415479219254280, -321.0102881602378488 ) ) ;
#72520 = CARTESIAN_POINT ( 'NONE',  ( 37.31559320140213032, -287.8116573555047921, -251.7650039744999049 ) ) ;
#72521 = CARTESIAN_POINT ( 'NONE',  ( -77.05084475036461811, -285.6707376738506809, -209.0460689899842350 ) ) ;
#72522 = VERTEX_POINT ( 'NONE', #44340 ) ;
#72523 = CARTESIAN_POINT ( 'NONE',  ( 196.0517256323039135, 25.50333437355849142, 11.93519303445567736 ) ) ;
#72524 = CARTESIAN_POINT ( 'NONE',  ( -19.55391271551662413, -296.6863134951481129, -344.0622593021132047 ) ) ;
#72525 = CARTESIAN_POINT ( 'NONE',  ( -110.7469981448205090, -294.9642398368066551, -291.9703047470334241 ) ) ;
#72526 = CARTESIAN_POINT ( 'NONE',  ( -107.3450741805652484, -277.3247976227939944, -292.0469738322642002 ) ) ;
#72527 = CARTESIAN_POINT ( 'NONE',  ( 30.68463594159268837, -298.2314732075915913, -193.4703145117252063 ) ) ;
#72528 = VECTOR ( 'NONE', #30390, 1000.000000000000000 ) ;
#72529 = CARTESIAN_POINT ( 'NONE',  ( -97.76283247898805939, -294.4493080345956741, -312.5510992403744694 ) ) ;
#72530 = CARTESIAN_POINT ( 'NONE',  ( 27.66738970187153868, -277.7898860117940103, -305.8489921116553774 ) ) ;
#72531 = CARTESIAN_POINT ( 'NONE',  ( -100.3159900907502760, -271.2252678196702504, -231.0533034547927116 ) ) ;
#72532 = CARTESIAN_POINT ( 'NONE',  ( 0.09847226857732659100, -293.7677214703746245, -207.2313785898181209 ) ) ;
#72533 = CARTESIAN_POINT ( 'NONE',  ( -28.84656577089856100, -296.0217406351200111, -343.2275856026936935 ) ) ;
#72534 = CARTESIAN_POINT ( 'NONE',  ( -43.38482778162041598, -264.5778734463897877, -435.9208459153147714 ) ) ;
#72535 = CARTESIAN_POINT ( 'NONE',  ( -95.99330775262825455, -293.9065832461334935, -317.3923178194326056 ) ) ;
#72536 = CARTESIAN_POINT ( 'NONE',  ( -73.24043553275097906, -298.2406541149025543, -202.2979816630649168 ) ) ;
#72537 = CARTESIAN_POINT ( 'NONE',  ( -92.61322325112715248, -275.2606048656767825, -219.6463460953772824 ) ) ;
#72538 = CARTESIAN_POINT ( 'NONE',  ( -110.2081949564013570, -291.5899308944818245, -263.0206561951536628 ) ) ;
#72539 = CARTESIAN_POINT ( 'NONE',  ( -61.01600955640119395, -295.7012379566804157, -339.4915810968141159 ) ) ;
#72540 = CARTESIAN_POINT ( 'NONE',  ( -111.3848459749370647, -280.7118448247438778, -256.2912972431313960 ) ) ;
#72541 = CARTESIAN_POINT ( 'NONE',  ( -81.93773299491124362, -278.1431198513420782, -208.1960785785962003 ) ) ;
#72542 = CARTESIAN_POINT ( 'NONE',  ( 0.8105687729348383108, -281.9057659049092877, -337.1424670130624008 ) ) ;
#72543 = CARTESIAN_POINT ( 'NONE',  ( 22.55637436049275735, -275.5481237413729332, -318.6057283681213335 ) ) ;
#72544 = CARTESIAN_POINT ( 'NONE',  ( -108.7806349874023368, -282.3600037446211104, -291.3301799447464759 ) ) ;
#72545 = CARTESIAN_POINT ( 'NONE',  ( -105.4512804616232557, -277.3975232945321068, -236.0745903104890999 ) ) ;
#72546 = CARTESIAN_POINT ( 'NONE',  ( -20.15017322816388301, -278.2722409075090582, -197.1333356819495179 ) ) ;
#72547 = CARTESIAN_POINT ( 'NONE',  ( -106.8570959947575858, -271.4454226281304727, -246.2160428287999139 ) ) ;
#72548 = CARTESIAN_POINT ( 'NONE',  ( 37.45331456715422291, -277.4727434856657169, -264.1638155495293745 ) ) ;
#72549 = DIRECTION ( 'NONE',  ( 0.000000000000000000, 0.000000000000000000, 1.000000000000000000 ) ) ;
#72550 = CARTESIAN_POINT ( 'NONE',  ( 26.66880200969132275, -291.0396556977514138, -230.4998943694332638 ) ) ;
#72551 = CARTESIAN_POINT ( 'NONE',  ( -110.7818462594062794, -290.2593683143845169, -293.6771520792515275 ) ) ;
#72552 = CARTESIAN_POINT ( 'NONE',  ( 34.81848707872747184, -277.2798301914128274, -249.1334051030851526 ) ) ;
#72553 = CARTESIAN_POINT ( 'NONE',  ( -55.71986598453124628, -295.8150078339552920, -197.7659835107414494 ) ) ;
#72554 = CARTESIAN_POINT ( 'NONE',  ( -114.0478625993830946, -283.6824563952880567, -275.6963609930496091 ) ) ;
#72555 = CARTESIAN_POINT ( 'NONE',  ( 151.4851178187871312, 15.00000000000000000, 0.000000000000000000 ) ) ;
#72556 = CARTESIAN_POINT ( 'NONE',  ( -94.89748846829182582, -281.8875155036677711, -318.4673863696773424 ) ) ;
#72557 = DIRECTION ( 'NONE',  ( 1.000000000000000000, 0.000000000000000000, 0.000000000000000000 ) ) ;
#72558 = CARTESIAN_POINT ( 'NONE',  ( -4.642465675522531754, -291.2877032153002119, -204.6364584404161917 ) ) ;
#72559 = CARTESIAN_POINT ( 'NONE',  ( -110.6369739595502750, -282.8455323536790615, -258.5050059402002489 ) ) ;
#72560 = CARTESIAN_POINT ( 'NONE',  ( 154.1407330040854333, 249.5000000000000568, -13.42592592592592915 ) ) ;
#72561 = CARTESIAN_POINT ( 'NONE',  ( 197.3748232817349049, 275.0000000000000568, -12.45182892472559821 ) ) ;
#72562 = CARTESIAN_POINT ( 'NONE',  ( -33.37794337555711621, -290.1018730301097435, -195.4530950868605430 ) ) ;
#72563 = CARTESIAN_POINT ( 'NONE',  ( -112.3133133919373137, -283.2148036820084940, -255.8751328056139585 ) ) ;
#72564 = CARTESIAN_POINT ( 'NONE',  ( -9.669690345268849185, -278.2846611672024437, -338.7904777536710412 ) ) ;
#72565 = CARTESIAN_POINT ( 'NONE',  ( -106.6398797693199754, -285.3368789335958695, -303.0072665436413217 ) ) ;
#72566 = CARTESIAN_POINT ( 'NONE',  ( -94.12204122672858375, -285.2012035854315855, -224.4611050949243349 ) ) ;
#72567 = CARTESIAN_POINT ( 'NONE',  ( -96.55642434655884188, -279.3696844236321226, -314.0742388105763325 ) ) ;
#72568 = CARTESIAN_POINT ( 'NONE',  ( -108.9206426547602007, -279.1557767770505620, -285.4957377086757333 ) ) ;
#72569 = EDGE_CURVE ( 'NONE', #54554, #55239, #15659, .T. ) ;
#72570 = CARTESIAN_POINT ( 'NONE',  ( -106.3759907889436676, -286.1676952669240563, -299.8071333148836288 ) ) ;
#72571 = ORIENTED_EDGE ( 'NONE', *, *, #68134, .T. ) ;
#72572 = CARTESIAN_POINT ( 'NONE',  ( -112.3062886209723246, -296.1648073402035948, -288.0053794569739125 ) ) ;
#72573 = CARTESIAN_POINT ( 'NONE',  ( 37.09415822743715552, -289.6124613335972526, -276.5941347606562317 ) ) ;
#72574 = CARTESIAN_POINT ( 'NONE',  ( 208.4306832106270804, -124.2391364535881024, 6.500000000000024869 ) ) ;
#72575 = CARTESIAN_POINT ( 'NONE',  ( 40.64545035920995986, -277.8376638359844719, -252.5284128619064461 ) ) ;
#72576 = ORIENTED_EDGE ( 'NONE', *, *, #30839, .F. ) ;
#72577 = CARTESIAN_POINT ( 'NONE',  ( 22.53031338191065558, -292.5892404096684913, -317.5178330610325474 ) ) ;
#72578 = CARTESIAN_POINT ( 'NONE',  ( -7.996478995075433360, -287.9638556434179577, -202.7625547549774865 ) ) ;
#72579 = CARTESIAN_POINT ( 'NONE',  ( -43.86239788051945254, -281.7288987808649949, -196.5846516963759143 ) ) ;
#72580 = CARTESIAN_POINT ( 'NONE',  ( 37.14116041450215988, -288.7618041610055570, -253.2470326521925585 ) ) ;
#72581 = CARTESIAN_POINT ( 'NONE',  ( 34.61440998920159018, -289.1994401457372419, -296.5079724830959549 ) ) ;
#72582 = CARTESIAN_POINT ( 'NONE',  ( -71.09274929014462430, -285.4976827031066478, -337.3520953439282266 ) ) ;
#72583 = CARTESIAN_POINT ( 'NONE',  ( -113.2988186932705190, -278.5608762988898661, -282.9910880453745676 ) ) ;
#72584 = ORIENTED_EDGE ( 'NONE', *, *, #34074, .F. ) ;
#72585 = CARTESIAN_POINT ( 'NONE',  ( -65.09772464383418367, -293.4918151325490498, -340.6525070171761627 ) ) ;
#72586 = CARTESIAN_POINT ( 'NONE',  ( 15.16288599107901547, -280.6019615119516857, -213.9653338154396920 ) ) ;
#72587 = CARTESIAN_POINT ( 'NONE',  ( -57.21469351174712159, -275.6535765551521422, -198.7817778015042620 ) ) ;
#72588 = CARTESIAN_POINT ( 'NONE',  ( 153.5041831715941782, 19.57420759269780319, 11.76949543550875354 ) ) ;
#72589 = CARTESIAN_POINT ( 'NONE',  ( 35.77081079830085031, -289.8376638359844719, -253.6410175316879361 ) ) ;
#72590 = AXIS2_PLACEMENT_3D ( 'NONE', #25163, #62087, #68728 ) ;
#72591 = CARTESIAN_POINT ( 'NONE',  ( -89.45142107969505219, -271.5703952154502190, -214.9851168817320684 ) ) ;
#72592 = DIRECTION ( 'NONE',  ( 0.000000000000000000, -1.000000000000000000, -0.000000000000000000 ) ) ;
#72593 = CARTESIAN_POINT ( 'NONE',  ( -104.4961695712554359, -278.4460939744859616, -241.5815127857250673 ) ) ;
#72594 = CARTESIAN_POINT ( 'NONE',  ( 37.20900640974227258, -276.9792854272424734, -288.0301875914694847 ) ) ;
#72595 = AXIS2_PLACEMENT_3D ( 'NONE', #92284, #36407, #42616 ) ;
#72596 = CARTESIAN_POINT ( 'NONE',  ( -90.48384561372591861, -298.7067987250415513, -219.3834844801939710 ) ) ;
#72597 = CARTESIAN_POINT ( 'NONE',  ( -38.74031533311053010, -282.1280457637220138, -347.1130827091283209 ) ) ;
#72598 = CARTESIAN_POINT ( 'NONE',  ( -97.36749464010824795, -291.7150028987358041, -313.6609795076416844 ) ) ;
#72599 = CARTESIAN_POINT ( 'NONE',  ( -36.92126781798521762, -299.5774404508446764, -194.0543399737223638 ) ) ;
#72600 = CARTESIAN_POINT ( 'NONE',  ( -48.92517658921273238, -299.1129439867789870, -194.5856578921626863 ) ) ;
#72601 = CARTESIAN_POINT ( 'NONE',  ( 20.26019253863147185, -296.2132047912186863, -318.1319290640575446 ) ) ;
#72602 = CARTESIAN_POINT ( 'NONE',  ( -92.09992261821246018, -281.8365326748772191, -321.3666617661593818 ) ) ;
#72603 = CARTESIAN_POINT ( 'NONE',  ( -96.55988284443661485, -290.8806004919076713, -221.1579155437943314 ) ) ;
#72604 = CARTESIAN_POINT ( 'NONE',  ( -94.14951462356270895, -271.2460666162605207, -221.9190971143331126 ) ) ;
#72605 = CARTESIAN_POINT ( 'NONE',  ( -62.95194199385857559, -287.3242735564728605, -198.5937442934177852 ) ) ;
#72606 = CARTESIAN_POINT ( 'NONE',  ( -96.81741606163974723, -288.8756490969257129, -313.2197844149259254 ) ) ;
#72607 = CARTESIAN_POINT ( 'NONE',  ( -76.51609685821101436, -209.3017665391693072, -356.9869174788681789 ) ) ;
#72608 = ORIENTED_EDGE ( 'NONE', *, *, #44755, .F. ) ;
#72609 = CARTESIAN_POINT ( 'NONE',  ( -89.10574573416242572, -288.3381346490827468, -326.5668994832099656 ) ) ;
#72610 = CARTESIAN_POINT ( 'NONE',  ( -3.360313273740507700, -288.2575124139892182, -335.0495605402925889 ) ) ;
#72611 = ORIENTED_EDGE ( 'NONE', *, *, #67910, .F. ) ;
#72612 = CARTESIAN_POINT ( 'NONE',  ( -73.47956238811100604, -286.6642240893996245, -202.6595034932258272 ) ) ;
#72613 = CARTESIAN_POINT ( 'NONE',  ( -89.09781327979187893, -278.1377930622334702, -321.9440039371183389 ) ) ;
#72614 = CARTESIAN_POINT ( 'NONE',  ( 23.77428276502948634, -293.0922129019433555, -316.6896097107490959 ) ) ;
#72615 = CARTESIAN_POINT ( 'NONE',  ( -81.49623364921241375, -284.2866546808349995, -333.3837363610172133 ) ) ;
#72616 = CARTESIAN_POINT ( 'NONE',  ( 38.94664176403490075, -283.0307116320295791, -267.0678165391638572 ) ) ;
#72617 = CARTESIAN_POINT ( 'NONE',  ( -5.460401608448171906, -282.9773602660387155, -340.4277084256985972 ) ) ;
#72618 = CARTESIAN_POINT ( 'NONE',  ( 34.58718658791602962, -281.7194969011699186, -257.7784814298119613 ) ) ;
#72619 = CARTESIAN_POINT ( 'NONE',  ( 161.5212002755277751, 220.3141551401068625, -205.3533786008646302 ) ) ;
#72620 = CARTESIAN_POINT ( 'NONE',  ( 178.9682605196512952, 254.2604872615934539, -166.3201451735521914 ) ) ;
#72621 = CARTESIAN_POINT ( 'NONE',  ( 83.45820220953470425, 82.29232363724392485, -299.0340934522332645 ) ) ;
#72622 = CARTESIAN_POINT ( 'NONE',  ( -71.97516272200695653, -272.7793929792926519, -205.8599289353179529 ) ) ;
#72623 = CARTESIAN_POINT ( 'NONE',  ( -79.44853104573034841, -295.1121907953627215, -334.7547643554154888 ) ) ;
#72624 = CARTESIAN_POINT ( 'NONE',  ( -11.83151317020731952, -92.77902702723882555, -356.4673753601988437 ) ) ;
#72625 = ADVANCED_FACE ( 'NONE', ( #83111 ), #75364, .F. ) ;
#72626 = CARTESIAN_POINT ( 'NONE',  ( -4.025619730384383921, -273.1671643557605762, -201.4748118082759163 ) ) ;
#72627 = CARTESIAN_POINT ( 'NONE',  ( -110.5776835635761017, -298.2551015922192619, -282.5001546655709603 ) ) ;
#72628 = EDGE_CURVE ( 'NONE', #36747, #59112, #52408, .T. ) ;
#72629 = CARTESIAN_POINT ( 'NONE',  ( -0.7313374559675888120, -289.8705152877921023, -334.1450890153101341 ) ) ;
#72630 = ORIENTED_EDGE ( 'NONE', *, *, #24839, .T. ) ;
#72631 = CARTESIAN_POINT ( 'NONE',  ( -50.41561929555482635, -296.1562796411411682, -346.0580913715991755 ) ) ;
#72632 = CARTESIAN_POINT ( 'NONE',  ( -81.52076531793906611, -285.9245920000120122, -212.1700650584869550 ) ) ;
#72633 = CARTESIAN_POINT ( 'NONE',  ( -92.93856628502165051, -272.1975345855373121, -217.5169543012414408 ) ) ;
#72634 = CARTESIAN_POINT ( 'NONE',  ( 39.49414499237111187, -294.3182804409632354, -267.4325367030131702 ) ) ;
#72635 = CARTESIAN_POINT ( 'NONE',  ( 37.72526998099149864, -294.2563479062197302, -287.2870475415577971 ) ) ;
#72636 = CARTESIAN_POINT ( 'NONE',  ( -87.93212010360555553, -291.4876291612071100, -217.6641788733667227 ) ) ;
#72637 = ORIENTED_EDGE ( 'NONE', *, *, #23802, .T. ) ;
#72638 = CARTESIAN_POINT ( 'NONE',  ( -43.94181038247550930, -275.8896270874741958, -195.0376113436787762 ) ) ;
#72639 = CARTESIAN_POINT ( 'NONE',  ( 35.35801304190726313, -274.0397283439281182, -246.0533773938741149 ) ) ;
#72640 = VERTEX_POINT ( 'NONE', #19200 ) ;
#72641 = CARTESIAN_POINT ( 'NONE',  ( -112.3403395174902357, -278.2746858806543742, -253.1933868178968794 ) ) ;
#72642 = CARTESIAN_POINT ( 'NONE',  ( 36.44315350027425637, -273.9325050280429537, -268.8658627906413017 ) ) ;
#72643 = CARTESIAN_POINT ( 'NONE',  ( -43.52183335250149554, -275.0520673500969338, -197.2620434942434144 ) ) ;
#72644 = CARTESIAN_POINT ( 'NONE',  ( 26.97912606564017679, -276.9711285845758084, -305.4848690527435338 ) ) ;
#72645 = CARTESIAN_POINT ( 'NONE',  ( -40.42847179124874657, -299.6142133325463988, -194.1720776783739950 ) ) ;
#72646 = CARTESIAN_POINT ( 'NONE',  ( 17.68453685504397299, -274.2898273730569940, -321.8443195779528310 ) ) ;
#72647 = CARTESIAN_POINT ( 'NONE',  ( -102.8558341196655732, -296.7631799731530577, -302.9068089170913254 ) ) ;
#72648 = CARTESIAN_POINT ( 'NONE',  ( -41.08721893353986587, -293.6749017781283442, -343.8676367511934018 ) ) ;
#72649 = CARTESIAN_POINT ( 'NONE',  ( 199.4565688755349981, 40.19734553069211103, 10.50000000000000888 ) ) ;
#72650 = CARTESIAN_POINT ( 'NONE',  ( -111.2798458314029659, -279.3114653483224856, -249.0848985517635583 ) ) ;
#72651 = CARTESIAN_POINT ( 'NONE',  ( 19.85417795680242392, -275.0783346835104339, -224.9799936443723425 ) ) ;
#72652 = CARTESIAN_POINT ( 'NONE',  ( -82.96826716633719911, -284.1275919621877506, -208.8824062727275077 ) ) ;
#72653 = CARTESIAN_POINT ( 'NONE',  ( -104.8775391835034014, -298.9863765758392447, -237.3620442603397578 ) ) ;
#72654 = DIRECTION ( 'NONE',  ( 0.000000000000000000, 1.000000000000000000, 0.000000000000000000 ) ) ;
#72655 = CARTESIAN_POINT ( 'NONE',  ( -99.74171250033620595, -284.2756170267631433, -232.0698491973785735 ) ) ;
#72656 = CARTESIAN_POINT ( 'NONE',  ( -109.7608660887781014, -276.5932177258724209, -285.6398096063447838 ) ) ;
#72657 = CARTESIAN_POINT ( 'NONE',  ( -21.54408018272725300, -275.4204838017519137, -342.2870973895800262 ) ) ;
#72659 = CARTESIAN_POINT ( 'NONE',  ( -4.491375455754583967, -284.6194807504754181, -337.7980639928842379 ) ) ;
#72658 = TOROIDAL_SURFACE ( 'NONE', #4583, 12.40608546931776957, 1.000000000000000000 ) ;
#72660 = CARTESIAN_POINT ( 'NONE',  ( 35.01452081217395573, -276.5946514338101565, -257.9695860609151623 ) ) ;
#72661 = ADVANCED_FACE ( 'NONE', ( #69387 ), #39819, .T. ) ;
#72662 = CARTESIAN_POINT ( 'NONE',  ( 154.4590814691937624, 20.78850955392830357, 13.92316269558947539 ) ) ;
#72663 = CARTESIAN_POINT ( 'NONE',  ( 37.94046176882081056, -273.8019471926983783, -258.4854946276341821 ) ) ;
#72664 = VECTOR ( 'NONE', #31917, 1000.000000000000000 ) ;
#72665 = CARTESIAN_POINT ( 'NONE',  ( -74.13335367105617024, -281.5645111751994136, -204.8141679600256850 ) ) ;
#72666 = CARTESIAN_POINT ( 'NONE',  ( 196.8803347170859865, 73.40565171261609123, 12.49999999999999289 ) ) ;
#72667 = CARTESIAN_POINT ( 'NONE',  ( 18.57537894557212610, -290.1762498905588359, -321.1996306617678556 ) ) ;
#72668 = CARTESIAN_POINT ( 'NONE',  ( 24.30966394850093693, -292.1314378457955740, -313.0929279872260054 ) ) ;
#72669 = DIRECTION ( 'NONE',  ( -0.000000000000000000, 1.000000000000000000, -0.000000000000000000 ) ) ;
#72670 = CARTESIAN_POINT ( 'NONE',  ( -65.71210231118379852, -296.4675217324693790, -202.6687935621388306 ) ) ;
#72671 = CARTESIAN_POINT ( 'NONE',  ( -73.20321590351130681, -289.7113434673329380, -205.3047678917250494 ) ) ;
#72672 = CARTESIAN_POINT ( 'NONE',  ( -111.8439089875458023, -277.9397250554267202, -284.5643135594219189 ) ) ;
#72673 = CARTESIAN_POINT ( 'NONE',  ( -67.60359018049207691, -295.6549983607338845, -201.7233188019406782 ) ) ;
#72674 = CARTESIAN_POINT ( 'NONE',  ( -15.17234992714933561, -287.2501807962000839, -343.4316190599973879 ) ) ;
#72675 = CARTESIAN_POINT ( 'NONE',  ( -2.028130870471564151, -284.1764967702965805, -335.1782835905693787 ) ) ;
#72676 = CARTESIAN_POINT ( 'NONE',  ( -49.16465440331155889, -284.1434735829894294, -195.2468375549695452 ) ) ;
#72677 = CARTESIAN_POINT ( 'NONE',  ( -6.994032904470032896, -284.0712237367500848, -337.4151858539075874 ) ) ;
#72678 = CARTESIAN_POINT ( 'NONE',  ( -80.71366044929442296, -284.4601327357931950, -329.3433649550614746 ) ) ;
#72679 = CARTESIAN_POINT ( 'NONE',  ( -106.2175352299979494, -292.1319217335318967, -301.0593786139695567 ) ) ;
#72680 = CARTESIAN_POINT ( 'NONE',  ( -38.36138943496778353, -274.3729763839149314, -193.3890157287981708 ) ) ;
#72681 = CARTESIAN_POINT ( 'NONE',  ( -110.5333982167679778, -288.3920446292280531, -289.1823228490201814 ) ) ;
#72682 = CARTESIAN_POINT ( 'NONE',  ( -102.0969893335362002, -278.0044214041092800, -312.1207748972948934 ) ) ;
#72683 = CARTESIAN_POINT ( 'NONE',  ( 19.23523255358808726, -296.2103464493407046, -319.0724779203311527 ) ) ;
#72684 = LINE ( 'NONE', #87333, #86292 ) ;
#72685 = CARTESIAN_POINT ( 'NONE',  ( 209.8616357346608936, 36.89613957940315458, 12.09245862095555779 ) ) ;
#72686 = CARTESIAN_POINT ( 'NONE',  ( -48.41943294058848579, -281.8809335630779174, -343.0145921786399299 ) ) ;
#72687 = CARTESIAN_POINT ( 'NONE',  ( -111.2673279605176759, -276.3768176437554303, -284.0345360605514315 ) ) ;
#72688 = CARTESIAN_POINT ( 'NONE',  ( -112.3828400292837273, -271.2102467711956137, -256.2397729456131401 ) ) ;
#72689 = CARTESIAN_POINT ( 'NONE',  ( -5.028484675708946305, -275.9637644424725522, -335.9474968275684432 ) ) ;
#72690 = CARTESIAN_POINT ( 'NONE',  ( -64.34350742637757037, -293.2134153304747883, -201.7791664698164595 ) ) ;
#72691 = CARTESIAN_POINT ( 'NONE',  ( 32.97945695563360857, -294.7636269776970153, -290.8596603395666307 ) ) ;
#72692 = CARTESIAN_POINT ( 'NONE',  ( 38.26613518709703499, -294.8337160385650009, -258.9585248358236527 ) ) ;
#72693 = CARTESIAN_POINT ( 'NONE',  ( 31.79163058365386973, -295.2913694723740150, -303.2547929590451190 ) ) ;
#72694 = CARTESIAN_POINT ( 'NONE',  ( -100.1675541633565132, -295.8734854955789046, -307.6347335298187318 ) ) ;
#72695 = CARTESIAN_POINT ( 'NONE',  ( -15.23856689835864664, -290.7662682545058601, -342.0844431101372720 ) ) ;
#72696 = CARTESIAN_POINT ( 'NONE',  ( -99.78723085027833406, -284.1204814658040050, -315.5008100114276317 ) ) ;
#72697 = CARTESIAN_POINT ( 'NONE',  ( -64.43587502152126945, -271.8418671105007434, -199.5925777300951722 ) ) ;
#72698 = CARTESIAN_POINT ( 'NONE',  ( -35.14611011754089986, -285.9122939627697519, -193.3792836050163260 ) ) ;
#72699 = CARTESIAN_POINT ( 'NONE',  ( -46.07608554803450573, -279.1432289929468311, -344.5449098422316752 ) ) ;
#72700 = CARTESIAN_POINT ( 'NONE',  ( -99.93999509964166350, -283.8734386798907394, -231.9422072200140406 ) ) ;
#72701 = CARTESIAN_POINT ( 'NONE',  ( -109.6215082978459634, -288.2945442657234594, -290.3768613297563661 ) ) ;
#72702 = CARTESIAN_POINT ( 'NONE',  ( -22.77999168687133391, -278.3760220647245092, -195.9554462355543194 ) ) ;
#72703 = CARTESIAN_POINT ( 'NONE',  ( -78.59295187722810283, -208.2960365483323244, -357.4574221067172743 ) ) ;
#72704 = CARTESIAN_POINT ( 'NONE',  ( -105.6202170683752541, -284.4066648466970832, -244.3604917212543910 ) ) ;
#72705 = CARTESIAN_POINT ( 'NONE',  ( 12.72102239935743562, -281.9376762649483226, -212.3806684269877110 ) ) ;
#72706 = CARTESIAN_POINT ( 'NONE',  ( -75.55697911132457989, -288.6078432237277980, -336.9374851502971069 ) ) ;
#72707 = CARTESIAN_POINT ( 'NONE',  ( -51.14747050546461793, -278.8259245745310864, -345.3000338929620057 ) ) ;
#72708 = CARTESIAN_POINT ( 'NONE',  ( -39.92938971463601661, -278.3991618759394555, -346.8371776259054968 ) ) ;
#72709 = CARTESIAN_POINT ( 'NONE',  ( -57.11117175625147269, -279.6232099540412719, -200.0890182841114893 ) ) ;
#72710 = CARTESIAN_POINT ( 'NONE',  ( -94.18229758850212363, -275.2052107901574800, -221.9575668034076728 ) ) ;
#72711 = CARTESIAN_POINT ( 'NONE',  ( 22.20925851149811692, -292.8966693147658589, -221.5483806580962209 ) ) ;
#72712 = CARTESIAN_POINT ( 'NONE',  ( -81.39817350995882350, -287.6742818801649264, -330.6821868511964340 ) ) ;
#72713 = CARTESIAN_POINT ( 'NONE',  ( -99.39157657486194353, -292.7442151106627648, -226.1315662186328552 ) ) ;
#72714 = CARTESIAN_POINT ( 'NONE',  ( -108.6027320246684269, -295.2457476494138291, -287.6214016828461126 ) ) ;
#72715 = CARTESIAN_POINT ( 'NONE',  ( 34.73549899882192449, -293.0634980774637484, -258.5797030023960588 ) ) ;
#72716 = CARTESIAN_POINT ( 'NONE',  ( -81.76257180806857150, -292.5423133271952452, -207.8448907438060758 ) ) ;
#72717 = CARTESIAN_POINT ( 'NONE',  ( 33.85778561786663943, -281.9852975541580804, -253.7922949074904579 ) ) ;
#72718 = CARTESIAN_POINT ( 'NONE',  ( -36.53081718739017703, -296.9824153312136445, -193.6703720887663280 ) ) ;
#72719 = CARTESIAN_POINT ( 'NONE',  ( -26.15118692841940984, -289.5646579613576819, -346.4405843363378494 ) ) ;
#72720 = CARTESIAN_POINT ( 'NONE',  ( -78.50876869752676157, -281.7396319832358813, -333.9659758506107892 ) ) ;
#72721 = EDGE_CURVE ( 'NONE', #16234, #41846, #64101, .T. ) ;
#72722 = CARTESIAN_POINT ( 'NONE',  ( -74.41341025751604832, -289.8645498355145378, -337.8404730962463987 ) ) ;
#72723 = CARTESIAN_POINT ( 'NONE',  ( -74.73458058308284535, -285.8727505285902453, -207.6406270880269460 ) ) ;
#72724 = DIRECTION ( 'NONE',  ( 0.000000000000000000, 1.000000000000000000, 0.000000000000000000 ) ) ;
#72725 = CARTESIAN_POINT ( 'NONE',  ( 191.9735245738955882, 278.3896920391067056, -124.9451965857499545 ) ) ;
#72726 = CARTESIAN_POINT ( 'NONE',  ( 201.7739257888548252, 292.3635967676956398, -68.22063874808750938 ) ) ;
#72727 = AXIS2_PLACEMENT_3D ( 'NONE', #21942, #7713, #8634 ) ;
#72728 = CARTESIAN_POINT ( 'NONE',  ( -89.58173318462191048, -278.4898060840101834, -219.0684315871032197 ) ) ;
#72729 = CARTESIAN_POINT ( 'NONE',  ( -59.81537445235002082, -278.6745003950895807, -200.5282240395157771 ) ) ;
#72730 = CARTESIAN_POINT ( 'NONE',  ( -0.05196895205309185611, -274.2010611771019626, -203.0020846880323404 ) ) ;
#72731 = CARTESIAN_POINT ( 'NONE',  ( -81.44234294714043187, -220.1383413502173880, -350.5104082359922586 ) ) ;
#72732 = EDGE_CURVE ( 'NONE', #68047, #78471, #48060, .T. ) ;
#72733 = CARTESIAN_POINT ( 'NONE',  ( -67.11599319349446091, -278.2441150999017623, -199.9899749891582417 ) ) ;
#72734 = CARTESIAN_POINT ( 'NONE',  ( -93.81978916493524423, -281.8920391718664860, -319.1870551757857015 ) ) ;
#72735 = CARTESIAN_POINT ( 'NONE',  ( -3.657551686419955761, -296.3739910336841490, -338.4883214400276188 ) ) ;
#72736 = CARTESIAN_POINT ( 'NONE',  ( -98.35438193625856229, -291.6025410122605876, -230.0766589644921680 ) ) ;
#72737 = CARTESIAN_POINT ( 'NONE',  ( -45.43326582176418071, -287.8416417169724468, -343.4074734170818601 ) ) ;
#72738 = CARTESIAN_POINT ( 'NONE',  ( -5.164482450790024437, -275.1160748727232885, -200.5188711000733122 ) ) ;
#72739 = CARTESIAN_POINT ( 'NONE',  ( -93.94119895680513821, -296.0660350180558567, -316.4838732051413217 ) ) ;
#72740 = ORIENTED_EDGE ( 'NONE', *, *, #40929, .F. ) ;
#72741 = CARTESIAN_POINT ( 'NONE',  ( 175.2296996224749250, 275.0000000000000568, -24.99999999999999289 ) ) ;
#72742 = CARTESIAN_POINT ( 'NONE',  ( -112.7927560803320830, -280.4206131454601518, -274.4172677843751558 ) ) ;
#72743 = CARTESIAN_POINT ( 'NONE',  ( -1.828323632045869118, -281.6141527805297642, -206.2282390209307721 ) ) ;
#72744 = CARTESIAN_POINT ( 'NONE',  ( -112.2958742488556823, -280.1540801664331752, -282.8449393693487650 ) ) ;
#72745 = CARTESIAN_POINT ( 'NONE',  ( -18.68723514664256413, -281.8648372545962388, -341.2333140471280331 ) ) ;
#72746 = CARTESIAN_POINT ( 'NONE',  ( 12.02521229381300572, -273.2329020383918987, -215.5784457234925640 ) ) ;
#72747 = DIRECTION ( 'NONE',  ( 0.000000000000000000, 1.000000000000000000, 0.000000000000000000 ) ) ;
#72748 = LINE ( 'NONE', #65679, #56238 ) ;
#72749 = CARTESIAN_POINT ( 'NONE',  ( 18.79224306375114040, -277.0721031080080365, -322.8314833540257496 ) ) ;
#72750 = VERTEX_POINT ( 'NONE', #32482 ) ;
#72751 = CARTESIAN_POINT ( 'NONE',  ( 33.82390975394172727, -277.2444477822796216, -246.5236143311895489 ) ) ;
#72752 = CARTESIAN_POINT ( 'NONE',  ( -51.22351806067383251, -275.8010109056640999, -345.5003315948738418 ) ) ;
#72753 = ORIENTED_EDGE ( 'NONE', *, *, #23679, .F. ) ;
#72754 = DIRECTION ( 'NONE',  ( -0.000000000000000000, -0.000000000000000000, 1.000000000000000000 ) ) ;
#72755 = CARTESIAN_POINT ( 'NONE',  ( -109.1111539952250951, -286.2364724873730779, -293.3721318079574871 ) ) ;
#72756 = CARTESIAN_POINT ( 'NONE',  ( -7.194386846226396237, -291.6552219792573624, -203.6997256379168277 ) ) ;
#72757 = CARTESIAN_POINT ( 'NONE',  ( 33.76833694114049678, -286.5267394708469055, -240.9529536600720974 ) ) ;
#72758 = CARTESIAN_POINT ( 'NONE',  ( -109.7156170244136888, -282.5896632547243712, -285.9130119237511849 ) ) ;
#72760 = CARTESIAN_POINT ( 'NONE',  ( 32.33085845630967725, -285.2872847148469191, -244.0038636518765145 ) ) ;
#72759 = CARTESIAN_POINT ( 'NONE',  ( -80.99010622357680234, -282.2323864183447881, -329.6713975624234081 ) ) ;
#72761 = CARTESIAN_POINT ( 'NONE',  ( -8.323208108905429725, -283.8685871247024011, -337.7781605352935230 ) ) ;
#72762 = CARTESIAN_POINT ( 'NONE',  ( -13.66897461514133383, -272.3592773133695459, -199.1950957955571937 ) ) ;
#72763 = CARTESIAN_POINT ( 'NONE',  ( -93.31806661614903931, -283.6640859793865843, -218.5819076144867665 ) ) ;
#72764 = CARTESIAN_POINT ( 'NONE',  ( -112.1286995360680265, -298.6331651887081193, -264.0644008026904999 ) ) ;
#72765 = CARTESIAN_POINT ( 'NONE',  ( -64.91578699423818932, -280.6241501027257073, -202.5151292883427629 ) ) ;
#72766 = CARTESIAN_POINT ( 'NONE',  ( -88.65379263049631220, -287.3348173322237358, -215.3621891257582774 ) ) ;
#72767 = DIRECTION ( 'NONE',  ( 0.000000000000000000, 0.000000000000000000, 1.000000000000000000 ) ) ;
#72768 = DIRECTION ( 'NONE',  ( -0.7957555401921980742, -0.6056179655966482667, 0.000000000000000000 ) ) ;
#72769 = CARTESIAN_POINT ( 'NONE',  ( 35.68445224958905726, -295.2241710157894090, -250.9077759206547285 ) ) ;
#72770 = CARTESIAN_POINT ( 'NONE',  ( -77.44622426448674446, -275.5895855807585804, -333.7990799351396163 ) ) ;
#72771 = CARTESIAN_POINT ( 'NONE',  ( -57.25892217699154685, -288.4998490426477247, -344.6283936932735514 ) ) ;
#72772 = CARTESIAN_POINT ( 'NONE',  ( 33.51259369878102490, -292.2226569974388326, -291.0489143048235974 ) ) ;
#72773 = CARTESIAN_POINT ( 'NONE',  ( -109.5308292116296087, -277.0555008853965546, -284.2107635596270256 ) ) ;
#72774 = CARTESIAN_POINT ( 'NONE',  ( -111.2782920302880001, -294.7851883511885376, -263.1566089504992760 ) ) ;
#72775 = CARTESIAN_POINT ( 'NONE',  ( -41.63830181620294013, -293.3122229488282073, -196.9434854874232599 ) ) ;
#72776 = CARTESIAN_POINT ( 'NONE',  ( -4.829096099716510437, -276.9805209788416391, -202.7746430608542312 ) ) ;
#72777 = CARTESIAN_POINT ( 'NONE',  ( -76.74098044987496792, -294.0489582041214476, -335.7709305526648222 ) ) ;
#72778 = CARTESIAN_POINT ( 'NONE',  ( 34.79696273316833555, -289.3561883829402177, -285.9913912323960972 ) ) ;
#72779 = CARTESIAN_POINT ( 'NONE',  ( -110.5714814780118047, -288.5345247329788094, -290.6434536131768596 ) ) ;
#72780 = CARTESIAN_POINT ( 'NONE',  ( 14.51133573259076925, -289.7301019903147790, -322.5783334252406007 ) ) ;
#72781 = CARTESIAN_POINT ( 'NONE',  ( 200.4644824113734671, 250.5000000000000568, -2.942835885954290021 ) ) ;
#72782 = CARTESIAN_POINT ( 'NONE',  ( -98.23942683986632574, -290.7930844619075401, -310.9310364460142182 ) ) ;
#72783 = LINE ( 'NONE', #7908, #91363 ) ;
#72784 = CARTESIAN_POINT ( 'NONE',  ( -7.062681113594275750, -289.8687120359217033, -340.7399770864576567 ) ) ;
#72785 = CARTESIAN_POINT ( 'NONE',  ( -14.69747092412048595, -278.3641297292050467, -198.4339793144716850 ) ) ;
#72786 = CARTESIAN_POINT ( 'NONE',  ( -82.22996982939004340, -279.7913096560416193, -207.8248282407932663 ) ) ;
#72787 = VECTOR ( 'NONE', #15062, 1000.000000000000000 ) ;
#72788 = CARTESIAN_POINT ( 'NONE',  ( 25.91053145502498722, -281.7988824034962363, -314.2579755673482964 ) ) ;
#72789 = CARTESIAN_POINT ( 'NONE',  ( 37.68168330610299677, -285.5252883469739231, -268.2817470021191752 ) ) ;
#72790 = DIRECTION ( 'NONE',  ( 0.000000000000000000, 0.000000000000000000, 1.000000000000000000 ) ) ;
#72791 = CARTESIAN_POINT ( 'NONE',  ( 14.20963097909127804, -278.9248101955988659, -216.8729293222980061 ) ) ;
#72792 = CARTESIAN_POINT ( 'NONE',  ( -89.07745193319594534, -281.7789361043462009, -324.7316401023517756 ) ) ;
#72793 = CARTESIAN_POINT ( 'NONE',  ( 153.6987871352777404, 19.48326534539592458, 11.45812909364015297 ) ) ;
#72794 = CARTESIAN_POINT ( 'NONE',  ( -105.7326466465223263, -276.5917805852744209, -304.3236144910305825 ) ) ;
#72795 = CARTESIAN_POINT ( 'NONE',  ( -93.68326502999310890, -284.1844589753897026, -218.2533082595517442 ) ) ;
#72796 = CARTESIAN_POINT ( 'NONE',  ( -40.54020606039571106, -298.9522361910534869, -197.1831134738568494 ) ) ;
#72797 = CARTESIAN_POINT ( 'NONE',  ( -80.00965940080263294, -293.0645425674039757, -210.0831407724429027 ) ) ;
#72798 = CARTESIAN_POINT ( 'NONE',  ( -3.697203440359453364, -299.7802514347591227, -193.8469198602112442 ) ) ;
#72799 = CARTESIAN_POINT ( 'NONE',  ( 32.53538869069117823, -275.4999698196624536, -291.6006793084644073 ) ) ;
#72800 = CARTESIAN_POINT ( 'NONE',  ( -12.31756191903461328, -296.7269406582806823, -341.1179870220809107 ) ) ;
#72801 = CARTESIAN_POINT ( 'NONE',  ( -97.28873851984336341, -290.0707921930952011, -318.7073966601080883 ) ) ;
#72802 = CARTESIAN_POINT ( 'NONE',  ( 37.00423617923385677, -279.8048493502550400, -283.9234460782151359 ) ) ;
#72803 = CARTESIAN_POINT ( 'NONE',  ( 26.49409145742661664, -292.8170659981735753, -227.2093164448088487 ) ) ;
#72804 = CARTESIAN_POINT ( 'NONE',  ( -96.75650345722364420, -289.0140461432455368, -313.1780491418830366 ) ) ;
#72805 = CARTESIAN_POINT ( 'NONE',  ( -5.378620047332675291, -292.6314885091609312, -338.2232907747255126 ) ) ;
#72806 = ORIENTED_EDGE ( 'NONE', *, *, #15662, .F. ) ;
#72807 = CARTESIAN_POINT ( 'NONE',  ( 154.9842916688209868, 275.0000000000000568, -12.88888888888890882 ) ) ;
#72808 = CARTESIAN_POINT ( 'NONE',  ( -110.4291984882819406, -290.0849398905399994, -268.4539024029337497 ) ) ;
#72809 = CARTESIAN_POINT ( 'NONE',  ( 9.339199855150262408, -282.8906705383787994, 74.50000000000001421 ) ) ;
#72810 = CARTESIAN_POINT ( 'NONE',  ( -73.51277607011510895, -286.5258270450058262, -202.5935002401162421 ) ) ;
#72811 = CARTESIAN_POINT ( 'NONE',  ( -67.74223827176244583, -294.1233781216987495, -207.3071070584150277 ) ) ;
#72812 = CARTESIAN_POINT ( 'NONE',  ( -4.613761650278911830, -293.6902255782867428, -339.8140205573930075 ) ) ;
#72813 = CARTESIAN_POINT ( 'NONE',  ( 4.291474855843541825, -283.8189811163575769, -334.6107874504319284 ) ) ;
#72814 = CARTESIAN_POINT ( 'NONE',  ( -95.76466535220404808, -284.9998614853337244, -226.5917549651722140 ) ) ;
#72815 = CARTESIAN_POINT ( 'NONE',  ( 22.67393365139516703, -276.2789273492726352, -227.9203913018577055 ) ) ;
#72816 = CARTESIAN_POINT ( 'NONE',  ( -39.76718585308042719, -293.1028433265271929, -344.9792155617773233 ) ) ;
#72817 = CARTESIAN_POINT ( 'NONE',  ( 36.09587323923904023, -274.3634149236244184, -271.6069373902695361 ) ) ;
#72818 = EDGE_LOOP ( 'NONE', ( #41016, #61106, #17035, #52208 ) ) ;
#72819 = EDGE_CURVE ( 'NONE', #64529, #85520, #61379, .T. ) ;
#72820 = CARTESIAN_POINT ( 'NONE',  ( 196.1981356858130425, 40.87848184507377880, 13.11514447343857981 ) ) ;
#72821 = CARTESIAN_POINT ( 'NONE',  ( -0.7199747513541546740, -294.2460677926919743, -338.0856253332792676 ) ) ;
#72822 = CARTESIAN_POINT ( 'NONE',  ( 33.19748600952929962, -289.1624936713531611, -246.5800873834269282 ) ) ;
#72823 = CARTESIAN_POINT ( 'NONE',  ( -109.5644004111295402, -297.9587339726267601, -244.5662721191335436 ) ) ;
#72824 = CARTESIAN_POINT ( 'NONE',  ( 30.05252867172026043, -287.8225472969218117, -241.9120375200736817 ) ) ;
#72825 = EDGE_CURVE ( 'NONE', #48357, #64930, #56517, .T. ) ;
#72826 = CARTESIAN_POINT ( 'NONE',  ( -112.4847428916724112, -277.8085886051226225, -254.6024475216803751 ) ) ;
#72827 = CARTESIAN_POINT ( 'NONE',  ( -81.80599152132158736, -296.2913906368955850, -333.1656076759642815 ) ) ;
#72828 = CARTESIAN_POINT ( 'NONE',  ( -70.12637761404209868, -287.6189855326091447, -338.6796219301734254 ) ) ;
#72829 = CARTESIAN_POINT ( 'NONE',  ( -107.1454133446231793, -296.4699679027177694, -302.8139439399148500 ) ) ;
#72830 = CARTESIAN_POINT ( 'NONE',  ( -4.827476657401152060, -292.8258111386011251, -204.9643726217158246 ) ) ;
#72831 = DIRECTION ( 'NONE',  ( 1.000000000000000000, 0.000000000000000000, 0.000000000000000000 ) ) ;
#72832 = CARTESIAN_POINT ( 'NONE',  ( 60.30377782462291236, -249.1633071459562245, 22.50000000000000000 ) ) ;
#72833 = CARTESIAN_POINT ( 'NONE',  ( 161.3931422173053249, 217.5860020223464630, -202.5160790843344500 ) ) ;
#72834 = CARTESIAN_POINT ( 'NONE',  ( 11.61776537017173183, -288.2371227443646831, -211.7628872388046659 ) ) ;
#72835 = CARTESIAN_POINT ( 'NONE',  ( -37.30987171927208834, -289.5523547857346784, -190.3611179825600175 ) ) ;
#72836 = VERTEX_POINT ( 'NONE', #67992 ) ;
#72837 = CARTESIAN_POINT ( 'NONE',  ( -17.01094650526230012, -279.6565829699431447, -196.1993135046544978 ) ) ;
#72838 = CARTESIAN_POINT ( 'NONE',  ( -81.69270557300031044, -285.6572679393446492, -330.7000851468633300 ) ) ;
#72839 = CARTESIAN_POINT ( 'NONE',  ( -104.9025625061584464, -283.5926130349020582, -234.5528345699403303 ) ) ;
#72840 = CARTESIAN_POINT ( 'NONE',  ( 22.31309839122275207, -286.2449531403032097, -314.9090593353636223 ) ) ;
#72841 = CARTESIAN_POINT ( 'NONE',  ( 19.09960526085329136, -276.7151387656413135, -219.7401610571842241 ) ) ;
#72842 = CARTESIAN_POINT ( 'NONE',  ( -81.98667224417084753, -297.9173867170221683, -212.4626196692436793 ) ) ;
#72843 = CARTESIAN_POINT ( 'NONE',  ( 21.71281251067375351, -292.8462644033361926, -314.1082094983529487 ) ) ;
#72844 = CARTESIAN_POINT ( 'NONE',  ( -96.74399494036289582, -279.8605757033813006, -221.5074523464344054 ) ) ;
#72846 = CARTESIAN_POINT ( 'NONE',  ( -109.7215378930284544, -278.0403781914830006, -259.7606838162875533 ) ) ;
#72845 = CARTESIAN_POINT ( 'NONE',  ( -51.28088489548370177, -277.2353657018302897, -342.0179329272686459 ) ) ;
#72847 = CARTESIAN_POINT ( 'NONE',  ( -32.71504482354093568, -275.1888127968763342, -193.7968178094361349 ) ) ;
#72848 = CARTESIAN_POINT ( 'NONE',  ( -48.46280659700573779, -276.1107419331834194, -346.2950548609296106 ) ) ;
#72849 = CARTESIAN_POINT ( 'NONE',  ( -95.90218042510922203, -239.8047343563239906, -341.6332487328612615 ) ) ;
#72850 = CARTESIAN_POINT ( 'NONE',  ( -35.06784298841319725, -275.0234667435146321, -345.3392106192002302 ) ) ;
#72851 = EDGE_CURVE ( 'NONE', #26459, #91019, #41319, .T. ) ;
#72852 = CARTESIAN_POINT ( 'NONE',  ( -113.1920869093001585, -298.0938358568027979, -261.1239583833628330 ) ) ;
#72853 = CARTESIAN_POINT ( 'NONE',  ( 21.31550574532285580, -278.6948066931273615, -317.0979686699210447 ) ) ;
#72854 = TOROIDAL_SURFACE ( 'NONE', #53172, 4.499999999999990230, 0.5000000000000000000 ) ;
#72855 = CARTESIAN_POINT ( 'NONE',  ( 65.71450562203199297, 45.78484130816451625, -315.1169351998001389 ) ) ;
#72856 = AXIS2_PLACEMENT_3D ( 'NONE', #9524, #73016, #8599 ) ;
#72857 = CARTESIAN_POINT ( 'NONE',  ( -79.49822820460157402, -286.5477384608152533, -210.3233512628877691 ) ) ;
#72858 = CARTESIAN_POINT ( 'NONE',  ( -100.1714248532217084, -286.8844126864483997, -227.5317330673458116 ) ) ;
#72859 = CARTESIAN_POINT ( 'NONE',  ( 2.509519063279600282, -285.9506782573768646, -209.0767562171938039 ) ) ;
#72860 = CARTESIAN_POINT ( 'NONE',  ( -110.7015735226289479, -276.8410931493526164, -278.8619500997134537 ) ) ;
#72861 = CARTESIAN_POINT ( 'NONE',  ( -100.0621680825726116, -285.8717648333191050, -310.1688694095292362 ) ) ;
#72862 = CARTESIAN_POINT ( 'NONE',  ( -92.71675402643796815, -277.7197443720456249, -221.7177449714219790 ) ) ;
#72863 = CARTESIAN_POINT ( 'NONE',  ( -37.79611087004261094, -278.3731007715740020, -343.8654030349177901 ) ) ;
#72864 = CARTESIAN_POINT ( 'NONE',  ( 33.64781523500835192, -276.2728844942318460, -287.6903298064727323 ) ) ;
#72865 = CARTESIAN_POINT ( 'NONE',  ( 39.24340640033333472, -286.3263062569518524, -268.7087937074405204 ) ) ;
#72866 = AXIS2_PLACEMENT_3D ( 'NONE', #63852, #42491, #21667 ) ;
#72867 = CARTESIAN_POINT ( 'NONE',  ( 3.727008315224979551, -281.3922982625654186, -205.3558374599040235 ) ) ;
#72868 = CARTESIAN_POINT ( 'NONE',  ( 31.02533418221001682, -282.4997674295435104, -305.6524132644659062 ) ) ;
#72869 = ORIENTED_EDGE ( 'NONE', *, *, #68018, .F. ) ;
#72870 = ORIENTED_EDGE ( 'NONE', *, *, #1142, .F. ) ;
#72871 = ADVANCED_FACE ( 'NONE', ( #11156, #40017 ), #3120, .T. ) ;
#72872 = DIRECTION ( 'NONE',  ( -5.501794166262391869E-14, -0.01273136352371387336, 0.9999189529070978688 ) ) ;
#72873 = CARTESIAN_POINT ( 'NONE',  ( -36.08321065769175817, -290.8969748645503728, -346.1283686582925725 ) ) ;
#72874 = CARTESIAN_POINT ( 'NONE',  ( -104.1710195045417606, -289.7229458616542956, -233.1167849466729649 ) ) ;
#72875 = CARTESIAN_POINT ( 'NONE',  ( -33.45504803521652804, -296.6041469108583328, -346.4749179285185505 ) ) ;
#72876 = CARTESIAN_POINT ( 'NONE',  ( -41.86814187491255268, -297.1908200787846113, -197.3397988196830397 ) ) ;
#72877 = CARTESIAN_POINT ( 'NONE',  ( -11.18011930742364690, -291.7327735019198371, -197.9941258714229377 ) ) ;
#72878 = CARTESIAN_POINT ( 'NONE',  ( 22.56642320430477611, -285.4368467842198811, -227.3597378230043091 ) ) ;
#72879 = CARTESIAN_POINT ( 'NONE',  ( 21.50096932750649970, -289.3696776354869939, -314.2532319823305897 ) ) ;
#72880 = CARTESIAN_POINT ( 'NONE',  ( -69.91165696735023971, -288.1233781216987495, -202.8022627189028810 ) ) ;
#72881 = CARTESIAN_POINT ( 'NONE',  ( -2.701219136153005351, -290.5942469076187535, -336.8820750439425069 ) ) ;
#72882 = CARTESIAN_POINT ( 'NONE',  ( -81.78955137494219230, -287.6558560713782526, -330.9780870856083652 ) ) ;
#72883 = CARTESIAN_POINT ( 'NONE',  ( -68.83941802020008538, -291.4663706477062988, -338.4403842650248180 ) ) ;
#72884 = CARTESIAN_POINT ( 'NONE',  ( -103.7037371727642494, -285.9117644680385979, -239.2652485834057927 ) ) ;
#72885 = CARTESIAN_POINT ( 'NONE',  ( -109.8706853286312963, -292.8061080240303227, -250.5745675780537454 ) ) ;
#72886 = CARTESIAN_POINT ( 'NONE',  ( -48.18343439339133027, -296.0521521680024080, -430.6442049081568939 ) ) ;
#72887 = DIRECTION ( 'NONE',  ( -0.000000000000000000, -0.000000000000000000, -1.000000000000000000 ) ) ;
#72888 = CARTESIAN_POINT ( 'NONE',  ( -106.5764924421242199, -274.9207630375488520, -240.4809386914803326 ) ) ;
#72889 = CARTESIAN_POINT ( 'NONE',  ( -38.89874539361407102, -282.2693099806596138, -343.5185427964374298 ) ) ;
#72890 = CARTESIAN_POINT ( 'NONE',  ( -23.72675424202179428, -280.8779958886743771, -344.1149917413332560 ) ) ;
#72891 = CARTESIAN_POINT ( 'NONE',  ( 30.75450656246835734, -293.2095365323900751, -305.9569808653699283 ) ) ;
#72892 = CARTESIAN_POINT ( 'NONE',  ( -47.36141293730224788, -296.3227172363077671, -197.1926891426785460 ) ) ;
#72893 = CARTESIAN_POINT ( 'NONE',  ( 21.96974492092504860, -274.2519511699902637, -315.3440779453779328 ) ) ;
#72894 = CARTESIAN_POINT ( 'NONE',  ( -102.9802714674142408, -298.3143374500106688, -237.1899057006374392 ) ) ;
#72895 = DIRECTION ( 'NONE',  ( 0.000000000000000000, 0.000000000000000000, 1.000000000000000000 ) ) ;
#72896 = CARTESIAN_POINT ( 'NONE',  ( -85.76700008427775401, -293.9519832235627064, -328.9184773446665986 ) ) ;
#72897 = CARTESIAN_POINT ( 'NONE',  ( -8.987206350759501916, -296.0991782222057509, -338.2821074093562288 ) ) ;
#72898 = DIRECTION ( 'NONE',  ( -1.000000000000000000, -0.000000000000000000, -0.000000000000000000 ) ) ;
#72899 = CARTESIAN_POINT ( 'NONE',  ( -80.24121609794639198, -296.4529576600072005, -329.6252155125271770 ) ) ;
#72900 = DIRECTION ( 'NONE',  ( -0.8510748438184358999, -0.5250018354872690862, -0.006684530980050039546 ) ) ;
#72901 = B_SPLINE_CURVE_WITH_KNOTS ( 'NONE', 3,
 ( #89296, #40041, #52861, #47141, #2690, #3619, #24451, #68483, #83134, #23533, #46222, #10236, #81279, #81739, #89771, #31571, #17828, #46680, #67095, #74180, #39561, #61403, #32506, #2229, #75126, #54264, #90235, #31112, #59999, #60461, #25384 ),
 .UNSPECIFIED., .F., .F.,
 ( 4, 2, 2, 2, 1, 2, 2, 2, 2, 2, 2, 2, 2, 2, 2, 4 ),
 ( 0.000000000000000000, 0.005916104402640001356, 0.007395130503299944882, 0.008874156603959888409, 0.01183220880527966271, 0.01479026100659944047, 0.01626928710725932675, 0.01774831320791921477, 0.02366441761055876683, 0.02662246981187848041, 0.02810149591253845516, 0.02958052201319842645, 0.03549662641583841566, 0.03845467861715847618, 0.04141273081847853671, 0.04732883522111848429 ),
 .UNSPECIFIED. ) ;
#72903 = CARTESIAN_POINT ( 'NONE',  ( -108.2990148797109384, -296.3252440394299470, -287.5619941437095690 ) ) ;
#72902 = CARTESIAN_POINT ( 'NONE',  ( -36.55668731188109177, -284.0820710801025371, -194.9972418441998911 ) ) ;
#72904 = CARTESIAN_POINT ( 'NONE',  ( -80.93820472494256535, -285.4784231988035685, -206.8275166316477680 ) ) ;
#72905 = CARTESIAN_POINT ( 'NONE',  ( -8.564236707468705134, -284.5987463175507628, -340.2819924957438502 ) ) ;
#72906 = CARTESIAN_POINT ( 'NONE',  ( 27.42470994676389395, -287.7659505920086076, -312.0653609268888431 ) ) ;
#72907 = CARTESIAN_POINT ( 'NONE',  ( 21.64331529827405021, -290.9185876760646465, -224.2882593392528179 ) ) ;
#72908 = CARTESIAN_POINT ( 'NONE',  ( -35.32998854785326159, -279.2739403521234749, -193.5358233559415453 ) ) ;
#72909 = CARTESIAN_POINT ( 'NONE',  ( -95.99890600148557951, -275.4094976428775681, -317.0979686699210447 ) ) ;
#72910 = CARTESIAN_POINT ( 'NONE',  ( -48.18343439339133027, -264.8229914578195121, -496.4753680102650151 ) ) ;
#72911 = CARTESIAN_POINT ( 'NONE',  ( 33.05514607539908667, -286.0731952119183461, -249.5462283535254358 ) ) ;
#72912 = CARTESIAN_POINT ( 'NONE',  ( -80.37856714471620023, -288.5403802820315491, -333.9022088773372161 ) ) ;
#72913 = CARTESIAN_POINT ( 'NONE',  ( 129.9467878515196162, -299.5541904835127980, -195.3611179825600175 ) ) ;
#72914 = CARTESIAN_POINT ( 'NONE',  ( -101.5916249803873228, -279.4294639178291391, -311.8164708445809765 ) ) ;
#72916 = CARTESIAN_POINT ( 'NONE',  ( 34.08676926968254861, -281.0180828953170362, -255.1337540159136950 ) ) ;
#72915 = CARTESIAN_POINT ( 'NONE',  ( 32.90881567044437617, -291.9252086300456313, -297.6241301183516157 ) ) ;
#72917 = CARTESIAN_POINT ( 'NONE',  ( 4.229085249920590428, -294.6753844772217121, -335.2380124001516037 ) ) ;
#72918 = CARTESIAN_POINT ( 'NONE',  ( 17.32686730478499015, -284.9045123526669272, -218.1256683838033155 ) ) ;
#72919 = EDGE_CURVE ( 'NONE', #75628, #84462, #44374, .T. ) ;
#72920 = CARTESIAN_POINT ( 'NONE',  ( -110.5270659326031790, -280.3417573866738053, -286.7593765964139720 ) ) ;
#72921 = CARTESIAN_POINT ( 'NONE',  ( -108.2002714205350316, -295.3667624903945352, -288.9167126970091317 ) ) ;
#72922 = CIRCLE ( 'NONE', #86480, 7.500000000000013323 ) ;
#72923 = ORIENTED_EDGE ( 'NONE', *, *, #57669, .F. ) ;
#72924 = CARTESIAN_POINT ( 'NONE',  ( 29.33919985515026596, -277.8906705383787994, 25.50000000000000000 ) ) ;
#72926 = CARTESIAN_POINT ( 'NONE',  ( 35.04456948638337366, -283.2962415486646250, -252.0863400165810333 ) ) ;
#72925 = AXIS2_PLACEMENT_3D ( 'NONE', #61855, #90686, #25846 ) ;
#72927 = DIRECTION ( 'NONE',  ( -0.000000000000000000, -0.000000000000000000, -1.000000000000000000 ) ) ;
#72928 = CARTESIAN_POINT ( 'NONE',  ( -106.6662871844225293, -293.6237833571632336, -303.7098442033569086 ) ) ;
#72929 = CARTESIAN_POINT ( 'NONE',  ( 26.01722170459059669, -274.1741510155194419, -226.8658954243709616 ) ) ;
#72930 = CIRCLE ( 'NONE', #85009, 0.5000000000000048850 ) ;
#72931 = CARTESIAN_POINT ( 'NONE',  ( -108.4269854908923065, -290.6053003448192271, -253.6969092170724878 ) ) ;
#72932 = AXIS2_PLACEMENT_3D ( 'NONE', #45498, #18049, #53084 ) ;
#72933 = CARTESIAN_POINT ( 'NONE',  ( -1.647042530098138169, -282.0545322102891532, -205.8894251845867700 ) ) ;
#72934 = CARTESIAN_POINT ( 'NONE',  ( -98.51764879670965058, -274.7208677167836868, -228.9910603197111243 ) ) ;
#72935 = CARTESIAN_POINT ( 'NONE',  ( 26.06759514603298200, -283.7143089214390557, -312.6186816612479333 ) ) ;
#72936 = CARTESIAN_POINT ( 'NONE',  ( 33.33769916781566423, -280.6071985825294632, -290.1488167041902670 ) ) ;
#72937 = CARTESIAN_POINT ( 'NONE',  ( -109.1491514686639874, -280.8312899128474101, -248.7118551419337678 ) ) ;
#72938 = CARTESIAN_POINT ( 'NONE',  ( 19.38870777905117748, -298.7440530408346717, -193.3610971472934636 ) ) ;
#72939 = ORIENTED_EDGE ( 'NONE', *, *, #41688, .F. ) ;
#72940 = CARTESIAN_POINT ( 'NONE',  ( -78.83976814825660995, -273.3426100920561339, -205.5004183633851653 ) ) ;
#72941 = CARTESIAN_POINT ( 'NONE',  ( 28.75412573992997878, -295.0156052494062351, -236.1170528349503002 ) ) ;
#72942 = CARTESIAN_POINT ( 'NONE',  ( 184.7149167944524493, -12.49482340714361506, -6.403442476110241977 ) ) ;
#72943 = CARTESIAN_POINT ( 'NONE',  ( 189.4188515237862589, 293.9636489450775798, 13.99999999999999112 ) ) ;
#72944 = EDGE_CURVE ( 'NONE', #26361, #76874, #28650, .T. ) ;
#72945 = CARTESIAN_POINT ( 'NONE',  ( 33.29126716111535700, -292.0446656426726690, -297.7707770550896385 ) ) ;
#72946 = CARTESIAN_POINT ( 'NONE',  ( -92.06009166544629352, -272.7509353165534094, -221.9474208573190879 ) ) ;
#72947 = CARTESIAN_POINT ( 'NONE',  ( -33.59296365779650984, -293.6186511641000152, -194.1465870286367874 ) ) ;
#72949 = CARTESIAN_POINT ( 'NONE',  ( -7.359831313354650462, -293.6417368952126594, -199.8550546068382232 ) ) ;
#72948 = CARTESIAN_POINT ( 'NONE',  ( -20.25526795762937127, -282.7662352645560304, -195.3538533559490702 ) ) ;
#72950 = CARTESIAN_POINT ( 'NONE',  ( -75.63264206588554828, -291.5644342603516748, -334.6710555069792576 ) ) ;
#72951 = CARTESIAN_POINT ( 'NONE',  ( 33.83424821312373609, -273.8510802730876890, -293.4698350415559389 ) ) ;
#72952 = CARTESIAN_POINT ( 'NONE',  ( -0.7413004339061621817, -278.4825690187726082, -335.2401704488314635 ) ) ;
#72953 = CARTESIAN_POINT ( 'NONE',  ( -8.698964420001162878, -292.7542922301141743, -339.0838532300561496 ) ) ;
#72954 = CARTESIAN_POINT ( 'NONE',  ( 7.791421277713025617, -282.5211529432661450, -209.4411152510967327 ) ) ;
#72955 = CARTESIAN_POINT ( 'NONE',  ( -97.55219031966049670, -283.6428974568090098, -311.7624974560998794 ) ) ;
#72956 = CARTESIAN_POINT ( 'NONE',  ( 3.645104413674261412, -281.6690924702567145, -205.4788437199935629 ) ) ;
#72957 = CARTESIAN_POINT ( 'NONE',  ( -16.26589251418299753, -281.5806564344613889, -344.0626971093176962 ) ) ;
#72958 = CARTESIAN_POINT ( 'NONE',  ( -51.25816404865174292, -278.1671542396359200, -345.8538477270203089 ) ) ;
#72959 = EDGE_CURVE ( 'NONE', #26750, #14772, #28193, .T. ) ;
#72960 = EDGE_CURVE ( 'NONE', #61290, #21738, #530, .T. ) ;
#72961 = CARTESIAN_POINT ( 'NONE',  ( 36.95535874902696349, -276.8520650188337413, -252.9073650446686656 ) ) ;
#72962 = CARTESIAN_POINT ( 'NONE',  ( 7.399455738971494334, -289.1948066931273615, -214.2051214447836571 ) ) ;
#72963 = ORIENTED_EDGE ( 'NONE', *, *, #41624, .F. ) ;
#72964 = CARTESIAN_POINT ( 'NONE',  ( -61.17494723188499250, -299.7430216201950657, -199.1937522017736626 ) ) ;
#72965 = CARTESIAN_POINT ( 'NONE',  ( -36.47174376346121250, -275.0613415323690560, -345.0136011372182452 ) ) ;
#72966 = CARTESIAN_POINT ( 'NONE',  ( -44.81992495491951445, -293.7190018679248737, -194.6911018076216351 ) ) ;
#72967 = CARTESIAN_POINT ( 'NONE',  ( 32.72916948474068022, -292.6233481988778635, -249.3547692446408632 ) ) ;
#72968 = CARTESIAN_POINT ( 'NONE',  ( 38.04673431516613391, -287.2521329936142251, -285.7270170991233158 ) ) ;
#72969 = CARTESIAN_POINT ( 'NONE',  ( 197.2116943569230330, 275.5000000000000568, -12.92446933126074882 ) ) ;
#72971 = CARTESIAN_POINT ( 'NONE',  ( -45.75063976348201322, -281.5602377114073533, -343.7320429426130772 ) ) ;
#72970 = CARTESIAN_POINT ( 'NONE',  ( 36.51774155373829700, -291.8792854290135210, -250.7302646962422159 ) ) ;
#72972 = CARTESIAN_POINT ( 'NONE',  ( -105.1667797009182976, -292.0115798283595723, -300.6645239998105126 ) ) ;
#72973 = CARTESIAN_POINT ( 'NONE',  ( -109.6636208144652898, -282.8471098087292148, -284.5120028395191412 ) ) ;
#72974 = CARTESIAN_POINT ( 'NONE',  ( 12.26179021644768596, -283.6593451517005064, -324.5896826196237726 ) ) ;
#72975 = CARTESIAN_POINT ( 'NONE',  ( -93.41270723345925830, -290.7755172703175504, -322.8673070979820636 ) ) ;
#72976 = CARTESIAN_POINT ( 'NONE',  ( 35.41300954710498416, -281.9493111653811184, -263.1390325155098253 ) ) ;
#72977 = CARTESIAN_POINT ( 'NONE',  ( 36.32654883532413947, -292.0819357405638925, -249.3133399081882828 ) ) ;
#72978 = CARTESIAN_POINT ( 'NONE',  ( 38.39595957079421851, -288.1915868864134609, -257.3236137424045751 ) ) ;
#72979 = CARTESIAN_POINT ( 'NONE',  ( 38.91344462144095928, -287.9164386581488202, -260.1298031878205279 ) ) ;
#72980 = CARTESIAN_POINT ( 'NONE',  ( -71.18010625531486824, -285.7589915692370823, -205.6775630764324205 ) ) ;
#72981 = ORIENTED_EDGE ( 'NONE', *, *, #29881, .T. ) ;
#72982 = CARTESIAN_POINT ( 'NONE',  ( 194.7771416239231996, 25.43510842100042169, 13.92549921621965936 ) ) ;
#72983 = CARTESIAN_POINT ( 'NONE',  ( 37.59834304831932883, -295.5542698966260104, -281.5099030915685034 ) ) ;
#72984 = CARTESIAN_POINT ( 'NONE',  ( -39.11331488911429943, -293.7587814665974406, -346.8474543798751029 ) ) ;
#72985 = ADVANCED_FACE ( 'NONE', ( #85470 ), #93037, .F. ) ;
#72986 = CARTESIAN_POINT ( 'NONE',  ( -99.66167402074758286, -278.1407705060379953, -231.7984487048651090 ) ) ;
#72987 = CARTESIAN_POINT ( 'NONE',  ( -26.21970324939029595, -297.5365650024917841, -193.4642417802111822 ) ) ;
#72988 = CARTESIAN_POINT ( 'NONE',  ( 34.63110557976099102, -291.8243916359490413, -254.4716231057545031 ) ) ;
#72989 = CARTESIAN_POINT ( 'NONE',  ( -4.883618958754046169, -276.2456833634645932, -203.8305878720648252 ) ) ;
#72990 = CARTESIAN_POINT ( 'NONE',  ( -96.90263219420342011, -295.3996471118767886, -226.4026223922836323 ) ) ;
#72991 = AXIS2_PLACEMENT_3D ( 'NONE', #48882, #75896, #83931 ) ;
#72992 = CARTESIAN_POINT ( 'NONE',  ( 35.23294904900917146, -294.9053319230876014, -281.6489240585741527 ) ) ;
#72993 = CARTESIAN_POINT ( 'NONE',  ( 22.83384010455815982, -294.0504229666166225, -228.4686050845659224 ) ) ;
#72994 = CARTESIAN_POINT ( 'NONE',  ( -43.23652644599203398, -278.5081728373386341, -430.8702270131919363 ) ) ;
#72995 = VECTOR ( 'NONE', #15811, 1000.000000000000000 ) ;
#72996 = CARTESIAN_POINT ( 'NONE',  ( -100.1116814962002763, -293.9939406137900164, -311.8069342023820241 ) ) ;
#72997 = CARTESIAN_POINT ( 'NONE',  ( -46.44614785560266768, -275.9367614351162956, -195.9157710565602031 ) ) ;
#72998 = CARTESIAN_POINT ( 'NONE',  ( -84.82851503168700447, -290.6668188310470100, -326.1811687410632885 ) ) ;
#72999 = CARTESIAN_POINT ( 'NONE',  ( -35.64586920953354365, -295.3636096911404252, -343.3750672587078157 ) ) ;
#73000 = AXIS2_PLACEMENT_3D ( 'NONE', #54962, #12842, #49271 ) ;
#73001 = CARTESIAN_POINT ( 'NONE',  ( -110.1485337288108894, -280.7812182887895460, -250.8800308435527597 ) ) ;
#73002 = CARTESIAN_POINT ( 'NONE',  ( -90.70213895787689751, -277.9998595718899992, -215.4606255731293629 ) ) ;
#73003 = ORIENTED_EDGE ( 'NONE', *, *, #78211, .T. ) ;
#73004 = CARTESIAN_POINT ( 'NONE',  ( 25.97822374580684013, -275.4786133166169861, -314.0869707326524463 ) ) ;
#73005 = CARTESIAN_POINT ( 'NONE',  ( -91.81150306074128764, -281.9165261843410804, -321.0992177375026699 ) ) ;
#73006 = CARTESIAN_POINT ( 'NONE',  ( -112.9208981838525574, -277.0797625313704771, -260.2535643847490974 ) ) ;
#73007 = CARTESIAN_POINT ( 'NONE',  ( -69.16251303111366155, -277.6344828261087514, -202.2481427452304104 ) ) ;
#73008 = CARTESIAN_POINT ( 'NONE',  ( -86.41723836161217775, -296.0382991430520860, -215.6543083155183922 ) ) ;
#73009 = CARTESIAN_POINT ( 'NONE',  ( 16.79684297403802518, -278.2820851640076398, -322.3382056213806663 ) ) ;
#73010 = CARTESIAN_POINT ( 'NONE',  ( 154.9842916688210153, 275.0000000000000568, 12.88888888888891593 ) ) ;
#73011 = CARTESIAN_POINT ( 'NONE',  ( -97.86808708340419116, -289.1823146644446183, -225.4511688677434620 ) ) ;
#73012 = CARTESIAN_POINT ( 'NONE',  ( -114.3901258662136797, -290.5413011400655137, -271.2287573755081667 ) ) ;
#73013 = CARTESIAN_POINT ( 'NONE',  ( -52.20854811850352206, -275.8625448284764730, -196.6261857251957963 ) ) ;
#73014 = CARTESIAN_POINT ( 'NONE',  ( -112.3417001281295313, -270.5523135751785162, -270.3357089863371812 ) ) ;
#73015 = CARTESIAN_POINT ( 'NONE',  ( -110.5348553077014344, -283.4541966234602910, -293.7908656783237120 ) ) ;
#73016 = DIRECTION ( 'NONE',  ( 1.000000000000000000, 0.000000000000000000, -0.000000000000000000 ) ) ;
#73017 = CARTESIAN_POINT ( 'NONE',  ( -77.91273765620854874, -283.5073216542049863, -207.2213837150852100 ) ) ;
#73018 = AXIS2_PLACEMENT_3D ( 'NONE', #81976, #38885, #89536 ) ;
#73019 = CARTESIAN_POINT ( 'NONE',  ( 199.7107580773175073, 25.46274433093360301, 10.17758690952041256 ) ) ;
#73020 = CARTESIAN_POINT ( 'NONE',  ( -3.439277640331756647, -291.3051705249692418, -205.2630668959616287 ) ) ;
#73021 = CARTESIAN_POINT ( 'NONE',  ( -42.74071489663341339, -284.1229211537595347, -196.3096664007881600 ) ) ;
#73022 = CARTESIAN_POINT ( 'NONE',  ( 195.1858027385590049, 26.47779181510070146, 15.05860297072264231 ) ) ;
#73023 = CARTESIAN_POINT ( 'NONE',  ( 194.5881128153457098, -26.00396092263537540, 21.50000000000000000 ) ) ;
#73024 = CARTESIAN_POINT ( 'NONE',  ( 12.27242766794423723, -290.7420802497326804, -214.0473386744183983 ) ) ;
#73025 = CARTESIAN_POINT ( 'NONE',  ( -107.8752399937672379, -279.8657679334177715, -292.2452165140078364 ) ) ;
#73026 = CARTESIAN_POINT ( 'NONE',  ( -24.58451979740540594, -284.0980321384393505, -345.9481484084293470 ) ) ;
#73028 = CARTESIAN_POINT ( 'NONE',  ( -81.47857639685697961, -285.4323240396813617, -212.2152999623895084 ) ) ;
#73027 = CARTESIAN_POINT ( 'NONE',  ( 18.79075021819331326, -274.3319095723495593, -320.9617173160100947 ) ) ;
#73029 = CARTESIAN_POINT ( 'NONE',  ( -110.7476787434561203, -280.0453493713906710, -265.1710101379803177 ) ) ;
#73030 = CARTESIAN_POINT ( 'NONE',  ( 15.72202112586517941, -277.0794065282693737, -320.7282026081434196 ) ) ;
#73031 = EDGE_CURVE ( 'NONE', #82490, #69835, #35756, .T. ) ;
#73032 = CARTESIAN_POINT ( 'NONE',  ( -109.0223123248972144, -286.8388378420689833, -248.1205266937496958 ) ) ;
#73033 = VERTEX_POINT ( 'NONE', #57082 ) ;
#73034 = CARTESIAN_POINT ( 'NONE',  ( -111.9109958098805038, -270.5893608454304058, -270.3361269473657558 ) ) ;
#73035 = CARTESIAN_POINT ( 'NONE',  ( -100.0097404549985640, -295.7918157752228581, -315.1914770268384700 ) ) ;
#73036 = CARTESIAN_POINT ( 'NONE',  ( 36.14531818545879815, -289.7009962858164727, -283.4571075966876492 ) ) ;
#73037 = CARTESIAN_POINT ( 'NONE',  ( 197.7051530045995094, 41.80213891112347824, 12.00000000000000000 ) ) ;
#73038 = CARTESIAN_POINT ( 'NONE',  ( 13.79469577742117714, -277.1948066931273047, -206.1857440867352693 ) ) ;
#73039 = CARTESIAN_POINT ( 'NONE',  ( -88.71415407399018704, -278.2710857511310678, -213.4193627885387343 ) ) ;
#73040 = CARTESIAN_POINT ( 'NONE',  ( 36.67798197893209533, -292.1814147632391041, -288.5133634305834107 ) ) ;
#73041 = CARTESIAN_POINT ( 'NONE',  ( -5.516593998334935023, -287.9986249842356756, -203.8801421112974026 ) ) ;
#73042 = CARTESIAN_POINT ( 'NONE',  ( -79.65225891650069912, -281.2316758307698024, -209.6339360414947635 ) ) ;
#73043 = CARTESIAN_POINT ( 'NONE',  ( 36.93595832552122005, -289.2040309470683610, -288.3450775158492547 ) ) ;
#73044 = CARTESIAN_POINT ( 'NONE',  ( -59.51578583863269500, -285.3393142978532637, -342.0628349263005248 ) ) ;
#73045 = CARTESIAN_POINT ( 'NONE',  ( -80.22442354794887365, -277.7818054746463758, -334.3789732546630376 ) ) ;
#73046 = CARTESIAN_POINT ( 'NONE',  ( -104.8482221143613913, -270.9780595289846019, -238.0671880161435467 ) ) ;
#73047 = CARTESIAN_POINT ( 'NONE',  ( 36.36221646880999714, -291.4192034941190173, -253.6582961215340788 ) ) ;
#73048 = CARTESIAN_POINT ( 'NONE',  ( -101.8900607146500192, -278.9379215109555616, -228.2823930435663158 ) ) ;
#73050 = CARTESIAN_POINT ( 'NONE',  ( -90.13700449647819823, -275.1563556530194319, -218.1737505820852903 ) ) ;
#73049 = AXIS2_PLACEMENT_3D ( 'NONE', #62901, #48177, #91738 ) ;
#73051 = FACE_OUTER_BOUND ( 'NONE', #19065, .T. ) ;
#73052 = CARTESIAN_POINT ( 'NONE',  ( -4.829096099716510437, -288.9805209788416391, -202.7746430608542312 ) ) ;
#73053 = CARTESIAN_POINT ( 'NONE',  ( 6.666607923622994925, -272.8809367692422825, -208.3510484586181235 ) ) ;
#73055 = VECTOR ( 'NONE', #43998, 1000.000000000000000 ) ;
#73054 = CARTESIAN_POINT ( 'NONE',  ( 208.6208076322478746, 32.98517505407394168, 14.26380412667038655 ) ) ;
#73056 = CARTESIAN_POINT ( 'NONE',  ( -85.52006280609499811, -278.8718443071332445, -215.4354062334244588 ) ) ;
#73057 = CIRCLE ( 'NONE', #15605, 4.025000000000000355 ) ;
#73058 = CARTESIAN_POINT ( 'NONE',  ( 38.98616187440877923, -276.8387606310905653, -276.8469641047298637 ) ) ;
#73059 = CARTESIAN_POINT ( 'NONE',  ( -86.50733033714197973, -298.7783042571975898, -215.6060659608170909 ) ) ;
#73060 = CARTESIAN_POINT ( 'NONE',  ( -81.43623256062613791, -282.6942458828311828, -333.2628231212455603 ) ) ;
#73061 = CARTESIAN_POINT ( 'NONE',  ( 34.06544669660750202, -289.5681981683001140, -290.0192744247504493 ) ) ;
#73062 = CARTESIAN_POINT ( 'NONE',  ( -26.35364258250954705, -299.7074747675757749, -194.0516646480180896 ) ) ;
#73063 = CARTESIAN_POINT ( 'NONE',  ( -101.9895631524544939, -298.2986125637458485, -229.2677788079590186 ) ) ;
#73064 = CARTESIAN_POINT ( 'NONE',  ( -12.37311779704040759, -296.7269406588296761, -340.9607307062144628 ) ) ;
#73065 = CARTESIAN_POINT ( 'NONE',  ( 36.02311296814248465, -279.7426621485017790, -285.1778750019664699 ) ) ;
#73066 = TOROIDAL_SURFACE ( 'NONE', #15612, 1.000000000000000000, 0.5000000000000000000 ) ;
#73067 = CARTESIAN_POINT ( 'NONE',  ( -95.03391018387637246, -271.2286763439871606, -222.9760077353333827 ) ) ;
#73068 = CARTESIAN_POINT ( 'NONE',  ( 17.75877964030828338, -288.4242270669927279, -217.6506670674926909 ) ) ;
#73069 = CARTESIAN_POINT ( 'NONE',  ( -53.48993985878833257, -288.1845432221370515, -341.8695820006565214 ) ) ;
#73070 = CARTESIAN_POINT ( 'NONE',  ( -98.66049953969873343, -248.8406155931078274, -334.2579121867940444 ) ) ;
#73071 = ORIENTED_EDGE ( 'NONE', *, *, #74867, .T. ) ;
#73072 = CARTESIAN_POINT ( 'NONE',  ( -8.472701289815535830, -287.2563324886975238, -341.1226210832681431 ) ) ;
#73073 = CARTESIAN_POINT ( 'NONE',  ( 32.33251146571912216, -287.5104289021707586, -292.3832470775842012 ) ) ;
#73074 = ORIENTED_EDGE ( 'NONE', *, *, #16074, .T. ) ;
#73075 = CARTESIAN_POINT ( 'NONE',  ( -80.77451170167559269, -286.5579207549085936, -207.0903385480012560 ) ) ;
#73076 = CIRCLE ( 'NONE', #85165, 1.000000000000000888 ) ;
#73077 = CARTESIAN_POINT ( 'NONE',  ( 11.76506004665075089, -276.6811842291739367, -324.4724358216403175 ) ) ;
#73078 = CARTESIAN_POINT ( 'NONE',  ( 1.555230137263102996, -291.4792703585474669, -204.2056330633209598 ) ) ;
#73079 = CARTESIAN_POINT ( 'NONE',  ( 35.51518249018909756, -282.5156972125018910, -295.1272094515709341 ) ) ;
#73080 = CARTESIAN_POINT ( 'NONE',  ( 26.15577599719389923, -283.6343154095646355, -312.6787062672458433 ) ) ;
#73081 = CARTESIAN_POINT ( 'NONE',  ( -24.53291955609521580, -283.2263779232612819, -346.3209468134538156 ) ) ;
#73082 = CARTESIAN_POINT ( 'NONE',  ( 33.78001832583415620, -281.6672170382085483, -253.8145578856452289 ) ) ;
#73083 = CARTESIAN_POINT ( 'NONE',  ( -99.62977921489535049, -248.4066214194129714, -334.3629173841853799 ) ) ;
#73084 = CARTESIAN_POINT ( 'NONE',  ( -68.78513416746625353, -279.4665886414322813, -338.2820478901094816 ) ) ;
#73085 = CARTESIAN_POINT ( 'NONE',  ( 120.6115914165433622, 149.8424774028926549, -263.0264761077845037 ) ) ;
#73086 = CARTESIAN_POINT ( 'NONE',  ( 4.580739421786890198, -58.54268714549175456, -351.3897242287694667 ) ) ;
#73087 = VECTOR ( 'NONE', #3137, 1000.000000000000000 ) ;
#73088 = CARTESIAN_POINT ( 'NONE',  ( -107.3480541873074117, -272.0321835944646978, -248.9341396886358382 ) ) ;
#73089 = CARTESIAN_POINT ( 'NONE',  ( 37.03546872130033307, -293.3064656943403747, -290.0477544997108907 ) ) ;
#73090 = CARTESIAN_POINT ( 'NONE',  ( -101.5192183512151018, -254.7299117250532277, -324.2986292072765764 ) ) ;
#73092 = CARTESIAN_POINT ( 'NONE',  ( -98.78793098692258923, -288.3905111404708919, -311.2595676259820721 ) ) ;
#73091 = CARTESIAN_POINT ( 'NONE',  ( -107.6178393504614377, -271.6262271496485710, -239.9854724940879294 ) ) ;
#73093 = CARTESIAN_POINT ( 'NONE',  ( -58.74205432471467958, -297.1923203538758003, -341.4448033007763570 ) ) ;
#73094 = CARTESIAN_POINT ( 'NONE',  ( 21.57882386082837556, -289.4797581162507072, -314.3095773604123337 ) ) ;
#73095 = EDGE_LOOP ( 'NONE', ( #81564, #54280, #9743, #93411 ) ) ;
#73096 = CARTESIAN_POINT ( 'NONE',  ( -76.95051930630967263, -296.5099352471046927, -336.1797910864050891 ) ) ;
#73097 = CARTESIAN_POINT ( 'NONE',  ( 9.064752347471532801, -287.2018323135091578, -213.9303674108047915 ) ) ;
#73098 = CARTESIAN_POINT ( 'NONE',  ( -10.44309843443351049, -273.3152305445330512, -198.4856947690159359 ) ) ;
#73099 = CIRCLE ( 'NONE', #33753, 8.000000000000000000 ) ;
#73100 = CARTESIAN_POINT ( 'NONE',  ( -2.032560889525590664, -295.3994176685293951, -338.6064365563865408 ) ) ;
#73101 = EDGE_CURVE ( 'NONE', #45666, #33195, #59545, .T. ) ;
#73102 = CARTESIAN_POINT ( 'NONE',  ( 36.22629968212283558, -293.7614618421599175, -247.8383227035716914 ) ) ;
#73103 = CARTESIAN_POINT ( 'NONE',  ( -107.0022520373381241, -291.0086096485084113, -248.4922429912959672 ) ) ;
#73104 = ORIENTED_EDGE ( 'NONE', *, *, #38171, .F. ) ;
#73105 = CARTESIAN_POINT ( 'NONE',  ( -57.75651281168471485, -275.7108350334418674, -197.5568130899085304 ) ) ;
#73106 = CARTESIAN_POINT ( 'NONE',  ( 38.92354293375725405, -274.2499612741542023, -262.6357259258361410 ) ) ;
#73107 = EDGE_CURVE ( 'NONE', #30245, #40166, #18706, .T. ) ;
#73108 = ORIENTED_EDGE ( 'NONE', *, *, #63351, .F. ) ;
#73109 = CARTESIAN_POINT ( 'NONE',  ( -114.3161071221565095, -278.0802304824414932, -268.7292890590784964 ) ) ;
#73110 = CARTESIAN_POINT ( 'NONE',  ( 14.06839398099382699, -273.1885869972965111, -217.4135718842441918 ) ) ;
#73111 = CARTESIAN_POINT ( 'NONE',  ( -92.25880484591469610, -274.3226999491774905, -221.7983989117779231 ) ) ;
#73112 = CARTESIAN_POINT ( 'NONE',  ( -85.47380000771069319, -274.3088133280386387, -215.0965126812099868 ) ) ;
#73113 = CARTESIAN_POINT ( 'NONE',  ( -93.41286672215939291, -275.0192372706783317, -219.0583908918939358 ) ) ;
#73114 = CARTESIAN_POINT ( 'NONE',  ( 9.483832685155217490, -274.4325049931520653, -329.4681939319050343 ) ) ;
#73115 = CARTESIAN_POINT ( 'NONE',  ( -93.15485587731009787, -296.5333459091953614, -317.5905093728383690 ) ) ;
#73116 = CARTESIAN_POINT ( 'NONE',  ( 21.78919188548751507, -292.7361839201291218, -314.1665118064395301 ) ) ;
#73117 = CYLINDRICAL_SURFACE ( 'NONE', #13997, 4.025000000000000355 ) ;
#73118 = CARTESIAN_POINT ( 'NONE',  ( -34.28725712780541102, -277.5070560793624850, -347.2389254522084343 ) ) ;
#73119 = CARTESIAN_POINT ( 'NONE',  ( 35.69887234250364827, -275.7349499831626076, -271.5828482630395797 ) ) ;
#73120 = CARTESIAN_POINT ( 'NONE',  ( -93.54599913363162500, -283.9489943653851469, -218.3761255032945598 ) ) ;
#73121 = CARTESIAN_POINT ( 'NONE',  ( -95.96129336208792893, -297.9062562753256884, -317.4322159043396141 ) ) ;
#73122 = DIRECTION ( 'NONE',  ( 1.000000000000000000, 0.000000000000000000, 0.000000000000000000 ) ) ;
#73123 = AXIS2_PLACEMENT_3D ( 'NONE', #65232, #22118, #79872 ) ;
#73124 = CARTESIAN_POINT ( 'NONE',  ( -39.96950239376612046, -285.2154572861724660, -197.2468486323607522 ) ) ;
#73125 = CARTESIAN_POINT ( 'NONE',  ( -101.4719067437793001, -276.2911120056779737, -307.4139430091987037 ) ) ;
#73126 = CARTESIAN_POINT ( 'NONE',  ( -103.6699102018617538, -276.6977129306728784, -302.3529546323155728 ) ) ;
#73127 = CARTESIAN_POINT ( 'NONE',  ( -72.40716872195855558, -285.5163125606239873, -336.6733609061362813 ) ) ;
#73128 = CARTESIAN_POINT ( 'NONE',  ( 28.39292233211522998, -277.1989220997525649, -303.1267739309547551 ) ) ;
#73129 = DIRECTION ( 'NONE',  ( -1.000000000000000000, -0.000000000000000000, -0.000000000000000000 ) ) ;
#73130 = CARTESIAN_POINT ( 'NONE',  ( 7.751075117740841236, -274.8481405682493914, -331.8518526148474166 ) ) ;
#73131 = TOROIDAL_SURFACE ( 'NONE', #54997, 12.40608546931776957, 1.000000000000000000 ) ;
#73132 = CARTESIAN_POINT ( 'NONE',  ( -96.27574277624613330, -281.1918237722447316, -223.7048531446321249 ) ) ;
#73133 = DIRECTION ( 'NONE',  ( -0.000000000000000000, -0.000000000000000000, 1.000000000000000000 ) ) ;
#73134 = CARTESIAN_POINT ( 'NONE',  ( -0.4412112234383363529, -288.4587809395545719, -204.4095045454016031 ) ) ;
#73135 = AXIS2_PLACEMENT_3D ( 'NONE', #59984, #23972, #15479 ) ;
#73136 = CARTESIAN_POINT ( 'NONE',  ( 155.3967522965721173, 18.12362412296635128, -8.741384835540280562 ) ) ;
#73137 = CARTESIAN_POINT ( 'NONE',  ( 6.758878966034807867, -290.6513980749826374, -209.6336831662218856 ) ) ;
#73138 = CARTESIAN_POINT ( 'NONE',  ( -47.80257052418233599, -229.5268262511776527, 22.50000000000000000 ) ) ;
#73139 = CARTESIAN_POINT ( 'NONE',  ( 9.260745600255551935, -297.4432165736817524, -196.9738530863085089 ) ) ;
#73140 = CARTESIAN_POINT ( 'NONE',  ( -44.39435959057286141, -290.1017168606732071, -196.4100128921299984 ) ) ;
#73141 = CARTESIAN_POINT ( 'NONE',  ( -101.7183354143585632, -264.3591293023451385, -316.7762957234928649 ) ) ;
#73142 = CARTESIAN_POINT ( 'NONE',  ( 180.2294467949672878, 214.9970011440365454, -24.94063848305471609 ) ) ;
#73143 = CARTESIAN_POINT ( 'NONE',  ( -57.12993618525803896, -287.7826750952785346, -344.1119553580791148 ) ) ;
#73144 = CARTESIAN_POINT ( 'NONE',  ( 20.82394529270771599, -283.7855490092647415, -315.7835585854966780 ) ) ;
#73145 = CARTESIAN_POINT ( 'NONE',  ( -43.56068242780591504, -284.2146047317261264, -194.5768080435144327 ) ) ;
#73146 = CIRCLE ( 'NONE', #61056, 2.842139515347646750 ) ;
#73147 = CIRCLE ( 'NONE', #20366, 2.999999999999997780 ) ;
#73148 = CARTESIAN_POINT ( 'NONE',  ( -0.9449166246075736408, -283.9840292369245844, -334.3193001659674337 ) ) ;
#73149 = CARTESIAN_POINT ( 'NONE',  ( -107.5127507160505900, -285.6304174285627937, -249.4820569209224743 ) ) ;
#73150 = CARTESIAN_POINT ( 'NONE',  ( -95.11347048095392154, -291.8664548480630287, -318.7632418221128887 ) ) ;
#73151 = CARTESIAN_POINT ( 'NONE',  ( -68.83929638076644153, -273.9825625775587241, -200.1068109098702053 ) ) ;
#73152 = AXIS2_PLACEMENT_3D ( 'NONE', #42004, #70918, #20722 ) ;
#73153 = CARTESIAN_POINT ( 'NONE',  ( 15.65814368809771295, -286.3895567345195445, -324.2885693897821398 ) ) ;
#73154 = CARTESIAN_POINT ( 'NONE',  ( 23.51804566061516510, -276.1822351590183189, -317.5533758655669203 ) ) ;
#73155 = CARTESIAN_POINT ( 'NONE',  ( 36.53202046756055665, -295.3939881498735076, -259.6597064731944897 ) ) ;
#73156 = CARTESIAN_POINT ( 'NONE',  ( -48.18343439339132317, -281.1256702228442350, -435.6442049081567234 ) ) ;
#73157 = CARTESIAN_POINT ( 'NONE',  ( -37.30987171927208124, -291.5519495502701943, -345.3611179825600175 ) ) ;
#73158 = CARTESIAN_POINT ( 'NONE',  ( -65.52016485367887810, -282.1132798393017538, -338.2512978017085175 ) ) ;
#73159 = ADVANCED_FACE ( 'NONE', ( #5480 ), #64669, .F. ) ;
#73160 = CARTESIAN_POINT ( 'NONE',  ( -110.9176308258383159, -276.7498517870059231, -254.9169901867596195 ) ) ;
#73161 = VERTEX_POINT ( 'NONE', #21072 ) ;
#73162 = EDGE_CURVE ( 'NONE', #52528, #80622, #93497, .T. ) ;
#73163 = CARTESIAN_POINT ( 'NONE',  ( -106.2090945444642358, -271.4571733933473752, -237.4979206764600406 ) ) ;
#73164 = CARTESIAN_POINT ( 'NONE',  ( 34.72754688294035930, -274.7384623431737509, -258.0426876069348054 ) ) ;
#73165 = CARTESIAN_POINT ( 'NONE',  ( -2.124973169838737963, -294.0473952654028267, -205.6127962383809518 ) ) ;
#73166 = AXIS2_PLACEMENT_3D ( 'NONE', #10724, #4565, #32529 ) ;
#73167 = CARTESIAN_POINT ( 'NONE',  ( 27.68999468555567844, -294.0368607340075755, -236.6819387010903881 ) ) ;
#73168 = CARTESIAN_POINT ( 'NONE',  ( -108.3579801980407211, -286.0397047751482660, -291.2548693938053361 ) ) ;
#73169 = CARTESIAN_POINT ( 'NONE',  ( -25.13360142715051992, -293.6301744186044971, -194.9318887829286950 ) ) ;
#73170 = CARTESIAN_POINT ( 'NONE',  ( 34.98090694058139860, -294.5489106884811008, -245.2461233633605673 ) ) ;
#73171 = CARTESIAN_POINT ( 'NONE',  ( -82.36147831468070990, -295.5194750967788195, -327.8905101744839499 ) ) ;
#73172 = CARTESIAN_POINT ( 'NONE',  ( -31.69606010021917797, -290.9811823337887517, -345.2003426393226846 ) ) ;
#73173 = CARTESIAN_POINT ( 'NONE',  ( -79.15794535491855299, -283.7664013229027091, -335.0171435302522696 ) ) ;
#73174 = CARTESIAN_POINT ( 'NONE',  ( 29.23053802437308946, -296.9591603901928352, -194.8226834078566299 ) ) ;
#73175 = CARTESIAN_POINT ( 'NONE',  ( -52.17120467166177633, -285.7007987483117404, -194.7482356052953776 ) ) ;
#73176 = CARTESIAN_POINT ( 'NONE',  ( -111.8072690319441733, -280.4562987191866910, -276.2328196184652143 ) ) ;
#73177 = CARTESIAN_POINT ( 'NONE',  ( -77.25217553056639019, -284.2992028870982608, -208.7030595633969199 ) ) ;
#73178 = CARTESIAN_POINT ( 'NONE',  ( 36.58979311425390080, -285.3890465491662098, -257.6705470108576037 ) ) ;
#73179 = CARTESIAN_POINT ( 'NONE',  ( -108.4387400044720522, -277.0297852208477707, -244.0274134981911516 ) ) ;
#73180 = CARTESIAN_POINT ( 'NONE',  ( 196.7445862410842778, 294.2657832282549748, -82.73034305482168804 ) ) ;
#73181 = CARTESIAN_POINT ( 'NONE',  ( -109.5601635404877499, -283.9096509625210842, -281.7530366059522180 ) ) ;
#73182 = CARTESIAN_POINT ( 'NONE',  ( 37.86193009706390455, -282.5740009459709086, -255.7863891489984951 ) ) ;
#73183 = CARTESIAN_POINT ( 'NONE',  ( -97.11444395950869080, -288.9630396228041036, -318.5486378931654485 ) ) ;
#73184 = CARTESIAN_POINT ( 'NONE',  ( 14.35554667347608415, -277.9402894807163875, -326.4136181273895545 ) ) ;
#73185 = CARTESIAN_POINT ( 'NONE',  ( -31.47128582580520373, -278.2947990966504790, -346.6947026069813091 ) ) ;
#73186 = CARTESIAN_POINT ( 'NONE',  ( -37.00619625555646053, -279.8897888413432042, -197.3618889339537361 ) ) ;
#73187 = CARTESIAN_POINT ( 'NONE',  ( -84.24320124703196200, -275.3832176796396993, -212.2913668866021055 ) ) ;
#73188 = CARTESIAN_POINT ( 'NONE',  ( 38.60628375436721171, -293.7117920417641699, -283.1257928102254482 ) ) ;
#73189 = CARTESIAN_POINT ( 'NONE',  ( -53.79507220571837678, -287.2844673148395032, -343.1700003172549600 ) ) ;
#73190 = CARTESIAN_POINT ( 'NONE',  ( -83.79495375490245124, -293.0269081422002273, -209.8914931144436764 ) ) ;
#73191 = CARTESIAN_POINT ( 'NONE',  ( 34.36707742795692155, -292.6733840335568857, -285.6553619667395196 ) ) ;
#73192 = CARTESIAN_POINT ( 'NONE',  ( 32.36572248969818588, -293.5069782880681259, -292.1088240402822862 ) ) ;
#73193 = CARTESIAN_POINT ( 'NONE',  ( -113.7004471572712703, -291.7282508814546986, -262.6816388558936524 ) ) ;
#73194 = CARTESIAN_POINT ( 'NONE',  ( 29.06180668779334653, -281.7902840199041066, -239.6707851293002136 ) ) ;
#73195 = CARTESIAN_POINT ( 'NONE',  ( -43.25215934052818767, -296.8996391772359402, -193.8453268357231991 ) ) ;
#73196 = CARTESIAN_POINT ( 'NONE',  ( -71.85327816632135978, -290.1477650267762556, -339.0798473680692950 ) ) ;
#73197 = CARTESIAN_POINT ( 'NONE',  ( -92.54800716189920706, -281.9718319951990111, -322.2701159640413948 ) ) ;
#73198 = CARTESIAN_POINT ( 'NONE',  ( 32.84733707369120737, -288.2893156450637093, -301.9719286036957442 ) ) ;
#73199 = CARTESIAN_POINT ( 'NONE',  ( -72.38788856700459462, -285.9080880295402380, -206.2855813242020986 ) ) ;
#73200 = CARTESIAN_POINT ( 'NONE',  ( 161.2244399300530233, 8.542400036368780647, 10.00000000000000000 ) ) ;
#73201 = AXIS2_PLACEMENT_3D ( 'NONE', #11140, #4981, #75542 ) ;
#73202 = CARTESIAN_POINT ( 'NONE',  ( 197.6688820137005678, 288.5744782996524123, -96.90442113908628130 ) ) ;
#73203 = CARTESIAN_POINT ( 'NONE',  ( -21.90833566152406675, -108.8621393979285443, -358.8400048060100858 ) ) ;
#73204 = CARTESIAN_POINT ( 'NONE',  ( -107.7709874604358902, -278.0111077307921050, -250.5077099796372408 ) ) ;
#73205 = CARTESIAN_POINT ( 'NONE',  ( -109.5930718114085352, -277.3085056103241754, -282.8436747111708769 ) ) ;
#73206 = CARTESIAN_POINT ( 'NONE',  ( 13.95354979347750835, -274.4151795074977827, -212.8917841408612048 ) ) ;
#73207 = CARTESIAN_POINT ( 'NONE',  ( 66.34501194978001593, 45.89495233920238348, -316.1728383282853656 ) ) ;
#73208 = CARTESIAN_POINT ( 'NONE',  ( -113.7879192522227925, -277.1474555070945485, -268.7285821512305688 ) ) ;
#73210 = CARTESIAN_POINT ( 'NONE',  ( -1.664197571552678223, -280.5970545489188339, -335.9422017180141893 ) ) ;
#73209 = CIRCLE ( 'NONE', #27867, 25.00000000000000355 ) ;
#73211 = CARTESIAN_POINT ( 'NONE',  ( -19.50312986280587069, -296.5860549155258923, -344.2783976665886030 ) ) ;
#73212 = EDGE_LOOP ( 'NONE', ( #68515, #23371, #86569, #26362 ) ) ;
#73213 = PRODUCT ( 'cast Iron C-Frame Chassis', 'cast Iron C-Frame Chassis', '', ( #11814 ) ) ;
#73214 = CARTESIAN_POINT ( 'NONE',  ( -49.70530253418396427, -292.3826893828946822, -198.3019032850177155 ) ) ;
#73215 = CARTESIAN_POINT ( 'NONE',  ( -63.48825068814020511, -274.6608112161942472, -198.1864818107218298 ) ) ;
#73216 = CARTESIAN_POINT ( 'NONE',  ( -80.71194023548018492, -288.3388930672060724, -329.7562829896559151 ) ) ;
#73217 = CARTESIAN_POINT ( 'NONE',  ( -114.2397671894842119, -273.2034605398562803, -270.3693937356876518 ) ) ;
#73218 = CARTESIAN_POINT ( 'NONE',  ( -108.8842984839512837, -296.5265477094952757, -284.9373756802219191 ) ) ;
#73219 = ORIENTED_EDGE ( 'NONE', *, *, #87889, .T. ) ;
#73220 = LINE ( 'NONE', #72284, #76470 ) ;
#73221 = VECTOR ( 'NONE', #37824, 1000.000000000000000 ) ;
#73222 = VECTOR ( 'NONE', #66558, 1000.000000000000000 ) ;
#73223 = CARTESIAN_POINT ( 'NONE',  ( -79.13504755576629179, -281.4137194915968507, -207.3489146086906203 ) ) ;
#73224 = EDGE_CURVE ( 'NONE', #1470, #41734, #28669, .T. ) ;
#73225 = AXIS2_PLACEMENT_3D ( 'NONE', #17566, #10435, #3822 ) ;
#73226 = CARTESIAN_POINT ( 'NONE',  ( -3.016480513786325535, -281.5965610198867921, -205.5703009478988008 ) ) ;
#73227 = CARTESIAN_POINT ( 'NONE',  ( -103.9166967655488349, -280.7930338330506288, -233.7312963297764270 ) ) ;
#73228 = CARTESIAN_POINT ( 'NONE',  ( -62.24596879253420667, -272.2021386847839608, -201.0034568747851438 ) ) ;
#73229 = DIRECTION ( 'NONE',  ( 0.2456588035076310295, -0.9693563597868428694, 0.000000000000000000 ) ) ;
#73230 = DIRECTION ( 'NONE',  ( -1.000000000000000000, 0.000000000000000000, 0.000000000000000000 ) ) ;
#73231 = CARTESIAN_POINT ( 'NONE',  ( -59.73565045294212439, -279.9206511083185092, -200.8275204372000928 ) ) ;
#73232 = CARTESIAN_POINT ( 'NONE',  ( 12.60741885962485576, -277.1789520242494973, -328.7498526183424588 ) ) ;
#73233 = AXIS2_PLACEMENT_3D ( 'NONE', #53351, #75601, #12137 ) ;
#73234 = CARTESIAN_POINT ( 'NONE',  ( -3.601420209294212249, -278.6070885727895075, -337.3574602997516081 ) ) ;
#73235 = CARTESIAN_POINT ( 'NONE',  ( -67.49293634223286631, -276.0147363679222394, -340.5715819368065240 ) ) ;
#73236 = ORIENTED_EDGE ( 'NONE', *, *, #18737, .F. ) ;
#73237 = CARTESIAN_POINT ( 'NONE',  ( 196.2220355002111489, 24.40165861654593016, 11.64020769021003332 ) ) ;
#73238 = CARTESIAN_POINT ( 'NONE',  ( 37.88885930567494142, -283.5980066611590473, -275.5225696371106210 ) ) ;
#73239 = CARTESIAN_POINT ( 'NONE',  ( -28.07578558877671426, -291.3697968209031046, -197.7379168887302967 ) ) ;
#73240 = CARTESIAN_POINT ( 'NONE',  ( -4.809520512284307436, -285.8180479359820652, -200.6835026635681629 ) ) ;
#73241 = CARTESIAN_POINT ( 'NONE',  ( -111.1075222570720058, -282.7133142886193014, -276.4090513059687169 ) ) ;
#73243 = CARTESIAN_POINT ( 'NONE',  ( -10.20263917335970305, -284.4889851876559419, -201.0307626556661091 ) ) ;
#73242 = CARTESIAN_POINT ( 'NONE',  ( -18.60297489575357233, -281.3808948384404971, -341.5773804018525652 ) ) ;
#73244 = CARTESIAN_POINT ( 'NONE',  ( -64.97978957592825111, -280.8879312464148938, -202.3665114541418006 ) ) ;
#73245 = CARTESIAN_POINT ( 'NONE',  ( 219.7099725226080977, -147.7221692137691775, -1.978481845683818907 ) ) ;
#73246 = CARTESIAN_POINT ( 'NONE',  ( -96.94180419081259004, -283.5944028192403152, -222.8819855696234242 ) ) ;
#73247 = CARTESIAN_POINT ( 'NONE',  ( -27.97177029087859168, -296.9334926536926105, -344.8254258010556441 ) ) ;
#73248 = CARTESIAN_POINT ( 'NONE',  ( -97.83645399810694698, -278.9209622056022795, -311.6381479445759055 ) ) ;
#73249 = CARTESIAN_POINT ( 'NONE',  ( -112.5204223572541053, -286.5208734570495039, -272.8154048871286932 ) ) ;
#73250 = EDGE_CURVE ( 'NONE', #14834, #83547, #49943, .T. ) ;
#73251 = CARTESIAN_POINT ( 'NONE',  ( 115.2448031289451222, -299.5541904835127980, -198.2496582146980302 ) ) ;
#73252 = CARTESIAN_POINT ( 'NONE',  ( -69.04176417201057347, -293.5587077001491139, -201.7582674619375780 ) ) ;
#73253 = CARTESIAN_POINT ( 'NONE',  ( 1.896654034993785931, -274.5274096662241163, -334.3388897330638656 ) ) ;
#73254 = CARTESIAN_POINT ( 'NONE',  ( 27.30339984700533407, -287.2964748890674400, -311.9943683261041087 ) ) ;
#73255 = CARTESIAN_POINT ( 'NONE',  ( -6.922078925331913268, -290.8580551372217542, -203.1220886693526211 ) ) ;
#73256 = CARTESIAN_POINT ( 'NONE',  ( -105.7327961481518059, -276.8795873496372906, -297.2665349502402705 ) ) ;
#73257 = CARTESIAN_POINT ( 'NONE',  ( -78.65652458365705968, -293.7542639725073172, -332.0993964455642526 ) ) ;
#73258 = CARTESIAN_POINT ( 'NONE',  ( -74.95399505978609511, -290.8795582832368609, -333.5151035318205004 ) ) ;
#73259 = DIRECTION ( 'NONE',  ( -0.8435586647355767242, 0.000000000000000000, -0.5370370370370473045 ) ) ;
#73260 = DIRECTION ( 'NONE',  ( 0.000000000000000000, 0.000000000000000000, -1.000000000000000000 ) ) ;
#73261 = CARTESIAN_POINT ( 'NONE',  ( -95.06977275496491586, -294.3518305742202870, -320.2627951568942990 ) ) ;
#73262 = CARTESIAN_POINT ( 'NONE',  ( 16.54482709176679478, -288.4344903114027829, -219.9174554845207012 ) ) ;
#73263 = CARTESIAN_POINT ( 'NONE',  ( -95.62838437909911704, -288.1270263401531793, -319.1320661971221284 ) ) ;
#73264 = CARTESIAN_POINT ( 'NONE',  ( 16.45401370096022831, -289.6944855736180102, -320.6492043221166455 ) ) ;
#73265 = CARTESIAN_POINT ( 'NONE',  ( 170.7304434856092143, 250.0000000000000568, -24.91818181818181088 ) ) ;
#73266 = CARTESIAN_POINT ( 'NONE',  ( -110.2827589834297015, -291.2721597052092193, -276.6539497295956380 ) ) ;
#73267 = CARTESIAN_POINT ( 'NONE',  ( 153.9133111279453203, 20.47222690886559704, 13.06183683676577267 ) ) ;
#73268 = CARTESIAN_POINT ( 'NONE',  ( -57.17322733088074926, -290.5074341996305520, -344.4072813486337736 ) ) ;
#73269 = CARTESIAN_POINT ( 'NONE',  ( -53.38516879397450055, -277.8676110552775071, -196.6801831234620010 ) ) ;
#73270 = CARTESIAN_POINT ( 'NONE',  ( -14.23815008033865759, -280.6769305874645397, -196.8751976733161939 ) ) ;
#73271 = CARTESIAN_POINT ( 'NONE',  ( -14.23006120043628719, -280.0104755763516664, -196.8777411304390625 ) ) ;
#73272 = CARTESIAN_POINT ( 'NONE',  ( 35.00453609008011568, -285.8085040041834759, -290.3278874668597496 ) ) ;
#73273 = DIRECTION ( 'NONE',  ( 0.000000000000000000, 0.000000000000000000, 1.000000000000000000 ) ) ;
#73274 = CARTESIAN_POINT ( 'NONE',  ( -66.53397474552238577, -277.8053176888203097, -202.0927518105919489 ) ) ;
#73275 = EDGE_CURVE ( 'NONE', #65497, #72058, #16557, .T. ) ;
#73276 = CARTESIAN_POINT ( 'NONE',  ( -109.5723787496062016, -282.2922277454530899, -290.5534362380706739 ) ) ;
#73277 = CARTESIAN_POINT ( 'NONE',  ( -110.6395504398199847, -271.5021483123970825, -270.3477634379551660 ) ) ;
#73278 = CARTESIAN_POINT ( 'NONE',  ( -113.0805574562855895, -276.9094828927819663, -280.0718888115501954 ) ) ;
#73279 = CARTESIAN_POINT ( 'NONE',  ( -91.67426346666579207, -284.2199701833703784, -216.2365850013540864 ) ) ;
#73280 = CARTESIAN_POINT ( 'NONE',  ( -90.32057426773499742, -274.0811625408844066, -219.8864625244989384 ) ) ;
#73281 = CARTESIAN_POINT ( 'NONE',  ( -63.37354268129882939, -275.1447534770784387, -198.5213694749504327 ) ) ;
#73282 = CARTESIAN_POINT ( 'NONE',  ( 32.11698423171890227, -275.5176906991226247, -292.8906242749386593 ) ) ;
#73283 = CARTESIAN_POINT ( 'NONE',  ( -76.68613590182987139, -297.5784857714271538, -334.2731698376891245 ) ) ;
#73284 = CARTESIAN_POINT ( 'NONE',  ( 3.181940437418188772, -288.6907664074376498, -335.8975896573491582 ) ) ;
#73285 = CARTESIAN_POINT ( 'NONE',  ( 22.25183336013190427, -280.2646852086944591, -316.8354894476419190 ) ) ;
#73286 = CIRCLE ( 'NONE', #11220, 26.04691768583011680 ) ;
#73287 = CARTESIAN_POINT ( 'NONE',  ( -40.63029578579246959, -291.8452168153966113, -193.4181941621540091 ) ) ;
#73288 = CARTESIAN_POINT ( 'NONE',  ( -107.9558864063967576, -289.3529395009105087, -289.9657638697507309 ) ) ;
#73289 = CARTESIAN_POINT ( 'NONE',  ( 27.75276186004279211, -291.0551154088623207, -233.1091158226316509 ) ) ;
#73290 = EDGE_LOOP ( 'NONE', ( #5200, #50243, #6624, #30403 ) ) ;
#73291 = CARTESIAN_POINT ( 'NONE',  ( 198.1232845152093205, 70.21759135774367167, 10.41992497367912662 ) ) ;
#73292 = CARTESIAN_POINT ( 'NONE',  ( -109.8513564468808141, -289.9416630509429069, -279.3242749132838867 ) ) ;
#73293 = CARTESIAN_POINT ( 'NONE',  ( 204.5044540939250055, -147.7221692137691775, 10.75739200365177695 ) ) ;
#73294 = CARTESIAN_POINT ( 'NONE',  ( 21.90092091071948133, -287.8354745835331983, -221.5437843153170832 ) ) ;
#73295 = CARTESIAN_POINT ( 'NONE',  ( -6.998514795304313196, -288.9805209788416391, -207.2794874003663779 ) ) ;
#73296 = CARTESIAN_POINT ( 'NONE',  ( 25.51507949784165064, -293.1956637955955216, -314.4504294448437349 ) ) ;
#73297 = CARTESIAN_POINT ( 'NONE',  ( -38.70684677102161686, -284.3841067151028597, -346.8557887065531986 ) ) ;
#73298 = CARTESIAN_POINT ( 'NONE',  ( -105.5641786249488661, -284.7322795454889501, -244.3862564384492941 ) ) ;
#73299 = CARTESIAN_POINT ( 'NONE',  ( 34.31083767777736426, -276.6524942850991238, -253.9599627617523083 ) ) ;
#73300 = CARTESIAN_POINT ( 'NONE',  ( 36.83860575284516869, -291.6853601666521740, -279.1282048728275527 ) ) ;
#73301 = AXIS2_PLACEMENT_3D ( 'NONE', #90372, #77131, #17968 ) ;
#73302 = CARTESIAN_POINT ( 'NONE',  ( -67.20508691652135269, -272.4465815549076524, -203.3002892612697678 ) ) ;
#73303 = ORIENTED_EDGE ( 'NONE', *, *, #16325, .F. ) ;
#73304 = CARTESIAN_POINT ( 'NONE',  ( 168.1488725781630649, 234.1813984995739588, -193.4213935641190858 ) ) ;
#73305 = CARTESIAN_POINT ( 'NONE',  ( 35.46503039139748381, -293.5358602183426910, -295.5229250387068305 ) ) ;
#73306 = CARTESIAN_POINT ( 'NONE',  ( 26.16677050198359922, -288.9475975164053807, -231.5282922457939776 ) ) ;
#73307 = CARTESIAN_POINT ( 'NONE',  ( -112.5880822664892946, -297.8186922332217819, -255.4788516716729987 ) ) ;
#73308 = CARTESIAN_POINT ( 'NONE',  ( -49.44656484132194407, -286.5452997819895700, -198.2167944679387404 ) ) ;
#73309 = CARTESIAN_POINT ( 'NONE',  ( -112.2574127015945038, -277.4008211540931370, -287.1079452577531583 ) ) ;
#73310 = CARTESIAN_POINT ( 'NONE',  ( 0.4975826701656294593, -295.2130402791743222, -337.3202956423671139 ) ) ;
#73311 = CARTESIAN_POINT ( 'NONE',  ( -75.06949527116447030, -287.6888276375071882, -336.0643823954877689 ) ) ;
#73312 = CARTESIAN_POINT ( 'NONE',  ( 38.30367215542386106, -293.7069653295882858, -256.0950062600824708 ) ) ;
#73313 = CARTESIAN_POINT ( 'NONE',  ( -12.25692811675622806, -292.7208376572637576, -201.7299579199793413 ) ) ;
#73314 = CARTESIAN_POINT ( 'NONE',  ( 121.3887860922853150, -299.5541904835127980, -195.3611179825600175 ) ) ;
#73315 = CARTESIAN_POINT ( 'NONE',  ( 154.0301839823544867, 204.4104515754077056, -214.4894503004110504 ) ) ;
#73316 = CARTESIAN_POINT ( 'NONE',  ( -29.55312618109221390, -287.6692180648167323, -194.4529769964728700 ) ) ;
#73317 = CARTESIAN_POINT ( 'NONE',  ( 25.22466315766302358, -284.4094976428775112, -220.5068182859052968 ) ) ;
#73318 = ORIENTED_EDGE ( 'NONE', *, *, #11195, .F. ) ;
#73319 = ADVANCED_FACE ( 'NONE', ( #78377 ), #45248, .F. ) ;
#73320 = CARTESIAN_POINT ( 'NONE',  ( -64.69829773598945621, -279.0528829450703370, -198.4375228125011290 ) ) ;
#73321 = CARTESIAN_POINT ( 'NONE',  ( 29.80712511043030233, -283.9903010158200800, -303.5100491196825487 ) ) ;
#73322 = CARTESIAN_POINT ( 'NONE',  ( -87.58154494375190779, -231.1970665811080607, -346.4935346893788619 ) ) ;
#73323 = CARTESIAN_POINT ( 'NONE',  ( -62.98646271852845047, -284.2993606257402348, -198.3822846776303379 ) ) ;
#73324 = CARTESIAN_POINT ( 'NONE',  ( 34.46457145140765022, -285.8884975024154187, -290.1780020825075326 ) ) ;
#73325 = CARTESIAN_POINT ( 'NONE',  ( 25.88648902800262519, -276.8546588469999392, -228.6178361735904900 ) ) ;
#73326 = CARTESIAN_POINT ( 'NONE',  ( -105.8657291402628005, -297.3839266291053605, -244.8686390916215885 ) ) ;
#73327 = CARTESIAN_POINT ( 'NONE',  ( -12.85964614132110384, -293.4121405110421392, -339.7102751670778389 ) ) ;
#73328 = CARTESIAN_POINT ( 'NONE',  ( -97.62216726411656964, -279.8432949026999381, -222.6161908273719234 ) ) ;
#73329 = CARTESIAN_POINT ( 'NONE',  ( -64.33314122881161268, -277.4143151077616380, -338.2415067401982469 ) ) ;
#73330 = CARTESIAN_POINT ( 'NONE',  ( -66.12401788427584393, -274.7638433940988421, -199.2620493716995895 ) ) ;
#73331 = CARTESIAN_POINT ( 'NONE',  ( -56.85869194969789220, -276.2183105691128731, -344.5818445310513880 ) ) ;
#73332 = CARTESIAN_POINT ( 'NONE',  ( 167.6033460893912093, 232.7025357864140460, -192.5994064319566803 ) ) ;
#73333 = CARTESIAN_POINT ( 'NONE',  ( 33.81920494783065578, -273.8600055619412501, -294.2092368426298208 ) ) ;
#73334 = CARTESIAN_POINT ( 'NONE',  ( -113.7762999216845685, -297.9508232105048933, -272.4717677076108657 ) ) ;
#73335 = CARTESIAN_POINT ( 'NONE',  ( 31.98288692825981272, -278.4805209788417528, -303.7098442033569654 ) ) ;
#73336 = DIRECTION ( 'NONE',  ( 1.000000000000000000, -1.124465274301078034E-16, 0.000000000000000000 ) ) ;
#73337 = CARTESIAN_POINT ( 'NONE',  ( -93.50072443926489996, -286.2981365367771218, -223.2401028949195165 ) ) ;
#73338 = CARTESIAN_POINT ( 'NONE',  ( -104.8731547512770845, -285.8559955635038250, -305.3108490011269396 ) ) ;
#73339 = CARTESIAN_POINT ( 'NONE',  ( -14.52632670182640950, -285.7043010160943481, -200.8576710055064609 ) ) ;
#73340 = CARTESIAN_POINT ( 'NONE',  ( -94.23565343474145095, -276.2927183532285085, -317.3864407143046265 ) ) ;
#73341 = CARTESIAN_POINT ( 'NONE',  ( -70.74993889211815201, -285.3579607533563376, -336.6682800726266578 ) ) ;
#73342 = CARTESIAN_POINT ( 'NONE',  ( -62.52788662254108942, -278.1984073910530810, -201.0514751904430000 ) ) ;
#73343 = CARTESIAN_POINT ( 'NONE',  ( -40.50540227777504754, -278.1725066775952655, -343.6144507909678509 ) ) ;
#73344 = CARTESIAN_POINT ( 'NONE',  ( 198.5844002719293258, 69.20872177009273685, -9.718513320358827201 ) ) ;
#73345 = CARTESIAN_POINT ( 'NONE',  ( -108.5963038186732490, -273.2573449458428172, -254.2127467091688118 ) ) ;
#73346 = CARTESIAN_POINT ( 'NONE',  ( -2.472573370753142097, -281.3043528291304938, -201.8752396110628808 ) ) ;
#73347 = CARTESIAN_POINT ( 'NONE',  ( 25.88333741668704135, -282.6243774972468259, -314.2262977005315179 ) ) ;
#73348 = ORIENTED_EDGE ( 'NONE', *, *, #64488, .F. ) ;
#73349 = ORIENTED_EDGE ( 'NONE', *, *, #28796, .F. ) ;
#73350 = CARTESIAN_POINT ( 'NONE',  ( 196.3596534549891999, 42.20329003140924584, 13.36271651522391757 ) ) ;
#73351 = CARTESIAN_POINT ( 'NONE',  ( 22.86522010551105666, -288.7890748681822402, -224.3460264735121825 ) ) ;
#73352 = CARTESIAN_POINT ( 'NONE',  ( -113.8968530000804122, -289.2263387567450650, -271.2064844508544752 ) ) ;
#73353 = CARTESIAN_POINT ( 'NONE',  ( -63.12682566572913601, -296.9048343114305908, -201.8405313894990343 ) ) ;
#73354 = CARTESIAN_POINT ( 'NONE',  ( -3.358913634876510734, -291.8376574636761234, -201.3648400860364802 ) ) ;
#73355 = CARTESIAN_POINT ( 'NONE',  ( 27.63271879142160614, -286.5028567980066327, -305.2408184777386282 ) ) ;
#73356 = CARTESIAN_POINT ( 'NONE',  ( 35.09854842600260838, -286.2963819804556920, -283.3143147896302594 ) ) ;
#73357 = CARTESIAN_POINT ( 'NONE',  ( -37.29595047966345334, -287.2577785869079889, -196.9515515626052036 ) ) ;
#73358 = CARTESIAN_POINT ( 'NONE',  ( 10.59707575819634329, -295.1948066931273615, -210.1954327657594490 ) ) ;
#73359 = CARTESIAN_POINT ( 'NONE',  ( -31.94459168598327281, -290.9843433514939761, -345.2178688343421413 ) ) ;
#73360 = CARTESIAN_POINT ( 'NONE',  ( -88.26852729870090286, -287.7633390339995572, -325.6466196857214754 ) ) ;
#73361 = CARTESIAN_POINT ( 'NONE',  ( -95.15015134527023122, -286.1250771809836237, -225.3786402061973035 ) ) ;
#73362 = CARTESIAN_POINT ( 'NONE',  ( -107.0876376419144407, -292.1879274363793115, -298.3884729142890819 ) ) ;
#73363 = CARTESIAN_POINT ( 'NONE',  ( 197.2116943569230898, 214.9331615741067765, -12.42446933126075592 ) ) ;
#73364 = CARTESIAN_POINT ( 'NONE',  ( 199.4392256788250677, 65.82574266882504332, -7.741079165001071516 ) ) ;
#73365 = CARTESIAN_POINT ( 'NONE',  ( -57.70197485341622468, -275.7705635469097274, -197.7543666000710516 ) ) ;
#73366 = AXIS2_PLACEMENT_3D ( 'NONE', #47684, #76585, #10765 ) ;
#73367 = CARTESIAN_POINT ( 'NONE',  ( -4.265437929646443749, -279.6968935445552233, -205.0895322268834207 ) ) ;
#73368 = CARTESIAN_POINT ( 'NONE',  ( -66.10566474741330012, -281.4284039943358380, -339.6400536383988538 ) ) ;
#73369 = CARTESIAN_POINT ( 'NONE',  ( -27.77809146484340630, -294.1309511784212987, -346.6553384539989793 ) ) ;
#73370 = CARTESIAN_POINT ( 'NONE',  ( -67.44947321883103086, -271.8916058150929871, -202.7343980839995936 ) ) ;
#73371 = CARTESIAN_POINT ( 'NONE',  ( -36.47343707306416150, -275.1210699945360716, -344.8087717291236913 ) ) ;
#73372 = CARTESIAN_POINT ( 'NONE',  ( -84.40338773409932571, -298.7040647819113133, -213.8460903892598708 ) ) ;
#73373 = CARTESIAN_POINT ( 'NONE',  ( 115.2448031289451222, -299.5541904835127980, -195.3611179825600175 ) ) ;
#73374 = CARTESIAN_POINT ( 'NONE',  ( -112.5950373509071056, -294.9266693593818900, -259.7358454896262856 ) ) ;
#73375 = CARTESIAN_POINT ( 'NONE',  ( 35.79463408042880701, -295.0899757926691223, -278.9615243916762779 ) ) ;
#73376 = EDGE_CURVE ( 'NONE', #93680, #30132, #58006, .T. ) ;
#73377 = DIRECTION ( 'NONE',  ( -1.000000000000000000, 0.000000000000000000, 0.000000000000000000 ) ) ;
#73378 = CLOSED_SHELL ( 'NONE', ( #88963, #12132, #16268, #66192, #39335, #2831, #45593, #39428, #22795, #56383, #12938, #92215, #63881, #7828, #14492, #19720, #72661, #26447, #82116, #3333, #496, #51867, #27761, #44310, #28653, #33680, #54216, #37952, #5274, #65701, #86089, #35486, #38330, #9523, #86734, #34802, #65528, #71229, #72871, #10298, #88140, #7380, #33038, #11031, #93133, #82778, #85965, #4301, #4457, #79803, #75812, #82798, #3005, #38059, #31464, #42947, #91622, #18033, #51751, #50939, #23451, #4778 ) ) ;
#73379 = CARTESIAN_POINT ( 'NONE',  ( -31.57946010632110045, -295.7805257696567764, -343.3455473247669261 ) ) ;
#73380 = DIRECTION ( 'NONE',  ( 0.000000000000000000, -1.000000000000000000, 0.000000000000000000 ) ) ;
#73382 = CARTESIAN_POINT ( 'NONE',  ( -109.8044857332493649, -296.4301988708591580, -279.6058443605987804 ) ) ;
#73381 = CARTESIAN_POINT ( 'NONE',  ( -82.27446949089110717, -283.4629807521067164, -209.8026517001472087 ) ) ;
#73383 = CARTESIAN_POINT ( 'NONE',  ( -113.5993743774286173, -284.4140470798727733, -281.4038888172017323 ) ) ;
#73384 = CARTESIAN_POINT ( 'NONE',  ( 37.25030625446895982, -283.6269863695704316, -282.4980855276584180 ) ) ;
#73385 = CARTESIAN_POINT ( 'NONE',  ( 28.68259623934678260, -286.7014099627325550, -230.6788079329030552 ) ) ;
#73386 = CARTESIAN_POINT ( 'NONE',  ( 18.11349744355580782, -290.8490223214878938, -220.0382006200393903 ) ) ;
#73387 = CARTESIAN_POINT ( 'NONE',  ( -113.1999759985792480, -277.7429151515743797, -282.9640846433767933 ) ) ;
#73388 = CARTESIAN_POINT ( 'NONE',  ( 35.77081079830085031, -273.2666405000204009, -287.0812184334320705 ) ) ;
#73389 = CARTESIAN_POINT ( 'NONE',  ( -48.18343439339133027, -259.3094209318401795, -498.0507307272308140 ) ) ;
#73390 = CARTESIAN_POINT ( 'NONE',  ( 19.83412559953331566, -285.6997226897290147, -224.3188636742244171 ) ) ;
#73391 = CARTESIAN_POINT ( 'NONE',  ( -65.34700925199277322, -288.3299657512839076, -341.8118834513197157 ) ) ;
#73392 = CARTESIAN_POINT ( 'NONE',  ( 11.63197158325052172, -285.8906705383787994, 52.50000000000000711 ) ) ;
#73393 = CARTESIAN_POINT ( 'NONE',  ( -95.46946979002640887, -280.6516830769908211, -220.7449602281085390 ) ) ;
#73395 = CARTESIAN_POINT ( 'NONE',  ( 33.96014260557003439, -281.4266088303234028, -286.1134101859606176 ) ) ;
#73394 = CARTESIAN_POINT ( 'NONE',  ( -16.97616787945061390, -292.8107036458754919, -342.9661946813372992 ) ) ;
#73396 = CARTESIAN_POINT ( 'NONE',  ( 22.28798240855449109, -294.3729556434117285, -319.0983544261346196 ) ) ;
#73397 = EDGE_CURVE ( 'NONE', #49342, #81684, #57412, .T. ) ;
#73398 = CARTESIAN_POINT ( 'NONE',  ( -58.75610754793071777, -281.7753311534822842, -198.4832785523234122 ) ) ;
#73399 = CARTESIAN_POINT ( 'NONE',  ( -90.58651960381676815, -294.8882949058986469, -320.7173387628213277 ) ) ;
#73400 = CARTESIAN_POINT ( 'NONE',  ( -111.2605617548323380, -270.7302858429516732, -256.4444337731355859 ) ) ;
#73401 = ORIENTED_EDGE ( 'NONE', *, *, #65309, .T. ) ;
#73402 = CARTESIAN_POINT ( 'NONE',  ( 201.5895683925353694, 64.65149228630519929, -9.583120145142274282 ) ) ;
#73403 = CARTESIAN_POINT ( 'NONE',  ( 37.20990563626141778, -283.5801565885579407, -274.0900424841237850 ) ) ;
#73404 = CARTESIAN_POINT ( 'NONE',  ( -107.8934490052756416, -296.3109284114943307, -251.3276888148648993 ) ) ;
#73405 = CARTESIAN_POINT ( 'NONE',  ( 0.000000000000000000, 3.000000000000000000, 9.000000000000001776 ) ) ;
#73406 = CARTESIAN_POINT ( 'NONE',  ( 21.31550574532286291, -278.4094976428775681, -223.6242672951989618 ) ) ;
#73407 = CARTESIAN_POINT ( 'NONE',  ( -3.887150547582444826, -273.6794228174786667, -201.1732918123841500 ) ) ;
#73408 = CARTESIAN_POINT ( 'NONE',  ( -107.0009799201558138, -290.6753033575084828, -248.4881913945528140 ) ) ;
#73409 = CARTESIAN_POINT ( 'NONE',  ( -108.9680842564292078, -280.2987881553842726, -253.0299653613055568 ) ) ;
#73410 = CARTESIAN_POINT ( 'NONE',  ( -66.14395323749488398, -275.2688830278736418, -202.4135600266756398 ) ) ;
#73411 = CARTESIAN_POINT ( 'NONE',  ( -4.490082734689728738, -284.2266176671263338, -339.1301797416747377 ) ) ;
#73412 = CARTESIAN_POINT ( 'NONE',  ( -2.949519435062557537, -279.3121831882229458, -205.5062231937867523 ) ) ;
#73413 = CARTESIAN_POINT ( 'NONE',  ( -77.40317453103840251, -279.5892618867650867, -333.8262779501284854 ) ) ;
#73414 = ORIENTED_EDGE ( 'NONE', *, *, #11080, .T. ) ;
#73415 = CARTESIAN_POINT ( 'NONE',  ( -58.11957492624920008, -273.6243368184152018, -196.1620496523297561 ) ) ;
#73416 = CARTESIAN_POINT ( 'NONE',  ( -92.76125680455017175, -293.1699437487487785, -220.6430816547708105 ) ) ;
#73417 = CARTESIAN_POINT ( 'NONE',  ( 121.3395553409046670, -299.5541904835127980, -195.3611179825600175 ) ) ;
#73418 = CARTESIAN_POINT ( 'NONE',  ( 196.3505989544111969, 71.51162351314616217, 11.47879840082592473 ) ) ;
#73419 = CARTESIAN_POINT ( 'NONE',  ( 37.59135382436164008, -291.8340384855868592, -281.5567825920381324 ) ) ;
#73420 = CARTESIAN_POINT ( 'NONE',  ( -40.77155924984348445, -273.5156386562580337, -197.3303878431244129 ) ) ;
#73421 = CARTESIAN_POINT ( 'NONE',  ( 140.6539576904058606, 250.0000000000000568, -10.49999999999999822 ) ) ;
#73422 = CARTESIAN_POINT ( 'NONE',  ( 6.085613872039532524, -294.1499191793195109, -207.6173840327866174 ) ) ;
#73424 = CARTESIAN_POINT ( 'NONE',  ( -19.49426017161818336, -293.4817097101841910, -195.8117653585358653 ) ) ;
#73423 = CARTESIAN_POINT ( 'NONE',  ( -85.33152481854864391, -281.9090924074130839, -210.2361428286349110 ) ) ;
#73425 = CARTESIAN_POINT ( 'NONE',  ( 19.14369761974795026, -288.8696336920671683, -221.2751905687686076 ) ) ;
#73426 = CARTESIAN_POINT ( 'NONE',  ( -39.22890033885708760, -275.0757377513016877, -345.1706555108469274 ) ) ;
#73427 = CARTESIAN_POINT ( 'NONE',  ( 10.60994894321324722, -278.3037151711751562, -327.2992734350243040 ) ) ;
#73428 = CARTESIAN_POINT ( 'NONE',  ( 19.04756446975046558, -292.3109305843573793, -318.9764817589377799 ) ) ;
#73429 = CARTESIAN_POINT ( 'NONE',  ( -5.485255548961519345, -282.3271771657813929, -201.6190462730926356 ) ) ;
#73430 = ORIENTED_EDGE ( 'NONE', *, *, #73993, .T. ) ;
#73431 = CARTESIAN_POINT ( 'NONE',  ( -65.32772441722129031, -283.0950140890378179, -337.8200315357108821 ) ) ;
#73432 = CARTESIAN_POINT ( 'NONE',  ( -67.25462164755556671, -280.7486541067718235, -199.7444794584705221 ) ) ;
#73433 = CARTESIAN_POINT ( 'NONE',  ( -41.56268591078386976, -281.8989929906176712, -346.8997220366821921 ) ) ;
#73434 = CARTESIAN_POINT ( 'NONE',  ( -75.20966505104998134, -278.4853843282359094, -337.1356449046780313 ) ) ;
#73435 = CARTESIAN_POINT ( 'NONE',  ( 37.80589588287897840, -276.9041209737049485, -257.0371625668553861 ) ) ;
#73436 = CARTESIAN_POINT ( 'NONE',  ( -67.74223827176244583, -294.1233781216987495, -207.3071070584150277 ) ) ;
#73437 = ORIENTED_EDGE ( 'NONE', *, *, #53943, .F. ) ;
#73438 = EDGE_LOOP ( 'NONE', ( #5558, #62957, #43225, #75529 ) ) ;
#73439 = CARTESIAN_POINT ( 'NONE',  ( -34.40682779664140156, -300.0890474781463695, -195.3601086761975694 ) ) ;
#73440 = CARTESIAN_POINT ( 'NONE',  ( -99.98284324329208061, -292.1540947248088855, -232.2781393385183151 ) ) ;
#73441 = CARTESIAN_POINT ( 'NONE',  ( -110.3792720864273633, -276.3735023082539897, -285.7676065126699996 ) ) ;
#73442 = CARTESIAN_POINT ( 'NONE',  ( -36.08087592867278204, -290.7967163796010368, -346.3502645340448112 ) ) ;
#73443 = CARTESIAN_POINT ( 'NONE',  ( -3.581817595367476681, -291.8587435186494190, -205.5216007122476753 ) ) ;
#73444 = CARTESIAN_POINT ( 'NONE',  ( 36.32465863657765226, -287.3391725553485117, -292.6058381088807892 ) ) ;
#73445 = CARTESIAN_POINT ( 'NONE',  ( 151.4851178187871312, 20.00000000000000000, 10.00000000000000000 ) ) ;
#73446 = CARTESIAN_POINT ( 'NONE',  ( -59.20435553746454360, -281.7396051465143501, -340.9021842449895416 ) ) ;
#73447 = CARTESIAN_POINT ( 'NONE',  ( -108.5873245166162349, -292.6844130281626235, -249.4610397006937603 ) ) ;
#73448 = CARTESIAN_POINT ( 'NONE',  ( -86.17121053890492988, -283.8405413143464671, -215.0988489160258155 ) ) ;
#73449 = CARTESIAN_POINT ( 'NONE',  ( -11.58590916279530703, -281.7097850003869439, -201.4750256364088443 ) ) ;
#73450 = CARTESIAN_POINT ( 'NONE',  ( -113.5784071327790343, -291.3751527329149553, -279.7873126814164948 ) ) ;
#73451 = CARTESIAN_POINT ( 'NONE',  ( -51.84570523314351220, -280.3540118765736224, -198.7019253458057051 ) ) ;
#73452 = CARTESIAN_POINT ( 'NONE',  ( -8.645651679697062164, -291.2143832910740571, -199.3361539045705513 ) ) ;
#73453 = CARTESIAN_POINT ( 'NONE',  ( 36.53312885592200132, -288.0873470717408509, -249.0377479990441714 ) ) ;
#73454 = CARTESIAN_POINT ( 'NONE',  ( 21.44605856236776376, -288.7136953007625380, -319.9950411762073941 ) ) ;
#73455 = CARTESIAN_POINT ( 'NONE',  ( -74.72193200695829773, -285.7061762645743670, -207.6577028508007743 ) ) ;
#73456 = ORIENTED_EDGE ( 'NONE', *, *, #64488, .T. ) ;
#73457 = CARTESIAN_POINT ( 'NONE',  ( 114.7448031289451222, -299.5541904835127980, -197.6977456432065310 ) ) ;
#73458 = CARTESIAN_POINT ( 'NONE',  ( 37.62610360218568673, -295.2687894611797219, -259.0492851422251874 ) ) ;
#73459 = CARTESIAN_POINT ( 'NONE',  ( -30.65086897587644188, -293.6540545197654524, -346.5748375549480329 ) ) ;
#73460 = CARTESIAN_POINT ( 'NONE',  ( -9.911321497236944111, -275.7436910945341424, -338.2789439992577627 ) ) ;
#73461 = CARTESIAN_POINT ( 'NONE',  ( -37.24537723390663047, -297.4019209128863395, -193.4622977766161966 ) ) ;
#73462 = CARTESIAN_POINT ( 'NONE',  ( 33.00291762288243547, -292.3203290233193457, -292.3234153618646474 ) ) ;
#73463 = CARTESIAN_POINT ( 'NONE',  ( -111.2547852393867913, -294.7418986956548110, -274.2120737867838329 ) ) ;
#73464 = CARTESIAN_POINT ( 'NONE',  ( 21.30185987935800185, -294.1407577732709910, -226.2242470523301279 ) ) ;
#73465 = CARTESIAN_POINT ( 'NONE',  ( 20.77664008092435566, -295.2582137918780631, -315.0637147690405868 ) ) ;
#73466 = CARTESIAN_POINT ( 'NONE',  ( 113.5000000000000568, -192.7866584945343504, -490.8867980474134356 ) ) ;
#73467 = CARTESIAN_POINT ( 'NONE',  ( -67.51421412072745909, -293.4468762690883068, -339.2062182335864122 ) ) ;
#73468 = CARTESIAN_POINT ( 'NONE',  ( -52.23673056871682974, -299.8617427440566985, -196.8027610985576530 ) ) ;
#73469 = CARTESIAN_POINT ( 'NONE',  ( -63.89506220021108618, -290.3482339748051686, -338.6674144032093636 ) ) ;
#73470 = CARTESIAN_POINT ( 'NONE',  ( -7.975911204908399554, -294.9898209940682250, -337.2307983939592759 ) ) ;
#73471 = CARTESIAN_POINT ( 'NONE',  ( -95.56306570372231590, -281.1888393503309658, -222.5009010000722469 ) ) ;
#73472 = CARTESIAN_POINT ( 'NONE',  ( -77.22107345109070309, -278.2145518185436117, -205.0086478154535143 ) ) ;
#73473 = VERTEX_POINT ( 'NONE', #230 ) ;
#73474 = CARTESIAN_POINT ( 'NONE',  ( -29.84056299386756450, -273.4933441729980359, -193.8297797727026648 ) ) ;
#73475 = CARTESIAN_POINT ( 'NONE',  ( 20.81607630902843198, -278.9882978791437154, -223.8962146469456513 ) ) ;
#73476 = CARTESIAN_POINT ( 'NONE',  ( -110.5628192823497500, -277.2193277152295536, -249.2635321963098249 ) ) ;
#73477 = CARTESIAN_POINT ( 'NONE',  ( -101.8254075753430072, -277.0691194804316524, -231.6351083500380241 ) ) ;
#73478 = EDGE_CURVE ( 'NONE', #25873, #86239, #84604, .T. ) ;
#73479 = CARTESIAN_POINT ( 'NONE',  ( -108.5052338887173562, -271.3746457240353607, -251.4275288122364032 ) ) ;
#73480 = FACE_OUTER_BOUND ( 'NONE', #19925, .T. ) ;
#73481 = CARTESIAN_POINT ( 'NONE',  ( 194.9270631639382430, 25.19695901056785914, 13.71261800098177730 ) ) ;
#73482 = CARTESIAN_POINT ( 'NONE',  ( -85.44330521762415742, -289.4115182660726759, -212.2878472769111511 ) ) ;
#73483 = CARTESIAN_POINT ( 'NONE',  ( -111.9945708100198374, -290.7888183149231622, -251.4414009962390821 ) ) ;
#73484 = CARTESIAN_POINT ( 'NONE',  ( -13.66470444066770362, -276.3589537348761382, -199.0208887977689756 ) ) ;
#73485 = CARTESIAN_POINT ( 'NONE',  ( -95.30835309555229173, -271.2084113262650362, -222.7504172643921265 ) ) ;
#73486 = CARTESIAN_POINT ( 'NONE',  ( -52.13216563256072789, -285.0647485861065888, -194.9052455788024929 ) ) ;
#73487 = FACE_OUTER_BOUND ( 'NONE', #12424, .T. ) ;
#73488 = CARTESIAN_POINT ( 'NONE',  ( -63.69339817169549178, -281.3953674949432866, -340.6333399312136976 ) ) ;
#73489 = VECTOR ( 'NONE', #59100, 1000.000000000000000 ) ;
#73490 = CARTESIAN_POINT ( 'NONE',  ( 201.0876323342543799, 25.81167821795959938, 9.999999999999998224 ) ) ;
#73491 = CARTESIAN_POINT ( 'NONE',  ( -36.18455904326116013, -290.8618652277949082, -196.9606216599541142 ) ) ;
#73492 = CARTESIAN_POINT ( 'NONE',  ( -46.86016132879224472, -284.0697312434418222, -196.6870396424370142 ) ) ;
#73493 = CARTESIAN_POINT ( 'NONE',  ( 195.4994389829729755, 25.60173194700487542, 14.63396631094618172 ) ) ;
#73494 = DIRECTION ( 'NONE',  ( 1.000000000000000000, -0.000000000000000000, -0.000000000000000000 ) ) ;
#73495 = CARTESIAN_POINT ( 'NONE',  ( 18.23696744037549067, -290.8490223206248970, -219.9260807567870586 ) ) ;
#73496 = CARTESIAN_POINT ( 'NONE',  ( -91.54168364009143488, -279.4399775163562936, -320.5233721338743749 ) ) ;
#73497 = CARTESIAN_POINT ( 'NONE',  ( -92.13892377627445285, -285.0191047458878870, -323.8893628508005236 ) ) ;
#73499 = CARTESIAN_POINT ( 'NONE',  ( -44.02437600801533790, -285.9653070484921500, -197.6676392992300180 ) ) ;
#73498 = CARTESIAN_POINT ( 'NONE',  ( -73.23877733225960185, -271.6602502115656534, -203.8145117498533239 ) ) ;
#73500 = CARTESIAN_POINT ( 'NONE',  ( 24.27704337199864781, -276.4243948019457093, -230.1304659065303042 ) ) ;
#73501 = CARTESIAN_POINT ( 'NONE',  ( -74.08555146273253911, -278.3567728226007034, -333.6263621230654053 ) ) ;
#73502 = EDGE_CURVE ( 'NONE', #21957, #66639, #39236, .T. ) ;
#73503 = EDGE_CURVE ( 'NONE', #50851, #64529, #75555, .T. ) ;
#73504 = CARTESIAN_POINT ( 'NONE',  ( -93.81163797262449577, -285.8669174654083918, -319.7184555395067491 ) ) ;
#73505 = ORIENTED_EDGE ( 'NONE', *, *, #58044, .F. ) ;
#73506 = FACE_OUTER_BOUND ( 'NONE', #70671, .T. ) ;
#73507 = CARTESIAN_POINT ( 'NONE',  ( -69.52985433128951342, -295.2975184575709591, -340.3249811405499372 ) ) ;
#73508 = CARTESIAN_POINT ( 'NONE',  ( 36.18317175677773889, -289.3621035366091974, -257.1883365611865884 ) ) ;
#73509 = CARTESIAN_POINT ( 'NONE',  ( 193.5162140859150668, 249.5000000000000568, 17.51463615629763027 ) ) ;
#73510 = CARTESIAN_POINT ( 'NONE',  ( -115.3430155898818299, -275.2662352645559167, -252.5904736702033517 ) ) ;
#73511 = CARTESIAN_POINT ( 'NONE',  ( -111.0363889025125133, -277.7397006396163874, -249.1341220442039628 ) ) ;
#73512 = CARTESIAN_POINT ( 'NONE',  ( -88.10125266742251426, -289.7554440269162797, -213.5288363139162868 ) ) ;
#73513 = APPLICATION_CONTEXT ( 'automotive_design' ) ;
#73514 = CARTESIAN_POINT ( 'NONE',  ( -110.5593206749061608, -285.9572980919892871, -279.1601770277165429 ) ) ;
#73515 = CARTESIAN_POINT ( 'NONE',  ( -37.02619628547270025, -281.8162981058169976, -196.3484537016190643 ) ) ;
#73516 = CARTESIAN_POINT ( 'NONE',  ( 34.29546097117965076, -288.6387165076610586, -243.7768474168693160 ) ) ;
#73517 = CARTESIAN_POINT ( 'NONE',  ( 37.34145334822082418, -283.4568815341990557, -262.9284876403270346 ) ) ;
#73518 = CARTESIAN_POINT ( 'NONE',  ( -25.76787376620716330, -277.0752797242349743, -346.4863210879388475 ) ) ;
#73519 = CARTESIAN_POINT ( 'NONE',  ( -96.57932617472518189, -295.1973952869595337, -224.9227868701736668 ) ) ;
#73520 = CARTESIAN_POINT ( 'NONE',  ( -114.3849361902278190, -278.3699000112984550, -271.6062780342882661 ) ) ;
#73521 = CARTESIAN_POINT ( 'NONE',  ( -85.01545242137235903, -299.3089474755935839, -213.1227606144830418 ) ) ;
#73522 = DIRECTION ( 'NONE',  ( -0.000000000000000000, -1.000000000000000000, -0.000000000000000000 ) ) ;
#73523 = CARTESIAN_POINT ( 'NONE',  ( -110.4683760289727132, -293.2662352645559167, -253.7030783399848985 ) ) ;
#73524 = CARTESIAN_POINT ( 'NONE',  ( 1.913946225635702492, -272.8097389662971750, -205.2998526814471063 ) ) ;
#73525 = DIRECTION ( 'NONE',  ( 1.000000000000000000, 0.000000000000000000, 0.000000000000000000 ) ) ;
#73526 = CARTESIAN_POINT ( 'NONE',  ( -106.5009479060917243, -278.3744678719471608, -246.6476364827599355 ) ) ;
#73527 = CARTESIAN_POINT ( 'NONE',  ( 28.76108799874752364, -277.2636781540074367, -309.0706790704900868 ) ) ;
#73528 = CARTESIAN_POINT ( 'NONE',  ( -93.26835507352255661, -282.8908476406718933, -322.9639397607558635 ) ) ;
#73529 = CARTESIAN_POINT ( 'NONE',  ( -66.71078729516291617, -291.2022724127160132, -338.3528364119063667 ) ) ;
#73530 = CARTESIAN_POINT ( 'NONE',  ( 52.55129206424644650, -300.6784332621725184, -194.0316613479411672 ) ) ;
#73531 = CARTESIAN_POINT ( 'NONE',  ( -54.52111395608655897, -299.0412168876722490, -195.7094170107499735 ) ) ;
#73532 = CARTESIAN_POINT ( 'NONE',  ( 37.54270597493783868, -295.5572517193583053, -270.7445168673075955 ) ) ;
#73533 = CARTESIAN_POINT ( 'NONE',  ( 33.97081688424970736, -279.8473453392966235, -293.2134667184989212 ) ) ;
#73534 = CARTESIAN_POINT ( 'NONE',  ( -70.19261666810130862, -271.6372005002476726, -203.3337796091085465 ) ) ;
#73535 = CARTESIAN_POINT ( 'NONE',  ( -113.3554383386322684, -286.2284728579659259, -264.3320398969979124 ) ) ;
#73536 = CARTESIAN_POINT ( 'NONE',  ( -21.07406231277025199, -287.7587972689769344, -341.8425143912570547 ) ) ;
#73537 = CARTESIAN_POINT ( 'NONE',  ( 204.8861687383550816, 294.6280919591721386, -68.62753702822789137 ) ) ;
#73538 = EDGE_LOOP ( 'NONE', ( #89326, #26727, #60, #82842 ) ) ;
#73539 = CARTESIAN_POINT ( 'NONE',  ( 14.19281757544087696, -286.9201075293059944, -326.8491100629050266 ) ) ;
#73540 = CARTESIAN_POINT ( 'NONE',  ( -29.17496981944978529, -288.6125235040371422, -342.9241388872305834 ) ) ;
#73541 = ORIENTED_EDGE ( 'NONE', *, *, #55554, .F. ) ;
#73542 = CARTESIAN_POINT ( 'NONE',  ( -112.6971453944939014, -285.8141752795130515, -255.8350001204779289 ) ) ;
#73543 = CARTESIAN_POINT ( 'NONE',  ( 35.62329281830566430, -275.9375067157598096, -274.3095437789028210 ) ) ;
#73544 = CARTESIAN_POINT ( 'NONE',  ( 22.87395351230433960, -291.8345116604801319, -222.8473119626277992 ) ) ;
#73545 = CARTESIAN_POINT ( 'NONE',  ( 37.45117085204278595, -282.4280039008593803, -288.2873762213042710 ) ) ;
#73546 = CARTESIAN_POINT ( 'NONE',  ( 35.81953328149513993, -283.3488454211931185, -292.2258040050188015 ) ) ;
#73547 = CARTESIAN_POINT ( 'NONE',  ( 6.916322366265646338, -282.8014735130303166, -333.4102036834366913 ) ) ;
#73548 = CARTESIAN_POINT ( 'NONE',  ( -43.75717589290088227, -280.3022688686673973, -197.5720960716281525 ) ) ;
#73549 = CARTESIAN_POINT ( 'NONE',  ( -106.6662871844225293, -275.6237833571633473, -303.7098442033569086 ) ) ;
#73550 = CARTESIAN_POINT ( 'NONE',  ( -104.0393943735737139, -256.4255047920307788, -326.8026429627599327 ) ) ;
#73551 = EDGE_LOOP ( 'NONE', ( #68319, #2029, #14401, #53030 ) ) ;
#73552 = CARTESIAN_POINT ( 'NONE',  ( -32.27152545579270537, -278.9883586153231363, -345.0737192621859890 ) ) ;
#73553 = CARTESIAN_POINT ( 'NONE',  ( 24.38510183189676184, -22.52970021484863139, -344.5096856694104872 ) ) ;
#73554 = CARTESIAN_POINT ( 'NONE',  ( -64.14634942166337339, -182.0482023548213135, -359.0711594925775216 ) ) ;
#73555 = CARTESIAN_POINT ( 'NONE',  ( -110.1510354040710240, -295.9939963101326157, -263.2815451879206989 ) ) ;
#73556 = CARTESIAN_POINT ( 'NONE',  ( 38.00292448592740868, -292.8640026154727138, -254.7172259279338391 ) ) ;
#73557 = CARTESIAN_POINT ( 'NONE',  ( -93.06201919177942727, -239.3495457806625666, -338.7989358161790392 ) ) ;
#73559 = CARTESIAN_POINT ( 'NONE',  ( -85.21934997310023618, -288.1258474033264747, -326.5905929868767998 ) ) ;
#73558 = CARTESIAN_POINT ( 'NONE',  ( -98.60903269017077832, -295.7391533980123768, -224.6783599883584657 ) ) ;
#73560 = CARTESIAN_POINT ( 'NONE',  ( -28.72955071285097262, -296.8023593552213129, -344.1469527926191745 ) ) ;
#73561 = CARTESIAN_POINT ( 'NONE',  ( 23.92983238359569853, -289.4269436513414462, -310.9678868490682930 ) ) ;
#73562 = VERTEX_POINT ( 'NONE', #72666 ) ;
#73563 = CARTESIAN_POINT ( 'NONE',  ( -44.76091528411387799, -296.0849945215481966, -346.8196975503954604 ) ) ;
#73564 = CARTESIAN_POINT ( 'NONE',  ( 16.01512698248800959, -287.3268878716897348, -220.4323636757369513 ) ) ;
#73565 = CARTESIAN_POINT ( 'NONE',  ( -80.38913755756647106, -296.2782704323740290, -206.9338987277804449 ) ) ;
#73566 = CARTESIAN_POINT ( 'NONE',  ( -79.51435165108738090, -292.3012975219951386, -206.0664719310573787 ) ) ;
#73567 = CARTESIAN_POINT ( 'NONE',  ( 29.52429437753199792, -294.5403406068215304, -308.5274708873618579 ) ) ;
#73568 = CARTESIAN_POINT ( 'NONE',  ( -46.99656601744062812, -292.0927803124943125, -198.0024034476047348 ) ) ;
#73569 = ORIENTED_EDGE ( 'NONE', *, *, #76892, .T. ) ;
#73570 = DIRECTION ( 'NONE',  ( -1.000000000000000000, 0.000000000000000000, 0.000000000000000000 ) ) ;
#73571 = CARTESIAN_POINT ( 'NONE',  ( -34.18823181446925474, -276.0116720405713977, -194.8669470971723285 ) ) ;
#73572 = CARTESIAN_POINT ( 'NONE',  ( 9.280884680798010322, -273.4717647087152841, -209.5800082262151420 ) ) ;
#73573 = EDGE_CURVE ( 'NONE', #9702, #14431, #2092, .T. ) ;
#73574 = ORIENTED_EDGE ( 'NONE', *, *, #54065, .T. ) ;
#73575 = CARTESIAN_POINT ( 'NONE',  ( 18.85397613791859328, -275.7771323264880721, -322.9117875524294732 ) ) ;
#73576 = CARTESIAN_POINT ( 'NONE',  ( -35.10209894702379785, -296.5605624607194386, -196.6683717249171366 ) ) ;
#73577 = CARTESIAN_POINT ( 'NONE',  ( -51.53994489043085991, -275.3752491977510317, -343.2258922102836323 ) ) ;
#73578 = CARTESIAN_POINT ( 'NONE',  ( -110.6508120073928012, -273.6316498264152983, -270.3748327195528987 ) ) ;
#73579 = CARTESIAN_POINT ( 'NONE',  ( -76.70074840789855841, -274.4522545458730178, -208.6013109364660068 ) ) ;
#73580 = CARTESIAN_POINT ( 'NONE',  ( -91.46325377951568214, -275.0546296546694407, -217.0241566589600097 ) ) ;
#73581 = CARTESIAN_POINT ( 'NONE',  ( -82.57225900220493031, -271.4582358020668380, -210.0247447229830584 ) ) ;
#73582 = CARTESIAN_POINT ( 'NONE',  ( -86.55248167706605500, -296.4092677367946180, -324.4184176492847200 ) ) ;
#73583 = CARTESIAN_POINT ( 'NONE',  ( -31.57413723428266650, -293.5527803757138940, -343.7745020587157683 ) ) ;
#73584 = CARTESIAN_POINT ( 'NONE',  ( 152.4536156746142410, 250.5000000000000568, -12.49999999999999289 ) ) ;
#73585 = CARTESIAN_POINT ( 'NONE',  ( 26.01977155947634301, -276.6221891280754335, -314.0979365405915473 ) ) ;
#73586 = CARTESIAN_POINT ( 'NONE',  ( 26.63550371709898101, -275.2373585112675300, -235.1001529562408621 ) ) ;
#73587 = CARTESIAN_POINT ( 'NONE',  ( -112.5105011902911940, -283.4197183812052003, -255.8397595530175295 ) ) ;
#73588 = CARTESIAN_POINT ( 'NONE',  ( -112.4783393714420612, -298.5973368360756126, -266.8470104335506221 ) ) ;
#73589 = CYLINDRICAL_SURFACE ( 'NONE', #9712, 5.000000000000000888 ) ;
#73590 = CARTESIAN_POINT ( 'NONE',  ( -60.01899645911787218, -284.9477541320167688, -200.8029268200316153 ) ) ;
#73591 = CARTESIAN_POINT ( 'NONE',  ( -104.2768329931730591, -277.2143839710297470, -238.6549452784948642 ) ) ;
#73592 = CARTESIAN_POINT ( 'NONE',  ( -54.10565710626204350, -275.8462268937993827, -342.0680240110532964 ) ) ;
#73593 = CARTESIAN_POINT ( 'NONE',  ( 22.06278547508822996, -284.1798132737311562, -316.1650495222779682 ) ) ;
#73594 = CARTESIAN_POINT ( 'NONE',  ( 34.55660827295164239, -276.9508445634169220, -285.1179386099806266 ) ) ;
#73595 = DIRECTION ( 'NONE',  ( 0.000000000000000000, 1.000000000000000000, -0.000000000000000000 ) ) ;
#73596 = CARTESIAN_POINT ( 'NONE',  ( 31.12740628944732180, -274.3873129190076838, -303.9240512760351294 ) ) ;
#73597 = CARTESIAN_POINT ( 'NONE',  ( -76.55828462739536633, -281.5293517990301666, -206.1752872885249985 ) ) ;
#73598 = DIRECTION ( 'NONE',  ( -1.000000000000000000, 0.000000000000000000, 2.940294503956655304E-16 ) ) ;
#73599 = CARTESIAN_POINT ( 'NONE',  ( -80.14302953936375218, -287.3982680931641198, -208.0294958870294408 ) ) ;
#73600 = DIRECTION ( 'NONE',  ( 0.000000000000000000, 1.000000000000000000, 0.000000000000000000 ) ) ;
#73601 = CARTESIAN_POINT ( 'NONE',  ( -111.1587735898196740, -288.3807147593695959, -283.7006271285201819 ) ) ;
#73602 = CARTESIAN_POINT ( 'NONE',  ( 152.4536156746142410, 250.5000000000000568, -11.99999999999999289 ) ) ;
#73603 = CARTESIAN_POINT ( 'NONE',  ( -87.65882197998212177, -272.0168377754796438, -216.7243889523163602 ) ) ;
#73604 = CARTESIAN_POINT ( 'NONE',  ( -110.1548466265458899, -288.5033038766547975, -284.8869173526937857 ) ) ;
#73605 = CARTESIAN_POINT ( 'NONE',  ( -89.67076919512652466, -242.4121354169174367, -340.4712336312485377 ) ) ;
#73606 = CARTESIAN_POINT ( 'NONE',  ( 180.2296971224742776, 215.0000000000000568, -25.00500000000002387 ) ) ;
#73607 = CARTESIAN_POINT ( 'NONE',  ( 38.66592401597007012, -285.9396796532453777, -263.0431830986759110 ) ) ;
#73608 = CARTESIAN_POINT ( 'NONE',  ( -5.671344487890855213, -284.2287594886905140, -337.0340707484441509 ) ) ;
#73609 = CARTESIAN_POINT ( 'NONE',  ( -103.1514809971601636, -283.2936556743579786, -232.2690778310053474 ) ) ;
#73610 = CARTESIAN_POINT ( 'NONE',  ( -103.5563182522245427, -290.9670253668535338, -239.6263762938148716 ) ) ;
#73611 = CARTESIAN_POINT ( 'NONE',  ( 34.02258056972365097, -282.7417113555861192, -252.3512885425136574 ) ) ;
#73612 = CARTESIAN_POINT ( 'NONE',  ( 35.51213872565642760, -282.2597465318610261, -263.1252304925569661 ) ) ;
#73613 = CARTESIAN_POINT ( 'NONE',  ( -29.13079578455961638, -290.9286190153812299, -345.3200292045121387 ) ) ;
#73614 = CARTESIAN_POINT ( 'NONE',  ( -106.8259593728122212, -273.3102782501214278, -237.2298335425319920 ) ) ;
#73615 = CARTESIAN_POINT ( 'NONE',  ( 22.97762395984459616, -286.2495636713586009, -315.8681871320640084 ) ) ;
#73616 = CARTESIAN_POINT ( 'NONE',  ( 32.55306073937912004, -275.1373937609188829, -237.9274532511399229 ) ) ;
#73617 = CARTESIAN_POINT ( 'NONE',  ( 0.7266827954646818410, -294.5424129330547203, -206.1532911679029496 ) ) ;
#73618 = CARTESIAN_POINT ( 'NONE',  ( -48.18343439339133027, -273.4097382619042378, -437.2279360942457060 ) ) ;
#73619 = CARTESIAN_POINT ( 'NONE',  ( 209.8616357346608652, 36.89613957940318301, 12.90102856104451767 ) ) ;
#73620 = CARTESIAN_POINT ( 'NONE',  ( -13.38432790028948105, -281.4193779454259356, -339.8937658062558285 ) ) ;
#73621 = CARTESIAN_POINT ( 'NONE',  ( -53.75630876482585307, -275.2620294246369781, -343.7669595599688819 ) ) ;
#73622 = CARTESIAN_POINT ( 'NONE',  ( 175.2296996224750103, 250.0000000000000568, 0.000000000000000000 ) ) ;
#73623 = CARTESIAN_POINT ( 'NONE',  ( -111.8275183238527859, -294.7489197492780022, -286.4329351178544130 ) ) ;
#73624 = CARTESIAN_POINT ( 'NONE',  ( 30.27225721122531965, -274.5272212395023530, -242.4388574905363782 ) ) ;
#73625 = CARTESIAN_POINT ( 'NONE',  ( -44.38556875275366309, -293.4817096713564979, -196.9538921988186644 ) ) ;
#73626 = CARTESIAN_POINT ( 'NONE',  ( -98.50262588172678591, -292.0513734106139623, -229.9856137624763335 ) ) ;
#73628 = ADVANCED_FACE ( 'NONE', ( #66498 ), #69481, .F. ) ;
#73627 = CARTESIAN_POINT ( 'NONE',  ( -111.3308017882582277, -286.2687808127481048, -273.7059785551666096 ) ) ;
#73629 = CARTESIAN_POINT ( 'NONE',  ( 38.02811692269265365, -295.1368341769661470, -283.0101937569141342 ) ) ;
#73630 = CARTESIAN_POINT ( 'NONE',  ( 27.62468457497261554, -294.3341909124545737, -229.8547735300761303 ) ) ;
#73631 = CARTESIAN_POINT ( 'NONE',  ( -61.01517326468108138, -295.2013572955071936, -339.4695022721770101 ) ) ;
#73632 = CARTESIAN_POINT ( 'NONE',  ( 24.41072296049498291, -290.1295099034729787, -312.9471172831084118 ) ) ;
#73633 = CARTESIAN_POINT ( 'NONE',  ( -112.2186515861688605, -284.4935601749267562, -288.3736005969368534 ) ) ;
#73634 = CARTESIAN_POINT ( 'NONE',  ( -30.61929291252672414, -296.2155323273656791, -194.8032890324896300 ) ) ;
#73635 = CARTESIAN_POINT ( 'NONE',  ( -111.8755006756809678, -284.1429300677547189, -289.7450440725257863 ) ) ;
#73636 = CARTESIAN_POINT ( 'NONE',  ( -103.2987761474397104, -280.0664363699397654, -305.3112384798483276 ) ) ;
#73637 = ADVANCED_FACE ( 'NONE', ( #74512 ), #24119, .F. ) ;
#73638 = CARTESIAN_POINT ( 'NONE',  ( -35.91041942542822341, -284.8654224589693058, -196.9780004312582378 ) ) ;
#73639 = CARTESIAN_POINT ( 'NONE',  ( 37.64107877718053885, -285.5313494596636588, -268.7537868595474606 ) ) ;
#73640 = CARTESIAN_POINT ( 'NONE',  ( -110.1436823427174829, -276.9590822054922796, -249.3807255346758893 ) ) ;
#73641 = CARTESIAN_POINT ( 'NONE',  ( 169.8384340989974817, 275.0000000000000568, -24.41176470588234437 ) ) ;
#73642 = CARTESIAN_POINT ( 'NONE',  ( -83.68206542277228266, -284.9041392444616463, -213.8103550137312538 ) ) ;
#73643 = CARTESIAN_POINT ( 'NONE',  ( 32.03930184909863499, -283.1765404849241463, -302.9559011245347619 ) ) ;
#73644 = CARTESIAN_POINT ( 'NONE',  ( -100.4938694101102072, -289.0328068589779491, -314.0031129878314005 ) ) ;
#73645 = CARTESIAN_POINT ( 'NONE',  ( -67.37435104295154531, -279.0396481673462858, -340.3931127831607455 ) ) ;
#73646 = CARTESIAN_POINT ( 'NONE',  ( -23.01471920588848974, -278.1878725536130332, -345.5683734184902960 ) ) ;
#73647 = CARTESIAN_POINT ( 'NONE',  ( -107.9720426774477176, -278.6296312504761090, -251.8633180385693606 ) ) ;
#73648 = CARTESIAN_POINT ( 'NONE',  ( -36.74774989060677655, -276.0395415949509470, -195.7059825134823541 ) ) ;
#73649 = CARTESIAN_POINT ( 'NONE',  ( 32.18596526420508752, -293.1266176246269310, -237.1478765250244294 ) ) ;
#73650 = CARTESIAN_POINT ( 'NONE',  ( 29.86331424860502182, -285.9869643751569015, -303.2778989004222581 ) ) ;
#73651 = CARTESIAN_POINT ( 'NONE',  ( -66.72597154568701683, -293.2736642367675586, -200.0546103920527514 ) ) ;
#73652 = CARTESIAN_POINT ( 'NONE',  ( -53.22971009541089416, -294.1808874949066421, -341.9800572436694210 ) ) ;
#73653 = CARTESIAN_POINT ( 'NONE',  ( -10.48617270934868273, -294.3585642312414734, -338.2644914912154945 ) ) ;
#73654 = CARTESIAN_POINT ( 'NONE',  ( -111.6982683039011732, -291.8683150995925644, -251.5307162369283560 ) ) ;
#73655 = CARTESIAN_POINT ( 'NONE',  ( 19.75043096694295386, -281.5594486824153933, -224.7060937725205747 ) ) ;
#73656 = CARTESIAN_POINT ( 'NONE',  ( -29.08712034845651218, -297.0735580783419323, -193.6716999799625398 ) ) ;
#73657 = CARTESIAN_POINT ( 'NONE',  ( 37.27590481853643922, -287.9706976402507053, -251.7727931777235426 ) ) ;
#73658 = CARTESIAN_POINT ( 'NONE',  ( 23.25274569757171861, -280.3069879425341355, -315.8431871770719113 ) ) ;
#73659 = CARTESIAN_POINT ( 'NONE',  ( 36.36637689983501787, -288.1646676603711512, -292.6074415033127138 ) ) ;
#73660 = CARTESIAN_POINT ( 'NONE',  ( 15.04170935009452492, -287.1500975042685013, -219.4880809373403281 ) ) ;
#73661 = FACE_OUTER_BOUND ( 'NONE', #56962, .T. ) ;
#73662 = CARTESIAN_POINT ( 'NONE',  ( 172.0097273584857476, 242.6675468326081386, -178.1715083274182518 ) ) ;
#73663 = CARTESIAN_POINT ( 'NONE',  ( 200.5626873411542022, 290.1978221515497580, -82.34105553867769345 ) ) ;
#73664 = CARTESIAN_POINT ( 'NONE',  ( -48.64284848592895827, -276.3967582034913448, -342.6959930051543211 ) ) ;
#73665 = CARTESIAN_POINT ( 'NONE',  ( -104.5602964264674597, -277.0792661149073410, -299.7439102515596687 ) ) ;
#73666 = CARTESIAN_POINT ( 'NONE',  ( -31.90863132321499052, -297.6261228324871126, -193.4230956962402672 ) ) ;
#73667 = CARTESIAN_POINT ( 'NONE',  ( -101.2177587865138122, -255.4137508676264758, -324.7206257864939403 ) ) ;
#73668 = CARTESIAN_POINT ( 'NONE',  ( -14.75139343379857237, -275.4503660745291427, -343.5122475340449455 ) ) ;
#73669 = CARTESIAN_POINT ( 'NONE',  ( 31.32406147061892554, -295.7362650858349866, -303.0259344471818395 ) ) ;
#73670 = CARTESIAN_POINT ( 'NONE',  ( -3.613418446484706781, -293.0023189722448933, -205.5506909153884010 ) ) ;
#73671 = CARTESIAN_POINT ( 'NONE',  ( -20.56402232430869859, -299.0600260379783322, -193.5203716029971019 ) ) ;
#73672 = CARTESIAN_POINT ( 'NONE',  ( -23.71002232962655043, -287.5592647787937608, -342.6310344664944409 ) ) ;
#73673 = CARTESIAN_POINT ( 'NONE',  ( -107.9871450505454078, -273.5924978600625650, -239.8531773425202971 ) ) ;
#73674 = CARTESIAN_POINT ( 'NONE',  ( -93.61493184256664790, -297.3782216505862834, -223.8408820521546545 ) ) ;
#73675 = ORIENTED_EDGE ( 'NONE', *, *, #31692, .F. ) ;
#73676 = CARTESIAN_POINT ( 'NONE',  ( 170.7304434856092143, 275.5000000000000568, -24.91818181818181088 ) ) ;
#73677 = CARTESIAN_POINT ( 'NONE',  ( -112.6418127817504882, -280.3848279753441375, -277.2250614057640519 ) ) ;
#73678 = CARTESIAN_POINT ( 'NONE',  ( -108.4686597135302435, -279.3979180812686991, -288.1661847545949513 ) ) ;
#73679 = CARTESIAN_POINT ( 'NONE',  ( -111.1076879352521161, -280.5440751509220263, -252.0716311130798317 ) ) ;
#73680 = CARTESIAN_POINT ( 'NONE',  ( 3.328563963598885955, -273.0891978607116926, -208.8457701666081903 ) ) ;
#73681 = EDGE_CURVE ( 'NONE', #93112, #34264, #1763, .T. ) ;
#73682 = CARTESIAN_POINT ( 'NONE',  ( 184.7149167944524493, -12.49482340714361506, 10.00000000000000000 ) ) ;
#73683 = DIRECTION ( 'NONE',  ( -1.000000000000000000, 0.000000000000000000, 0.000000000000000000 ) ) ;
#73684 = CARTESIAN_POINT ( 'NONE',  ( -46.45856240551105287, -280.1000542919696841, -197.8815487093973786 ) ) ;
#73685 = CARTESIAN_POINT ( 'NONE',  ( 19.90870854953572788, -275.6577261825014489, -219.0330654206976533 ) ) ;
#73686 = CARTESIAN_POINT ( 'NONE',  ( 21.95293194294287176, -278.1820719610389006, -316.3074083321283752 ) ) ;
#73687 = CARTESIAN_POINT ( 'NONE',  ( -110.8784302436431943, -276.8647050264839322, -291.1205885337175232 ) ) ;
#73688 = ORIENTED_EDGE ( 'NONE', *, *, #88205, .T. ) ;
#73689 = DIRECTION ( 'NONE',  ( 0.4988042400434494761, -0.06911816301596634959, -0.8639542867860402486 ) ) ;
#73690 = CARTESIAN_POINT ( 'NONE',  ( 22.95449566359588189, -284.1466750916733304, -315.5581928751946066 ) ) ;
#73691 = CARTESIAN_POINT ( 'NONE',  ( -108.8662801307387298, -289.9518823065682227, -254.9716351141615291 ) ) ;
#73692 = CARTESIAN_POINT ( 'NONE',  ( -52.14552365770757092, -285.2161435861906966, -194.8471456306270682 ) ) ;
#73693 = CARTESIAN_POINT ( 'NONE',  ( -111.2384876779529321, -282.8568795459104876, -265.3749094065218515 ) ) ;
#73694 = EDGE_CURVE ( 'NONE', #39232, #49322, #34744, .T. ) ;
#73696 = CARTESIAN_POINT ( 'NONE',  ( 36.99215484285436872, -285.5693247642517463, -265.5168886629330700 ) ) ;
#73695 = CARTESIAN_POINT ( 'NONE',  ( -42.99615841849104214, -281.6995004537365617, -343.7832790167157100 ) ) ;
#73697 = CARTESIAN_POINT ( 'NONE',  ( -37.02191670866836404, -281.2613224832580272, -196.9647403827163998 ) ) ;
#73698 = DIRECTION ( 'NONE',  ( 0.6421047760857910847, 0.000000000000000000, 0.7666168903225496489 ) ) ;
#73699 = CARTESIAN_POINT ( 'NONE',  ( -58.28662483653853599, -281.7181827838107324, -343.6809779964736435 ) ) ;
#73700 = CARTESIAN_POINT ( 'NONE',  ( 35.83823662742457117, -295.7639170356713407, -286.8416407754301645 ) ) ;
#73701 = CARTESIAN_POINT ( 'NONE',  ( -100.6669930418708674, -278.7022781458733220, -306.9839892094036600 ) ) ;
#73702 = CARTESIAN_POINT ( 'NONE',  ( -84.38579946574607504, -287.4065314940246481, -211.7361988700553468 ) ) ;
#73703 = CARTESIAN_POINT ( 'NONE',  ( -39.20123149955971797, -293.9491682775845902, -194.8112079111448338 ) ) ;
#73704 = CARTESIAN_POINT ( 'NONE',  ( 37.08768832890161349, -273.6758569551037681, -280.0081805225850076 ) ) ;
#73705 = CARTESIAN_POINT ( 'NONE',  ( -9.631121957500443642, -287.8963223875177277, -342.0289816169834580 ) ) ;
#73706 = CARTESIAN_POINT ( 'NONE',  ( 35.50688522963516647, -291.7968554212936283, -258.4699331130584028 ) ) ;
#73707 = CARTESIAN_POINT ( 'NONE',  ( -48.18343439339133027, -268.0651010539349386, -439.6569430058891044 ) ) ;
#73708 = CARTESIAN_POINT ( 'NONE',  ( -110.6616344576441691, -277.1617631064543730, -276.1008324570767059 ) ) ;
#73709 = CARTESIAN_POINT ( 'NONE',  ( -107.1568040914610549, -294.3594249170555486, -295.7456499766643105 ) ) ;
#73710 = CARTESIAN_POINT ( 'NONE',  ( -73.77498017898039961, -290.8618641948971799, -334.2024188173149355 ) ) ;
#73711 = DIRECTION ( 'NONE',  ( -0.8043439146810466012, -0.5941640067486159138, 0.000000000000000000 ) ) ;
#73712 = FACE_OUTER_BOUND ( 'NONE', #75473, .T. ) ;
#73713 = CARTESIAN_POINT ( 'NONE',  ( 38.75113981520446060, -291.9599899316522738, -264.6525752021095172 ) ) ;
#73714 = CARTESIAN_POINT ( 'NONE',  ( 5.169741830558485240, -288.2375378929597218, -209.9726644693475350 ) ) ;
#73715 = CARTESIAN_POINT ( 'NONE',  ( -113.3545673421658648, -288.8173870666251446, -268.3587500776523029 ) ) ;
#73716 = CARTESIAN_POINT ( 'NONE',  ( 28.17452688350138601, -288.5244254239260613, -236.7376439021539056 ) ) ;
#73717 = DIRECTION ( 'NONE',  ( -1.000000000000000000, -0.000000000000000000, -0.000000000000000000 ) ) ;
#73718 = CARTESIAN_POINT ( 'NONE',  ( 34.72465733445011438, -288.1852340720965913, -257.4643935687864769 ) ) ;
#73719 = CARTESIAN_POINT ( 'NONE',  ( -2.700661915091799870, -296.5762869281131202, -337.2820061819716670 ) ) ;
#73720 = DIRECTION ( 'NONE',  ( 0.000000000000000000, 0.000000000000000000, 1.000000000000000000 ) ) ;
#73721 = CARTESIAN_POINT ( 'NONE',  ( -4.489367707384485762, -289.8339165161353321, -339.5761962308149009 ) ) ;
#73722 = CARTESIAN_POINT ( 'NONE',  ( -97.25298841204069333, -277.1951343289675265, -224.6340422650594348 ) ) ;
#73723 = CARTESIAN_POINT ( 'NONE',  ( -113.2163645477496061, -279.0479534217701030, -257.3695980268642529 ) ) ;
#73724 = CARTESIAN_POINT ( 'NONE',  ( -72.49337008041595709, -279.2664867021431405, -201.8621341704333929 ) ) ;
#73725 = CARTESIAN_POINT ( 'NONE',  ( -63.22995514473932133, -283.7149093591689279, -199.9154083422040458 ) ) ;
#73726 = DIRECTION ( 'NONE',  ( -1.000000000000000000, -0.000000000000000000, -0.000000000000000000 ) ) ;
#73727 = CARTESIAN_POINT ( 'NONE',  ( -11.28780985351950861, -278.5347071759974256, -200.7937257455134556 ) ) ;
#73728 = CARTESIAN_POINT ( 'NONE',  ( -73.33904704047141365, -281.5290120307544157, -336.2156664521891116 ) ) ;
#73729 = CARTESIAN_POINT ( 'NONE',  ( -104.9195950068973247, -260.6502555361738018, -315.6180979797861141 ) ) ;
#73730 = CARTESIAN_POINT ( 'NONE',  ( -95.63219835742853547, -276.3624001833008492, -319.6248253433047921 ) ) ;
#73731 = CARTESIAN_POINT ( 'NONE',  ( -65.85872123725167171, -299.1922791858725645, -202.4090226470799792 ) ) ;
#73732 = CARTESIAN_POINT ( 'NONE',  ( -83.70730369116959935, -282.5917432765307922, -331.5156693667757963 ) ) ;
#73733 = CARTESIAN_POINT ( 'NONE',  ( -109.7440779004766256, -273.4979115589378011, -259.5027959293468030 ) ) ;
#73734 = CARTESIAN_POINT ( 'NONE',  ( -91.76224254228044686, -274.7198147158087522, -216.7233434610150482 ) ) ;
#73735 = CARTESIAN_POINT ( 'NONE',  ( 29.10704942818989593, -274.8093255014956640, -239.9625370447037938 ) ) ;
#73736 = CARTESIAN_POINT ( 'NONE',  ( -17.67210618421144019, -296.7985928854120630, -342.7358906590718561 ) ) ;
#73737 = CARTESIAN_POINT ( 'NONE',  ( -103.7973530481297075, -290.2114433359136001, -309.3593278020074990 ) ) ;
#73738 = CARTESIAN_POINT ( 'NONE',  ( -64.20703467292696587, -277.7843467449993682, -199.6832325289846892 ) ) ;
#73739 = CARTESIAN_POINT ( 'NONE',  ( -111.5425395019756252, -290.1277284527902793, -290.9338047475022222 ) ) ;
#73740 = CARTESIAN_POINT ( 'NONE',  ( -97.54915770768187144, -289.0315988377550411, -312.0781245275720721 ) ) ;
#73741 = CARTESIAN_POINT ( 'NONE',  ( 17.95866809632716254, -290.8443932923930788, -219.6968315096645483 ) ) ;
#73742 = ORIENTED_EDGE ( 'NONE', *, *, #45806, .F. ) ;
#73743 = CARTESIAN_POINT ( 'NONE',  ( 199.5543596254793499, 67.40697023589044079, 8.432225012702247113 ) ) ;
#73744 = CARTESIAN_POINT ( 'NONE',  ( -105.7660700396458822, -290.4029477440144547, -244.6032623194039672 ) ) ;
#73745 = DIRECTION ( 'NONE',  ( -0.000000000000000000, 1.000000000000000000, -0.000000000000000000 ) ) ;
#73746 = CARTESIAN_POINT ( 'NONE',  ( -52.13970387330772382, -286.8085524760460316, -194.9820007753183120 ) ) ;
#73747 = CARTESIAN_POINT ( 'NONE',  ( 30.91033621190086578, -290.2662352645559167, -285.9065529553535612 ) ) ;
#73748 = CARTESIAN_POINT ( 'NONE',  ( -66.84512178793866610, -294.4881553351906973, -341.2439469251428932 ) ) ;
#73749 = CARTESIAN_POINT ( 'NONE',  ( 36.01070059573344651, -283.1439305523996381, -292.2857158972446996 ) ) ;
#73750 = CARTESIAN_POINT ( 'NONE',  ( -49.41943863945510174, -285.7273382127859804, -198.3156738816327902 ) ) ;
#73751 = CARTESIAN_POINT ( 'NONE',  ( 34.65100332138116812, -277.0609250344158454, -285.1358981638676937 ) ) ;
#73752 = CARTESIAN_POINT ( 'NONE',  ( -37.52933173917555365, -290.0699379404213119, -195.7038249997779644 ) ) ;
#73753 = CARTESIAN_POINT ( 'NONE',  ( -54.28840429534911038, -272.6245083723702010, -198.9472557324415050 ) ) ;
#73754 = ORIENTED_EDGE ( 'NONE', *, *, #82664, .T. ) ;
#73755 = DIRECTION ( 'NONE',  ( -1.000000000000000000, -0.000000000000000000, -0.000000000000000000 ) ) ;
#73756 = CARTESIAN_POINT ( 'NONE',  ( 25.69489922945507843, -293.8035364451362170, -314.5670523385749107 ) ) ;
#73757 = CARTESIAN_POINT ( 'NONE',  ( -73.08654553314303826, -287.4947045784555826, -205.0502160175830682 ) ) ;
#73758 = CARTESIAN_POINT ( 'NONE',  ( -106.8802828879418172, -297.2162379984434892, -302.7011553453286865 ) ) ;
#73759 = CARTESIAN_POINT ( 'NONE',  ( 26.45228736770980049, -287.7147263547475404, -234.5613535756960459 ) ) ;
#73760 = CARTESIAN_POINT ( 'NONE',  ( -111.1078145051525894, -277.8780976944817667, -249.1153988151750127 ) ) ;
#73761 = CARTESIAN_POINT ( 'NONE',  ( -33.55269532271341859, -292.7500827522039231, -193.5564551725889260 ) ) ;
#73762 = CARTESIAN_POINT ( 'NONE',  ( 36.61397865747861147, -285.9016788278399304, -286.8781827619521323 ) ) ;
#73763 = CARTESIAN_POINT ( 'NONE',  ( -24.90704448006370697, -295.2311137609514162, -346.3830811067127797 ) ) ;
#73764 = CARTESIAN_POINT ( 'NONE',  ( -55.02158141227934607, -292.1517460690146208, -199.5126226953891830 ) ) ;
#73765 = CARTESIAN_POINT ( 'NONE',  ( 2.197429475817664013, -229.5268262511776527, 22.47499999999998721 ) ) ;
#73766 = FACE_OUTER_BOUND ( 'NONE', #70957, .T. ) ;
#73767 = CARTESIAN_POINT ( 'NONE',  ( -101.6167628974910002, -254.6067659492929351, -324.2419241925472875 ) ) ;
#73768 = CARTESIAN_POINT ( 'NONE',  ( 29.51467527819651337, -288.5903127428882158, -233.4692965923466659 ) ) ;
#73769 = CARTESIAN_POINT ( 'NONE',  ( -2.659677404128736544, -280.1237833571632336, -342.4524372437778652 ) ) ;
#73770 = ORIENTED_EDGE ( 'NONE', *, *, #48476, .T. ) ;
#73771 = CARTESIAN_POINT ( 'NONE',  ( -103.2967528793522263, -283.0396799742412099, -302.4802008733856269 ) ) ;
#73772 = CARTESIAN_POINT ( 'NONE',  ( 22.78724498022210909, -282.9427202189310151, -225.7914021569596628 ) ) ;
#73773 = CARTESIAN_POINT ( 'NONE',  ( -101.6854563161719227, -256.6257814484651476, -325.9156231221182338 ) ) ;
#73774 = CARTESIAN_POINT ( 'NONE',  ( -100.9388859079359406, -282.5640546632850487, -312.8117763095281703 ) ) ;
#73775 = CARTESIAN_POINT ( 'NONE',  ( -11.42785105332955098, -284.4115164783612499, -200.3588378163500181 ) ) ;
#73776 = CARTESIAN_POINT ( 'NONE',  ( -8.188134955983059626, -276.2901658752921321, -200.3742206346934154 ) ) ;
#73777 = CARTESIAN_POINT ( 'NONE',  ( -95.34174379319205173, -297.6692346955820199, -225.9111981844087040 ) ) ;
#73778 = CARTESIAN_POINT ( 'NONE',  ( 20.90386569182295418, -292.8637558888753460, -315.2002126159817976 ) ) ;
#73779 = CARTESIAN_POINT ( 'NONE',  ( -112.6194715577560146, -279.4009956492743640, -254.5950386476127392 ) ) ;
#73780 = CARTESIAN_POINT ( 'NONE',  ( 16.53115478250300896, -276.2589932042342298, -319.6414663191355885 ) ) ;
#73781 = CARTESIAN_POINT ( 'NONE',  ( 19.16138736105685325, -299.6846001230114211, -193.5876150138238074 ) ) ;
#73782 = CARTESIAN_POINT ( 'NONE',  ( -17.45137186351961489, -275.7216532141115408, -344.4277592622011639 ) ) ;
#73783 = CARTESIAN_POINT ( 'NONE',  ( -114.0438014765299215, -273.4268578961535354, -284.1485094271325806 ) ) ;
#73784 = CARTESIAN_POINT ( 'NONE',  ( 35.38724277842326416, -273.3161052442963523, -251.9927585438613278 ) ) ;
#73785 = CARTESIAN_POINT ( 'NONE',  ( -70.53536832136332180, -296.9064252494713969, -339.1998332857435230 ) ) ;
#73786 = DIRECTION ( 'NONE',  ( -1.000000000000000000, -0.000000000000000000, -0.000000000000000000 ) ) ;
#73787 = DIRECTION ( 'NONE',  ( 1.000000000000000000, 0.000000000000000000, 0.000000000000000000 ) ) ;
#73788 = CARTESIAN_POINT ( 'NONE',  ( -64.15568773085546184, -284.4900749232543262, -338.5904089261549643 ) ) ;
#73789 = CARTESIAN_POINT ( 'NONE',  ( -91.69306513445995677, -285.5740807330581106, -323.4638781271057155 ) ) ;
#73790 = CARTESIAN_POINT ( 'NONE',  ( -22.43094972540467325, -285.5965859655285612, -198.7440730104717659 ) ) ;
#73791 = CARTESIAN_POINT ( 'NONE',  ( -107.8873185852755370, -276.6660275418012134, -292.2062575061756888 ) ) ;
#73792 = CARTESIAN_POINT ( 'NONE',  ( -106.7277233849747375, -286.7590490024441578, -243.9708687387712587 ) ) ;
#73793 = CARTESIAN_POINT ( 'NONE',  ( -22.03164190960058377, -278.7315944653297493, -198.2233311138994907 ) ) ;
#73794 = EDGE_CURVE ( 'NONE', #22798, #90280, #90938, .T. ) ;
#73795 = CARTESIAN_POINT ( 'NONE',  ( 25.64816641636719652, -277.1452475668247075, -307.8644883084474486 ) ) ;
#73796 = EDGE_CURVE ( 'NONE', #68989, #14859, #17309, .T. ) ;
#73797 = CYLINDRICAL_SURFACE ( 'NONE', #12573, 9.103929867429224387 ) ;
#73798 = CARTESIAN_POINT ( 'NONE',  ( -90.24548739326772306, -273.7707272385108581, -219.9525582034610807 ) ) ;
#73799 = CARTESIAN_POINT ( 'NONE',  ( 35.45939109536712408, -282.6670921712283189, -295.1062011347452767 ) ) ;
#73800 = CARTESIAN_POINT ( 'NONE',  ( -38.72514932449956149, -283.5614130177448828, -347.2871407044924013 ) ) ;
#73801 = ORIENTED_EDGE ( 'NONE', *, *, #6032, .T. ) ;
#73802 = ORIENTED_EDGE ( 'NONE', *, *, #46714, .T. ) ;
#73803 = CARTESIAN_POINT ( 'NONE',  ( 196.6739207415263593, 42.33397377253083960, 12.85244989408970184 ) ) ;
#73804 = CARTESIAN_POINT ( 'NONE',  ( 19.34654445579052862, -288.7197857380605797, -220.0169296502561167 ) ) ;
#73805 = CARTESIAN_POINT ( 'NONE',  ( -109.4332341122041754, -295.9134067552732290, -257.8946647959382972 ) ) ;
#73806 = CARTESIAN_POINT ( 'NONE',  ( -0.8449143339587453783, -291.8724508696616908, -202.6758358785880034 ) ) ;
#73807 = CARTESIAN_POINT ( 'NONE',  ( -13.07767898527680295, -287.2109539346897691, -339.9453477319760282 ) ) ;
#73808 = CARTESIAN_POINT ( 'NONE',  ( -18.33870979613791619, -287.3773197666213832, -341.5074526759464675 ) ) ;
#73809 = AXIS2_PLACEMENT_3D ( 'NONE', #91895, #5294, #32754 ) ;
#73810 = CARTESIAN_POINT ( 'NONE',  ( 16.25398396665944745, -288.0395014047340396, -220.1964574321729629 ) ) ;
#73811 = CARTESIAN_POINT ( 'NONE',  ( -112.0492067503147382, -276.6442006755905823, -263.1794260992977001 ) ) ;
#73812 = CARTESIAN_POINT ( 'NONE',  ( -45.95578702752110445, -287.5593842692071576, -346.1252375044198288 ) ) ;
#73813 = CARTESIAN_POINT ( 'NONE',  ( 14.88766819689077003, -288.7885883979220694, -216.5364607004050868 ) ) ;
#73814 = CARTESIAN_POINT ( 'NONE',  ( -29.20164869531769369, -286.9492078427433057, -345.1379825956768173 ) ) ;
#73815 = CARTESIAN_POINT ( 'NONE',  ( -26.69676767428009967, -283.8548206379275030, -342.8701154712414905 ) ) ;
#73816 = CARTESIAN_POINT ( 'NONE',  ( -95.18478502880068959, -293.2136646698784830, -222.3390730214786117 ) ) ;
#73817 = CARTESIAN_POINT ( 'NONE',  ( 82.14122032850023913, -300.1543061692601668, -193.4499960878401623 ) ) ;
#73818 = CARTESIAN_POINT ( 'NONE',  ( 210.3152560301384142, 38.32590481451376263, 10.50000000000000000 ) ) ;
#73819 = CARTESIAN_POINT ( 'NONE',  ( -111.7808693500708159, -298.3032906383199929, -283.6225164144282189 ) ) ;
#73820 = CARTESIAN_POINT ( 'NONE',  ( -14.24823353745979482, -279.5564611225354952, -200.8864260453578652 ) ) ;
#73821 = CARTESIAN_POINT ( 'NONE',  ( 37.12240448217178113, -279.6723202601086768, -279.7327463155705800 ) ) ;
#73822 = CARTESIAN_POINT ( 'NONE',  ( -41.94612645753468172, -294.3058208084767102, -347.1138451097400548 ) ) ;
#73823 = CARTESIAN_POINT ( 'NONE',  ( -110.5822304238010503, -270.9353513147710828, -259.3439437264424328 ) ) ;
#73824 = CARTESIAN_POINT ( 'NONE',  ( -35.09826129485670521, -275.1036056119682485, -344.7673084690574115 ) ) ;
#73825 = CARTESIAN_POINT ( 'NONE',  ( -26.11566802437828017, -296.2214099567489711, -342.9918255394018729 ) ) ;
#73826 = CARTESIAN_POINT ( 'NONE',  ( 154.0331653244526819, 19.37068896744924018, 11.96806464917981216 ) ) ;
#73827 = CARTESIAN_POINT ( 'NONE',  ( -67.28786665653916543, -272.2417987862393716, -200.0629430128183799 ) ) ;
#73828 = CARTESIAN_POINT ( 'NONE',  ( -83.58649898465269246, -293.9161297838734299, -330.7216908243435682 ) ) ;
#73829 = CARTESIAN_POINT ( 'NONE',  ( 28.93305158235684615, -295.4081990845666610, -302.4635687803697124 ) ) ;
#73830 = CARTESIAN_POINT ( 'NONE',  ( -4.254505052825189537, -295.4072536823830433, -335.6272686060038950 ) ) ;
#73831 = FACE_OUTER_BOUND ( 'NONE', #55142, .T. ) ;
#73833 = CARTESIAN_POINT ( 'NONE',  ( -98.73330315598403217, -296.0044225332788415, -309.9514553950112372 ) ) ;
#73832 = CARTESIAN_POINT ( 'NONE',  ( -37.94346067913136267, -284.0647605629362147, -195.0083164981553523 ) ) ;
#73834 = CARTESIAN_POINT ( 'NONE',  ( -112.3597286615845974, -284.7692380986950980, -253.0032553564617785 ) ) ;
#73835 = CARTESIAN_POINT ( 'NONE',  ( 33.96054671114661971, -283.1490896012176677, -245.1989188759397393 ) ) ;
#73836 = CARTESIAN_POINT ( 'NONE',  ( -102.4983191144708741, -284.7558070208886534, -229.3689322181430441 ) ) ;
#73837 = CARTESIAN_POINT ( 'NONE',  ( -111.0789092493111099, -288.7200106634448957, -257.3044641378569395 ) ) ;
#73838 = CARTESIAN_POINT ( 'NONE',  ( -4.771743288812454686, -271.9809262143061233, -202.8022627189028810 ) ) ;
#73839 = CARTESIAN_POINT ( 'NONE',  ( -72.59595684809394811, -284.2598991290782919, -205.8612979581295690 ) ) ;
#73840 = CARTESIAN_POINT ( 'NONE',  ( -112.2663082739289564, -289.2670012222915830, -286.7255796422575145 ) ) ;
#73841 = CARTESIAN_POINT ( 'NONE',  ( 164.2231345125756263, 264.6571197653884155, 7.500000000000000000 ) ) ;
#73842 = CARTESIAN_POINT ( 'NONE',  ( -111.5982237241403823, -279.7496748086906564, -288.4318337455994197 ) ) ;
#73844 = CARTESIAN_POINT ( 'NONE',  ( 19.69519086606120695, -280.5749137806306521, -224.7663753842709866 ) ) ;
#73843 = CARTESIAN_POINT ( 'NONE',  ( -19.69740637617231016, -292.8466233125772078, -343.6752236016824895 ) ) ;
#73845 = CARTESIAN_POINT ( 'NONE',  ( -47.62947259828213475, -295.3461899170790730, -346.6707618167072837 ) ) ;
#73846 = CARTESIAN_POINT ( 'NONE',  ( -84.59301588795722182, -283.4868478609280942, -211.3981859481368701 ) ) ;
#73847 = CARTESIAN_POINT ( 'NONE',  ( -89.68118424490572238, -281.3146599581779697, -216.5711059396477651 ) ) ;
#73848 = CARTESIAN_POINT ( 'NONE',  ( -69.83922304417063742, -294.5497814741926277, -335.9912898032399085 ) ) ;
#73849 = CARTESIAN_POINT ( 'NONE',  ( -86.81020433254104773, -271.3662507241008939, -213.6978074929134834 ) ) ;
#73850 = VERTEX_POINT ( 'NONE', #22460 ) ;
#73851 = CARTESIAN_POINT ( 'NONE',  ( 175.2296996224750103, 128.0000000000000568, 0.000000000000000000 ) ) ;
#73852 = CARTESIAN_POINT ( 'NONE',  ( 26.98908576708132401, -284.0417792222714297, -308.3235406939451195 ) ) ;
#73853 = CARTESIAN_POINT ( 'NONE',  ( -39.69729818416332989, -294.5901478204166324, -343.3971139300035702 ) ) ;
#73854 = DIRECTION ( 'NONE',  ( -0.000000000000000000, -0.000000000000000000, 1.000000000000000000 ) ) ;
#73855 = CARTESIAN_POINT ( 'NONE',  ( -95.99890600148557951, -275.4094976428775681, -317.0979686699210447 ) ) ;
#73856 = CARTESIAN_POINT ( 'NONE',  ( -38.34502749961526291, -273.2370464740843659, -193.5291444596736028 ) ) ;
#73857 = CARTESIAN_POINT ( 'NONE',  ( -103.5554268108481324, -290.8003721497686911, -239.6244557814866027 ) ) ;
#73858 = CARTESIAN_POINT ( 'NONE',  ( -96.17687782110718331, -280.6899571714385502, -225.9652891420465153 ) ) ;
#73859 = CARTESIAN_POINT ( 'NONE',  ( -95.25302026304424885, -274.7907954267257082, -224.6148676669409667 ) ) ;
#73860 = CARTESIAN_POINT ( 'NONE',  ( -1.987035912855077413, -284.1919728182602398, -337.8628819255183089 ) ) ;
#73861 = CARTESIAN_POINT ( 'NONE',  ( -19.42284112748631131, -279.0826062357957085, -199.1323857647484203 ) ) ;
#73862 = CARTESIAN_POINT ( 'NONE',  ( 22.44627944024040644, -278.1716316236181683, -315.6424403049408625 ) ) ;
#73863 = ORIENTED_EDGE ( 'NONE', *, *, #2023, .F. ) ;
#73864 = CARTESIAN_POINT ( 'NONE',  ( -88.03477456345915186, -273.1994360773490484, -212.3315192770881197 ) ) ;
#73865 = CARTESIAN_POINT ( 'NONE',  ( -27.94840955108134750, -294.0923447998343931, -196.4643949375640659 ) ) ;
#73866 = DIRECTION ( 'NONE',  ( -1.000000000000000000, -0.000000000000000000, 0.000000000000000000 ) ) ;
#73867 = CARTESIAN_POINT ( 'NONE',  ( 221.8344101925596306, 1.000000000000000222, -7.000000000000000888 ) ) ;
#73868 = CARTESIAN_POINT ( 'NONE',  ( -39.10325494934452450, -293.2136277450637181, -346.1054405960279610 ) ) ;
#73869 = AXIS2_PLACEMENT_3D ( 'NONE', #57085, #233, #28654 ) ;
#73870 = CARTESIAN_POINT ( 'NONE',  ( -55.29475553308035529, -297.4816189100373549, -199.5290269991330945 ) ) ;
#73871 = CARTESIAN_POINT ( 'NONE',  ( 154.9842916688209868, 128.0000000000000568, -12.88888888888889461 ) ) ;
#73872 = CARTESIAN_POINT ( 'NONE',  ( -7.479538313361029367, -293.9567322257258866, -200.1261392262484264 ) ) ;
#73873 = CARTESIAN_POINT ( 'NONE',  ( 108.5619616845123971, -302.2645883696979467, -190.3030568020281805 ) ) ;
#73874 = CARTESIAN_POINT ( 'NONE',  ( -6.278151174005602186, -288.4613230929442125, -202.2655952638983194 ) ) ;
#73875 = CARTESIAN_POINT ( 'NONE',  ( -41.99542039640643054, -275.1107534586386123, -345.0625258940852405 ) ) ;
#73876 = CARTESIAN_POINT ( 'NONE',  ( 37.04214408809731651, -277.5241241732517210, -274.3661998222550551 ) ) ;
#73877 = CARTESIAN_POINT ( 'NONE',  ( 11.21264757630517295, -292.4531601628782482, -326.7861967517209791 ) ) ;
#73878 = CARTESIAN_POINT ( 'NONE',  ( -66.90272753528901717, -281.5292724995988465, -200.6011642793420719 ) ) ;
#73879 = ORIENTED_EDGE ( 'NONE', *, *, #77244, .F. ) ;
#73880 = CARTESIAN_POINT ( 'NONE',  ( -64.06706087006881489, -283.0773503888726736, -338.3158277531293834 ) ) ;
#73881 = CARTESIAN_POINT ( 'NONE',  ( -75.17170661637928220, -278.6237813932754079, -337.0723098398895559 ) ) ;
#73882 = CARTESIAN_POINT ( 'NONE',  ( -1.831900275020204472, -281.3872222048400431, -338.2364657459490900 ) ) ;
#73883 = CARTESIAN_POINT ( 'NONE',  ( -34.28841866488321699, -277.9558883237970690, -347.0650793260665523 ) ) ;
#73884 = EDGE_CURVE ( 'NONE', #31000, #16833, #51334, .T. ) ;
#73885 = CARTESIAN_POINT ( 'NONE',  ( 23.82360943416126986, -277.6846734358366007, -315.9847156104772807 ) ) ;
#73886 = CARTESIAN_POINT ( 'NONE',  ( -6.998514795304313196, -294.9805209788416391, -207.2794874003663779 ) ) ;
#73887 = ORIENTED_EDGE ( 'NONE', *, *, #3993, .T. ) ;
#73888 = CARTESIAN_POINT ( 'NONE',  ( -106.6190931217805087, -298.9273471183138895, -241.6271056257840257 ) ) ;
#73889 = CARTESIAN_POINT ( 'NONE',  ( -88.15471438379844926, -292.4004734663049021, -217.4490762572561096 ) ) ;
#73890 = CARTESIAN_POINT ( 'NONE',  ( -41.98350225846543538, -275.1310184801379819, -344.8743369305223041 ) ) ;
#73891 = CARTESIAN_POINT ( 'NONE',  ( -92.83719101655950112, -291.5942743863346891, -322.3428438578150690 ) ) ;
#73892 = CARTESIAN_POINT ( 'NONE',  ( -92.62815983957735000, -290.5812807393708681, -222.5353922588550688 ) ) ;
#73893 = CARTESIAN_POINT ( 'NONE',  ( 20.52247575971392735, -287.7465773972697320, -321.0885967068805371 ) ) ;
#73894 = CARTESIAN_POINT ( 'NONE',  ( 164.7123623445222904, 3.000000000000000000, 10.00000000000000178 ) ) ;
#73895 = CARTESIAN_POINT ( 'NONE',  ( -109.1391143042689436, -283.1754909391347610, -253.2312859296519889 ) ) ;
#73896 = CARTESIAN_POINT ( 'NONE',  ( -69.26809409742949697, -291.3371681885150792, -337.3803006998751925 ) ) ;
#73897 = CARTESIAN_POINT ( 'NONE',  ( -79.69205875168110254, -283.9483635898707234, -209.9896532683062560 ) ) ;
#73898 = EDGE_CURVE ( 'NONE', #77341, #25970, #71052, .T. ) ;
#73899 = CARTESIAN_POINT ( 'NONE',  ( 21.71533229932875386, -282.2578444688995205, -226.5962534668126978 ) ) ;
#73900 = CARTESIAN_POINT ( 'NONE',  ( -51.62972456036622759, -290.1718923654533455, -345.7844072912005799 ) ) ;
#73901 = CARTESIAN_POINT ( 'NONE',  ( -69.77325112503888249, -280.1055240545388187, -204.8783137650117396 ) ) ;
#73902 = CARTESIAN_POINT ( 'NONE',  ( -64.23495259808915137, -290.5039918610806353, -198.5782455056484821 ) ) ;
#73903 = CARTESIAN_POINT ( 'NONE',  ( 9.703807935584841005, -287.4840925372035940, -209.6085131739653775 ) ) ;
#73904 = CARTESIAN_POINT ( 'NONE',  ( 30.07461289773250712, -287.5627034143271317, -233.1754279496403797 ) ) ;
#73905 = CARTESIAN_POINT ( 'NONE',  ( -35.93559594995342366, -286.2369562790522650, -197.3746611869852927 ) ) ;
#73906 = EDGE_LOOP ( 'NONE', ( #77019, #49772, #55852 ) ) ;
#73907 = CARTESIAN_POINT ( 'NONE',  ( 194.7211398848818362, 27.16984437419170462, 14.02118807791477018 ) ) ;
#73908 = CARTESIAN_POINT ( 'NONE',  ( 23.80336376861723835, -294.8088618346456542, -225.6220227360954027 ) ) ;
#73909 = CARTESIAN_POINT ( 'NONE',  ( -101.2257768192920082, -294.6788166068431565, -312.5535512445609925 ) ) ;
#73910 = CARTESIAN_POINT ( 'NONE',  ( -6.187383634769226148, -275.6911965959109239, -336.6532594284458924 ) ) ;
#73911 = CARTESIAN_POINT ( 'NONE',  ( -35.82231046780808725, -297.4192976348145407, -193.4632129206172237 ) ) ;
#73912 = CARTESIAN_POINT ( 'NONE',  ( 23.92835671900255790, -291.4687502070530059, -229.4137384997679590 ) ) ;
#73913 = CARTESIAN_POINT ( 'NONE',  ( -101.0499860729498778, -294.2802809457257354, -308.1347300222603280 ) ) ;
#73914 = CARTESIAN_POINT ( 'NONE',  ( -98.63956921055091698, -292.3151546047912461, -229.8992058195396453 ) ) ;
#73915 = CARTESIAN_POINT ( 'NONE',  ( 19.57713208129874971, -293.9806969196148430, -224.1409160332540864 ) ) ;
#73916 = FACE_OUTER_BOUND ( 'NONE', #66764, .T. ) ;
#73917 = CARTESIAN_POINT ( 'NONE',  ( 26.53421145933675263, -292.0839678369325725, -310.0807717358518971 ) ) ;
#73918 = CARTESIAN_POINT ( 'NONE',  ( -71.72753629290552624, -299.5979734891082558, -203.6939506260904409 ) ) ;
#73919 = CARTESIAN_POINT ( 'NONE',  ( -56.11437692538834199, -290.2410734688080538, -341.2022243196234399 ) ) ;
#73920 = CARTESIAN_POINT ( 'NONE',  ( -53.74804602735255799, -279.2414416841962748, -343.9621137417991008 ) ) ;
#73921 = CARTESIAN_POINT ( 'NONE',  ( -110.0755937367490418, -277.5393388361014217, -246.4638037918190605 ) ) ;
#73922 = CARTESIAN_POINT ( 'NONE',  ( -18.56681917932296599, -273.6362941101798469, -195.7352761255145026 ) ) ;
#73923 = CARTESIAN_POINT ( 'NONE',  ( 33.59625934825948690, -279.9273388536918219, -293.0925086881986772 ) ) ;
#73924 = CARTESIAN_POINT ( 'NONE',  ( -64.43859120765851856, -278.1043208008236434, -199.0861079120081740 ) ) ;
#73925 = CARTESIAN_POINT ( 'NONE',  ( -107.9283820667177736, -295.5058280006942937, -249.8973985858545745 ) ) ;
#73926 = CARTESIAN_POINT ( 'NONE',  ( 157.7238125175282448, 18.72892514816167164, 11.10081581328679867 ) ) ;
#73927 = CARTESIAN_POINT ( 'NONE',  ( -21.92060251988330677, -274.9064447384953951, -198.9042609540987314 ) ) ;
#73928 = CIRCLE ( 'NONE', #33110, 1.000000000000000888 ) ;
#73929 = CARTESIAN_POINT ( 'NONE',  ( 194.2991783531507508, 27.07972378075054465, 14.57245942894549096 ) ) ;
#73930 = CARTESIAN_POINT ( 'NONE',  ( -112.3666653663188839, -288.6691802253907895, -262.7768855651746094 ) ) ;
#73931 = CARTESIAN_POINT ( 'NONE',  ( -105.1559689240054212, -290.0805981575247188, -306.8333669901844019 ) ) ;
#73932 = CARTESIAN_POINT ( 'NONE',  ( -11.01419554982314075, -276.3945657467878618, -199.9005619880542781 ) ) ;
#73933 = CARTESIAN_POINT ( 'NONE',  ( -89.38284643684882269, -295.3175821860816654, -216.5138247584088731 ) ) ;
#73934 = EDGE_CURVE ( 'NONE', #47807, #17649, #60330, .T. ) ;
#73935 = CARTESIAN_POINT ( 'NONE',  ( -13.48180273340718571, -281.9471979166174265, -343.4012721203852720 ) ) ;
#73936 = DIRECTION ( 'NONE',  ( 0.000000000000000000, 0.000000000000000000, 1.000000000000000000 ) ) ;
#73937 = CARTESIAN_POINT ( 'NONE',  ( 2.706147341885323243, -280.5152443130122606, -333.8344045608845931 ) ) ;
#73938 = CARTESIAN_POINT ( 'NONE',  ( 201.0876323342543515, 25.81167821795959938, 10.49999999999999822 ) ) ;
#73939 = CARTESIAN_POINT ( 'NONE',  ( -14.70946362963264065, -291.1470087163989433, -200.5405452603425260 ) ) ;
#73940 = CARTESIAN_POINT ( 'NONE',  ( -90.53162389273815336, -283.4288544204246705, -218.5022676429446449 ) ) ;
#73941 = FACE_OUTER_BOUND ( 'NONE', #73095, .T. ) ;
#73942 = CARTESIAN_POINT ( 'NONE',  ( 221.8344101925596021, 1.000000000000000222, -8.171572875253810153 ) ) ;
#73943 = CARTESIAN_POINT ( 'NONE',  ( 0.9515220733797971064, -290.5630023235333397, -205.8736790340005882 ) ) ;
#73944 = CARTESIAN_POINT ( 'NONE',  ( -110.6968746167573983, -280.0408341145362670, -278.9024217866071353 ) ) ;
#73945 = CARTESIAN_POINT ( 'NONE',  ( -101.0801813714010819, -285.1939784076167257, -312.9464394515257482 ) ) ;
#73947 = CARTESIAN_POINT ( 'NONE',  ( -67.54769721631765833, -285.6444702736058616, -203.9036297671191846 ) ) ;
#73946 = CARTESIAN_POINT ( 'NONE',  ( -31.34941537011497203, -272.2070926714131929, -195.0260647574129962 ) ) ;
#73948 = CARTESIAN_POINT ( 'NONE',  ( -4.789228989113279766, -278.0401137696960063, -336.3729365570699201 ) ) ;
#73949 = CARTESIAN_POINT ( 'NONE',  ( 5.499601202870486816, -277.2584797257404716, -329.7298779904547246 ) ) ;
#73950 = CARTESIAN_POINT ( 'NONE',  ( -111.6150036585392087, -286.4138848813902314, -281.1422890198280129 ) ) ;
#73951 = ORIENTED_EDGE ( 'NONE', *, *, #30285, .F. ) ;
#73952 = CARTESIAN_POINT ( 'NONE',  ( 154.1407330040854333, 128.0000000000000568, 13.42592592592592737 ) ) ;
#73953 = CARTESIAN_POINT ( 'NONE',  ( -77.08404761448591103, -295.4021818777276849, -336.3742362034354869 ) ) ;
#73954 = CARTESIAN_POINT ( 'NONE',  ( 29.11119913181458685, -289.0789560618642327, -236.2493032309313321 ) ) ;
#73955 = FACE_OUTER_BOUND ( 'NONE', #5072, .T. ) ;
#73956 = CARTESIAN_POINT ( 'NONE',  ( -55.63300648810263738, -292.7666405000204577, -350.3538533559490702 ) ) ;
#73957 = CARTESIAN_POINT ( 'NONE',  ( -68.53415931668918404, -278.5721433217157141, -200.2859392594817791 ) ) ;
#73958 = CARTESIAN_POINT ( 'NONE',  ( -39.17183834611936533, -290.4294551764250514, -194.1701960755857215 ) ) ;
#73959 = EDGE_CURVE ( 'NONE', #40992, #60489, #43782, .T. ) ;
#73960 = CARTESIAN_POINT ( 'NONE',  ( -94.67354007227584134, -286.7210794403503655, -224.0402700283262050 ) ) ;
#73961 = CARTESIAN_POINT ( 'NONE',  ( -107.4112342350791067, -280.6265932114612838, -246.3659205339392599 ) ) ;
#73962 = CARTESIAN_POINT ( 'NONE',  ( 38.38885664596990921, -288.8492132832033690, -260.1881605336885741 ) ) ;
#73963 = CARTESIAN_POINT ( 'NONE',  ( 2.176196039675799554, -284.5235453667215211, -334.1660781397623055 ) ) ;
#73964 = CARTESIAN_POINT ( 'NONE',  ( 37.23927360239664353, -275.9584694388872776, -289.5099655181301159 ) ) ;
#73965 = CARTESIAN_POINT ( 'NONE',  ( -50.21330951316453195, -295.9071516055281563, -196.8344665436037246 ) ) ;
#73966 = CARTESIAN_POINT ( 'NONE',  ( -16.98994805964158417, -280.1412381099899562, -196.0993768756424060 ) ) ;
#73967 = CARTESIAN_POINT ( 'NONE',  ( -73.56864489035299925, -299.4875645629279575, -205.3309505810239841 ) ) ;
#73968 = CARTESIAN_POINT ( 'NONE',  ( 158.5846220834750397, 17.31716537717085203, 10.56280983457213907 ) ) ;
#73969 = FACE_OUTER_BOUND ( 'NONE', #43625, .T. ) ;
#73970 = CARTESIAN_POINT ( 'NONE',  ( -29.91532298040375792, -272.3847949563289603, -194.7382184377183023 ) ) ;
#73971 = LINE ( 'NONE', #38448, #53033 ) ;
#73972 = CARTESIAN_POINT ( 'NONE',  ( -95.32568175659837095, -277.4349709954749414, -314.8116108522064565 ) ) ;
#73973 = CARTESIAN_POINT ( 'NONE',  ( -2.750648921129092539, -275.7042312916930769, -201.9983547557986867 ) ) ;
#73974 = CARTESIAN_POINT ( 'NONE',  ( 31.81471935147924768, -280.1807685078698000, -236.9189749165308001 ) ) ;
#73975 = CARTESIAN_POINT ( 'NONE',  ( -20.88249082309033255, -290.5981528987918523, -342.5211376605471401 ) ) ;
#73976 = CARTESIAN_POINT ( 'NONE',  ( -113.5417001291470882, -274.1520230306431358, -270.3814460222293405 ) ) ;
#73977 = CARTESIAN_POINT ( 'NONE',  ( -36.20720205948475723, -299.2711283777799736, -193.7579611739544987 ) ) ;
#73978 = CARTESIAN_POINT ( 'NONE',  ( -68.58937396217021387, -293.6407473853936949, -202.3498941708393204 ) ) ;
#73979 = CARTESIAN_POINT ( 'NONE',  ( 11.07595942897569152, -280.3803540244982742, -327.4884985235727299 ) ) ;
#73980 = CARTESIAN_POINT ( 'NONE',  ( 36.78390087520668317, -283.3768880073544665, -262.9848089022532349 ) ) ;
#73981 = CARTESIAN_POINT ( 'NONE',  ( -82.03613388021695130, -271.4600018336710150, -210.5112076429528543 ) ) ;
#73982 = CARTESIAN_POINT ( 'NONE',  ( -110.9537752465019054, -286.4036669783151865, -250.4724264816589141 ) ) ;
#73983 = CARTESIAN_POINT ( 'NONE',  ( 22.20477840730272234, -287.0677375418065367, -313.1214146159805978 ) ) ;
#73984 = CARTESIAN_POINT ( 'NONE',  ( 181.4475197844431023, 253.2525738607984636, -166.6027886999133614 ) ) ;
#73985 = VERTEX_POINT ( 'NONE', #8259 ) ;
#73986 = CARTESIAN_POINT ( 'NONE',  ( -37.51858574207007280, -287.6290242378129847, -346.7846581648530560 ) ) ;
#73987 = CARTESIAN_POINT ( 'NONE',  ( -48.06828069080074783, -288.8589574907578594, -342.6411516971366495 ) ) ;
#73988 = ORIENTED_EDGE ( 'NONE', *, *, #60912, .T. ) ;
#73989 = CARTESIAN_POINT ( 'NONE',  ( -113.8445911960692740, -285.7080996857646937, -264.2864697702846684 ) ) ;
#73990 = CARTESIAN_POINT ( 'NONE',  ( 9.495392128865923098, -275.0500366565785271, -214.2737113012912857 ) ) ;
#73991 = CARTESIAN_POINT ( 'NONE',  ( 15.23629030490137204, -291.6938436256614295, -214.4576656514300623 ) ) ;
#73992 = CARTESIAN_POINT ( 'NONE',  ( -2.931002068478880673, -283.2608556296496545, -339.1450526373840830 ) ) ;
#73993 = EDGE_CURVE ( 'NONE', #14152, #35152, #87642, .T. ) ;
#73994 = CARTESIAN_POINT ( 'NONE',  ( 32.53024891969280930, -282.6775741676256075, -239.6916137929241017 ) ) ;
#73995 = CARTESIAN_POINT ( 'NONE',  ( 17.81409120262141244, -282.6225527137782478, -324.1362916875922906 ) ) ;
#73996 = CIRCLE ( 'NONE', #16549, 4.003189038634634045 ) ;
#73997 = CARTESIAN_POINT ( 'NONE',  ( 31.98288692825983404, -272.6237833571632905, -237.0123917617631264 ) ) ;
#73998 = CARTESIAN_POINT ( 'NONE',  ( -113.5233723423151844, -274.1796448693337425, -270.3818398631209448 ) ) ;
#73999 = VERTEX_POINT ( 'NONE', #23858 ) ;
#74000 = CARTESIAN_POINT ( 'NONE',  ( 34.66882665568951438, -277.8154144072465215, -290.7676487879307956 ) ) ;
#74001 = CARTESIAN_POINT ( 'NONE',  ( 83.75835951168025417, 83.55189833975310876, -301.8609685986378963 ) ) ;
#74002 = CARTESIAN_POINT ( 'NONE',  ( -92.81635225106667519, -296.5777067063164623, -222.7345601121778316 ) ) ;
#74003 = CARTESIAN_POINT ( 'NONE',  ( 22.16565205169789721, -292.4044017913836342, -221.5922555796551023 ) ) ;
#74004 = CARTESIAN_POINT ( 'NONE',  ( -69.44094709307063340, -196.3684237509906438, -356.8806884016171921 ) ) ;
#74006 = CARTESIAN_POINT ( 'NONE',  ( -78.63877396349961657, -288.0180704208287352, -331.5863002574434404 ) ) ;
#74005 = CARTESIAN_POINT ( 'NONE',  ( -9.360389901375182120, -296.9707284207239582, -193.9569664623705023 ) ) ;
#74007 = CARTESIAN_POINT ( 'NONE',  ( -94.01021694886543401, -297.7421531344366485, -318.3343705354888016 ) ) ;
#74008 = CARTESIAN_POINT ( 'NONE',  ( 31.43018154816243381, -288.5220917264987293, -244.3009173340606992 ) ) ;
#74009 = ORIENTED_EDGE ( 'NONE', *, *, #65011, .T. ) ;
#74010 = CARTESIAN_POINT ( 'NONE',  ( 22.99419793529893141, -295.1302093936623123, -317.8416640315668928 ) ) ;
#74011 = CARTESIAN_POINT ( 'NONE',  ( -93.46532047161268508, -284.3812961703030169, -317.1385450321559460 ) ) ;
#74012 = CARTESIAN_POINT ( 'NONE',  ( -108.5139559848918367, -295.7099174771433354, -241.8898842515198737 ) ) ;
#74013 = CARTESIAN_POINT ( 'NONE',  ( -72.10836744950326249, -292.4070185617318316, -201.8232849165753748 ) ) ;
#74014 = CARTESIAN_POINT ( 'NONE',  ( 34.40316898700486803, -293.6905211723409934, -242.4254207124098457 ) ) ;
#74015 = CARTESIAN_POINT ( 'NONE',  ( -74.98142758465684210, -291.7027069911534340, -207.7541127260791711 ) ) ;
#74016 = ORIENTED_EDGE ( 'NONE', *, *, #25097, .T. ) ;
#74017 = DIRECTION ( 'NONE',  ( 1.000000000000000000, 0.000000000000000000, 0.000000000000000000 ) ) ;
#74018 = CARTESIAN_POINT ( 'NONE',  ( -59.80484286905655011, -299.6247338728821887, -197.9482555088488027 ) ) ;
#74019 = CARTESIAN_POINT ( 'NONE',  ( -5.266476787068576471, -273.2598862934049748, -200.7968400251429841 ) ) ;
#74020 = EDGE_CURVE ( 'NONE', #76130, #44950, #67990, .T. ) ;
#74021 = VERTEX_POINT ( 'NONE', #66048 ) ;
#74022 = CARTESIAN_POINT ( 'NONE',  ( -11.89246028269889521, -276.2373537007119353, -343.0245947462095728 ) ) ;
#74023 = CARTESIAN_POINT ( 'NONE',  ( -48.98174036788562802, -272.3014056643684739, -197.4331210636979677 ) ) ;
#74024 = CARTESIAN_POINT ( 'NONE',  ( -110.7092802395923030, -280.2657719315449185, -281.6776399509125213 ) ) ;
#74025 = CARTESIAN_POINT ( 'NONE',  ( 10.44132800435818176, -274.5237536264277765, -327.1735083567404558 ) ) ;
#74026 = CARTESIAN_POINT ( 'NONE',  ( -102.8938401618347598, -298.2042568843719437, -237.2320412923612309 ) ) ;
#74027 = CARTESIAN_POINT ( 'NONE',  ( -109.8173900607150273, -273.6363086341236226, -259.4935747174474727 ) ) ;
#74028 = CARTESIAN_POINT ( 'NONE',  ( 29.88879290598534411, -300.4807074052612279, -194.1431463050642492 ) ) ;
#74029 = CARTESIAN_POINT ( 'NONE',  ( -70.65253295767170982, -271.6351552179695545, -202.7682542806483923 ) ) ;
#74030 = CARTESIAN_POINT ( 'NONE',  ( -18.18581442662500791, -295.4500627239226560, -340.9085822236979766 ) ) ;
#74031 = CARTESIAN_POINT ( 'NONE',  ( 13.32186135899736712, -291.3526097137193460, -216.9890423849845433 ) ) ;
#74032 = DIRECTION ( 'NONE',  ( 1.000000000000000000, 0.000000000000000000, 0.000000000000000000 ) ) ;
#74033 = CARTESIAN_POINT ( 'NONE',  ( -65.06703844468856346, -277.8970583573882891, -342.1866575937361858 ) ) ;
#74034 = CARTESIAN_POINT ( 'NONE',  ( 20.68023803851075115, -275.0956008965272872, -226.0409415048833921 ) ) ;
#74035 = CARTESIAN_POINT ( 'NONE',  ( -107.7797056379767042, -282.8528943729294269, -300.3594966493653828 ) ) ;
#74036 = CARTESIAN_POINT ( 'NONE',  ( -80.79070720895846591, -297.6399208026963379, -331.7615506574988444 ) ) ;
#74037 = DIRECTION ( 'NONE',  ( -1.000000000000000000, 0.000000000000000000, 0.000000000000000000 ) ) ;
#74038 = CARTESIAN_POINT ( 'NONE',  ( -68.83520217444021227, -284.8243469092976738, -204.3112403664440251 ) ) ;
#74039 = CARTESIAN_POINT ( 'NONE',  ( -107.5986887696888914, -282.2038508086868092, -297.2267664648894083 ) ) ;
#74040 = CARTESIAN_POINT ( 'NONE',  ( -111.2935362167384028, -276.7527542278039618, -273.3777303605774591 ) ) ;
#74041 = CARTESIAN_POINT ( 'NONE',  ( -109.3450387087716678, -276.9280324707634691, -285.5563195962548093 ) ) ;
#74042 = CARTESIAN_POINT ( 'NONE',  ( 6.497960560500725791, -282.6475964659681495, -209.4448455354399812 ) ) ;
#74043 = CARTESIAN_POINT ( 'NONE',  ( -27.25069010524445901, -275.3881972586881943, -197.6098607496846000 ) ) ;
#74044 = CARTESIAN_POINT ( 'NONE',  ( 175.2296996224750103, 20.99999999999998934, 24.00000000000000355 ) ) ;
#74045 = CARTESIAN_POINT ( 'NONE',  ( -68.49812611553188901, -272.0494656572178087, -200.8075507593206055 ) ) ;
#74046 = CARTESIAN_POINT ( 'NONE',  ( -78.91844335957073042, -281.4937130275479831, -207.6775619331630480 ) ) ;
#74047 = CARTESIAN_POINT ( 'NONE',  ( 152.4536156746142410, 250.0000000000000568, 14.50000000000000000 ) ) ;
#74048 = CARTESIAN_POINT ( 'NONE',  ( -7.926708649766956327, -288.3545367623178777, -200.7061602810057366 ) ) ;
#74049 = DIRECTION ( 'NONE',  ( -0.000000000000000000, -0.000000000000000000, -1.000000000000000000 ) ) ;
#74050 = CARTESIAN_POINT ( 'NONE',  ( -70.12307423234990722, -287.4837946938689583, -337.8316282302185414 ) ) ;
#74051 = CARTESIAN_POINT ( 'NONE',  ( 82.12347693879148380, -301.5478687382300222, -195.3203844934047311 ) ) ;
#74052 = CARTESIAN_POINT ( 'NONE',  ( -34.44493754159675802, -296.8841301922085449, -196.9646518883128010 ) ) ;
#74053 = CARTESIAN_POINT ( 'NONE',  ( -109.8746062731175925, -288.4859813781841353, -286.2267237104661035 ) ) ;
#74054 = CARTESIAN_POINT ( 'NONE',  ( 197.2116108777964030, 281.1590520725322335, -110.1526527170710921 ) ) ;
#74055 = CARTESIAN_POINT ( 'NONE',  ( -34.35568795768310935, -296.0893742577463286, -195.3621272966507263 ) ) ;
#74056 = CARTESIAN_POINT ( 'NONE',  ( 38.65517597159660568, -286.1187184660389562, -277.2300752977436673 ) ) ;
#74057 = CARTESIAN_POINT ( 'NONE',  ( -73.11585798146181503, -283.8248703265669519, -203.2641755041348404 ) ) ;
#74058 = CARTESIAN_POINT ( 'NONE',  ( -107.3952957145899489, -290.8242974950010193, -249.7864196659722609 ) ) ;
#74059 = CARTESIAN_POINT ( 'NONE',  ( 9.638876423637331214, -282.1382749288294463, -213.6537281136629929 ) ) ;
#74060 = CARTESIAN_POINT ( 'NONE',  ( 33.60967859368582822, -282.1193723256164958, -252.4635796065689419 ) ) ;
#74061 = CARTESIAN_POINT ( 'NONE',  ( -110.3226172204161060, -292.2914602069034800, -289.1794629474961198 ) ) ;
#74062 = AXIS2_PLACEMENT_3D ( 'NONE', #63052, #56403, #57345 ) ;
#74063 = CARTESIAN_POINT ( 'NONE',  ( 19.38657721681793333, -298.9107079942916698, -193.3595438923215113 ) ) ;
#74064 = EDGE_LOOP ( 'NONE', ( #71945, #41972, #49335, #35367 ) ) ;
#74065 = CARTESIAN_POINT ( 'NONE',  ( -77.39423046762806280, -287.6643403369684506, -334.4932875205238929 ) ) ;
#74066 = CARTESIAN_POINT ( 'NONE',  ( 38.49210793758086879, -275.3842445764277045, -256.9353631442095320 ) ) ;
#74068 = CARTESIAN_POINT ( 'NONE',  ( 16.03440785392185930, -294.7929590593000171, -218.1062932318696710 ) ) ;
#74067 = AXIS2_PLACEMENT_3D ( 'NONE', #35165, #64564, #77325 ) ;
#74069 = DIRECTION ( 'NONE',  ( 0.000000000000000000, 0.000000000000000000, 1.000000000000000000 ) ) ;
#74070 = CARTESIAN_POINT ( 'NONE',  ( 35.77081079830085031, -283.8376638359844719, -253.6410175316879361 ) ) ;
#74071 = CARTESIAN_POINT ( 'NONE',  ( -56.48237439469045285, -275.2979696095242161, -343.1036746451746353 ) ) ;
#74072 = DIRECTION ( 'NONE',  ( 0.000000000000000000, 1.000000000000000000, 0.000000000000000000 ) ) ;
#74073 = CARTESIAN_POINT ( 'NONE',  ( -77.76067872853617757, -295.9187959603378317, -205.7643178802415491 ) ) ;
#74074 = CARTESIAN_POINT ( 'NONE',  ( -31.32306011502545573, -273.4787235356348560, -197.4947024048278763 ) ) ;
#74075 = CARTESIAN_POINT ( 'NONE',  ( -102.2446926663671434, -291.5994798883600083, -305.3735453317185602 ) ) ;
#74076 = CARTESIAN_POINT ( 'NONE',  ( -70.33742643559412500, -292.5473594625576652, -204.9800007217740472 ) ) ;
#74077 = CARTESIAN_POINT ( 'NONE',  ( -92.28835985056018387, -287.0133692145570876, -220.6991060442264541 ) ) ;
#74078 = CARTESIAN_POINT ( 'NONE',  ( -6.144246839916199576, -293.8793714446516105, -200.5950576397290774 ) ) ;
#74079 = CARTESIAN_POINT ( 'NONE',  ( 17.12666970094143082, -294.1239784272474935, -216.5604260796218341 ) ) ;
#74080 = CARTESIAN_POINT ( 'NONE',  ( 33.44554181360330603, -293.6208820830340755, -288.1983370152443058 ) ) ;
#74081 = CARTESIAN_POINT ( 'NONE',  ( 34.17317958005470757, -289.2602468526873167, -247.7212091064836272 ) ) ;
#74082 = CARTESIAN_POINT ( 'NONE',  ( 37.54886640620244265, -281.9433491754959391, -288.3171717360264665 ) ) ;
#74083 = CARTESIAN_POINT ( 'NONE',  ( -9.741444982281025844, -296.4749431538819522, -194.8100556288417522 ) ) ;
#74084 = CARTESIAN_POINT ( 'NONE',  ( -100.9952947267095311, -284.9579023370150708, -226.9400380962346446 ) ) ;
#74085 = CARTESIAN_POINT ( 'NONE',  ( 24.39892694632474601, -276.9611834918085265, -228.3865420773499295 ) ) ;
#74086 = EDGE_CURVE ( 'NONE', #86133, #66468, #58924, .T. ) ;
#74087 = CARTESIAN_POINT ( 'NONE',  ( -81.70645854460470048, -284.2274422445447044, -211.8897684659552851 ) ) ;
#74088 = CARTESIAN_POINT ( 'NONE',  ( 37.36499653700855106, -285.4597184632267499, -263.1749040344540163 ) ) ;
#74089 = CARTESIAN_POINT ( 'NONE',  ( -112.8112183209951951, -276.7839227141478773, -263.1082201134603338 ) ) ;
#74090 = CARTESIAN_POINT ( 'NONE',  ( -112.8394912670188432, -266.8193566212495966, -283.2716462811306428 ) ) ;
#74091 = CARTESIAN_POINT ( 'NONE',  ( -98.15481678675584476, -284.6214697438447843, -229.8672507439929404 ) ) ;
#74092 = CARTESIAN_POINT ( 'NONE',  ( 34.22205117453609802, -283.1049434256077575, -297.6857994496793367 ) ) ;
#74093 = CARTESIAN_POINT ( 'NONE',  ( 38.85548804555890712, -286.7331400490336364, -280.1052448063181259 ) ) ;
#74094 = CARTESIAN_POINT ( 'NONE',  ( -6.320047787611907886, -296.3990595258504186, -337.5595636656794341 ) ) ;
#74095 = CARTESIAN_POINT ( 'NONE',  ( -105.6194086025502941, -279.7115288435012985, -304.3116333470424024 ) ) ;
#74096 = CARTESIAN_POINT ( 'NONE',  ( -25.82755104337161001, -278.2235887362064659, -345.9965768796326984 ) ) ;
#74097 = CARTESIAN_POINT ( 'NONE',  ( -109.9042652887385714, -278.2743104563852512, -278.7877087598748744 ) ) ;
#74098 = CARTESIAN_POINT ( 'NONE',  ( -87.34373792482682575, -299.3530998771738041, -214.6850491549435276 ) ) ;
#74099 = CARTESIAN_POINT ( 'NONE',  ( 14.42574231205511559, -284.7815316515611244, -216.2510939733350597 ) ) ;
#74100 = CARTESIAN_POINT ( 'NONE',  ( -112.5670063441248487, -291.9987437865419793, -282.5099335869472270 ) ) ;
#74101 = CARTESIAN_POINT ( 'NONE',  ( -61.12640126555984210, -294.2885130424811564, -339.7583732013938516 ) ) ;
#74102 = ORIENTED_EDGE ( 'NONE', *, *, #41537, .F. ) ;
#74103 = CARTESIAN_POINT ( 'NONE',  ( 34.34432392533349798, -293.4021767407929815, -284.2608101467076267 ) ) ;
#74104 = CARTESIAN_POINT ( 'NONE',  ( -112.6241767957439208, -291.8163863148431005, -255.6624973926950872 ) ) ;
#74105 = CARTESIAN_POINT ( 'NONE',  ( -96.49305964120316048, -279.8038530137138196, -227.4075461153082642 ) ) ;
#74106 = CARTESIAN_POINT ( 'NONE',  ( -113.6275033766746816, -271.7183020747088449, -261.7997842456563262 ) ) ;
#74107 = CARTESIAN_POINT ( 'NONE',  ( 9.741791337865567613, -287.3326975390622238, -209.5626178559400046 ) ) ;
#74108 = EDGE_CURVE ( 'NONE', #40624, #74338, #27174, .T. ) ;
#74109 = CARTESIAN_POINT ( 'NONE',  ( 10.21821628200788723, -288.7500546430942450, -330.9582543885248924 ) ) ;
#74110 = CARTESIAN_POINT ( 'NONE',  ( -94.97636106151357183, -285.5172047747840338, -225.5040721867185880 ) ) ;
#74111 = CARTESIAN_POINT ( 'NONE',  ( 201.2104617360081704, 60.19600395700749829, 7.000000000000000000 ) ) ;
#74112 = CARTESIAN_POINT ( 'NONE',  ( 197.8085509907933499, 288.8371460693426229, -97.00402988771099899 ) ) ;
#74113 = CARTESIAN_POINT ( 'NONE',  ( -107.9091210890304922, -264.1399593486416393, -305.3610597610020818 ) ) ;
#74114 = CARTESIAN_POINT ( 'NONE',  ( -51.32173023620880059, -276.4326623318781344, -342.1744905856324408 ) ) ;
#74115 = CARTESIAN_POINT ( 'NONE',  ( -56.69495985702592833, -276.2277734727795178, -341.1222383648528762 ) ) ;
#74116 = CARTESIAN_POINT ( 'NONE',  ( -113.5227515574856199, -272.3617025945729893, -258.9436525938332920 ) ) ;
#74117 = CARTESIAN_POINT ( 'NONE',  ( 7.421282116121920680, -59.95783495620983672, -352.0918686609887231 ) ) ;
#74118 = CARTESIAN_POINT ( 'NONE',  ( -109.2788355681009591, -276.9041559917061477, -296.5612820402409966 ) ) ;
#74119 = CARTESIAN_POINT ( 'NONE',  ( -30.65746628350342107, -296.7288736711072943, -346.0532247793873353 ) ) ;
#74120 = CARTESIAN_POINT ( 'NONE',  ( 4.533786936460485251, -293.1263665521543658, -210.4289775808706793 ) ) ;
#74121 = CARTESIAN_POINT ( 'NONE',  ( -100.6234947798112529, -297.9318373175615307, -226.7538968511926214 ) ) ;
#74122 = CARTESIAN_POINT ( 'NONE',  ( -90.09896791709276442, -273.9815612777582601, -214.3421386863742271 ) ) ;
#74123 = CARTESIAN_POINT ( 'NONE',  ( -105.9864616521684439, -296.3861943176669342, -295.3471470798364180 ) ) ;
#74124 = EDGE_LOOP ( 'NONE', ( #84131, #75390, #89821, #46553, #4105, #20680 ) ) ;
#74125 = DIRECTION ( 'NONE',  ( 0.000000000000000000, 0.000000000000000000, 1.000000000000000000 ) ) ;
#74126 = CARTESIAN_POINT ( 'NONE',  ( -40.96428677039318700, -281.9270822897667585, -194.8750545159856813 ) ) ;
#74127 = EDGE_CURVE ( 'NONE', #34178, #44986, #69521, .T. ) ;
#74128 = AXIS2_PLACEMENT_3D ( 'NONE', #82120, #89674, #17738 ) ;
#74129 = CARTESIAN_POINT ( 'NONE',  ( -24.54999144379014098, -282.4008824602091181, -346.2828319175758338 ) ) ;
#74130 = CARTESIAN_POINT ( 'NONE',  ( -103.4036249863241039, -279.2022535986235425, -302.2597875590351464 ) ) ;
#74131 = CARTESIAN_POINT ( 'NONE',  ( -71.10024695211329515, -279.2517252425743095, -338.4370647884793470 ) ) ;
#74132 = CIRCLE ( 'NONE', #80156, 6.654241149514406040 ) ;
#74133 = CARTESIAN_POINT ( 'NONE',  ( -54.35297439646813444, -272.3095128412138592, -198.6580894672950421 ) ) ;
#74134 = DIRECTION ( 'NONE',  ( -1.000000000000000000, 0.000000000000000000, -0.000000000000000000 ) ) ;
#74135 = FACE_OUTER_BOUND ( 'NONE', #14883, .T. ) ;
#74136 = CARTESIAN_POINT ( 'NONE',  ( -43.75320516041123398, -280.1356946007289821, -197.5929865935247278 ) ) ;
#74137 = CARTESIAN_POINT ( 'NONE',  ( 25.93972252484041974, -276.9326244026899531, -314.0378611791103367 ) ) ;
#74138 = CARTESIAN_POINT ( 'NONE',  ( 9.302661250104792501, -278.4119172560397146, -329.1582303168679573 ) ) ;
#74139 = CARTESIAN_POINT ( 'NONE',  ( 23.88455896225976005, -274.7397553729381912, -316.0771052533010561 ) ) ;
#74140 = ORIENTED_EDGE ( 'NONE', *, *, #49739, .T. ) ;
#74141 = CARTESIAN_POINT ( 'NONE',  ( 197.9931848602547007, 41.98013133710430367, 9.866139269262600209 ) ) ;
#74142 = CARTESIAN_POINT ( 'NONE',  ( 37.64409719623136397, -283.6337449956719752, -278.3192184821394903 ) ) ;
#74143 = CARTESIAN_POINT ( 'NONE',  ( -77.33489659352031254, -290.6976595528046801, -209.0981931161518617 ) ) ;
#74144 = ADVANCED_FACE ( 'NONE', ( #75913 ), #17699, .F. ) ;
#74145 = CARTESIAN_POINT ( 'NONE',  ( 38.87534378137304003, -286.7728627327135200, -260.1496046652058567 ) ) ;
#74146 = CARTESIAN_POINT ( 'NONE',  ( -109.0808821390584313, -282.5550031631399293, -288.5672647534580051 ) ) ;
#74148 = CARTESIAN_POINT ( 'NONE',  ( 27.63605345376637956, -285.1435730492021321, -233.9347213795768994 ) ) ;
#74147 = CARTESIAN_POINT ( 'NONE',  ( 14.32556134786536539, -280.8835305204922861, -322.8338868396316457 ) ) ;
#74149 = CARTESIAN_POINT ( 'NONE',  ( -35.66905315835412438, -281.2786454423715554, -196.9706347262064696 ) ) ;
#74150 = CARTESIAN_POINT ( 'NONE',  ( -110.4869523937869644, -270.7648327691349550, -253.7848480562450106 ) ) ;
#74151 = CARTESIAN_POINT ( 'NONE',  ( -49.98108835201040279, -281.6105708526275748, -345.5588711938694360 ) ) ;
#74152 = CARTESIAN_POINT ( 'NONE',  ( -11.71597919749275007, -296.7187942265700258, -340.9025581638647964 ) ) ;
#74153 = CARTESIAN_POINT ( 'NONE',  ( -103.2192761891207340, -278.7740643137713619, -302.1647717303428067 ) ) ;
#74154 = CARTESIAN_POINT ( 'NONE',  ( -102.4651287664665915, -287.0533518826933914, -232.7213364136994755 ) ) ;
#74155 = CARTESIAN_POINT ( 'NONE',  ( 185.4166944662832179, 250.5000000000000568, 23.37680765314684450 ) ) ;
#74156 = CARTESIAN_POINT ( 'NONE',  ( -94.58627324178790730, -293.1511046174771309, -221.0222393547170441 ) ) ;
#74157 = CARTESIAN_POINT ( 'NONE',  ( -13.16411792140720571, -274.7380510624283829, -341.4117965440746048 ) ) ;
#74158 = CARTESIAN_POINT ( 'NONE',  ( -34.68266843584159176, -288.2167057135251866, -347.1536200344426106 ) ) ;
#74159 = CARTESIAN_POINT ( 'NONE',  ( 34.21682604564620789, -292.1876656275298956, -288.4115403876330106 ) ) ;
#74160 = CARTESIAN_POINT ( 'NONE',  ( -48.18343439339133027, -268.4940904799746590, -439.4148130071812375 ) ) ;
#74161 = CARTESIAN_POINT ( 'NONE',  ( -106.7353611553109687, -276.9153732991545098, -294.7181068949386145 ) ) ;
#74162 = CARTESIAN_POINT ( 'NONE',  ( -102.5636530326079736, -294.2158886811116076, -305.8147826327883081 ) ) ;
#74163 = CARTESIAN_POINT ( 'NONE',  ( -92.77272076091672659, -291.1831901360292818, -318.6931876558040244 ) ) ;
#74164 = CARTESIAN_POINT ( 'NONE',  ( 219.8344101925596021, 3.000000000000000000, -10.00000000000000000 ) ) ;
#74165 = CARTESIAN_POINT ( 'NONE',  ( 164.2231345125756263, 291.1800221208779931, -7.499999999999996447 ) ) ;
#74166 = CARTESIAN_POINT ( 'NONE',  ( 10.69745547976779321, -291.1818454733262342, -211.0061316691098625 ) ) ;
#74167 = CARTESIAN_POINT ( 'NONE',  ( 24.18992803154551297, -288.5919580142817154, -229.5218649911083730 ) ) ;
#74168 = CARTESIAN_POINT ( 'NONE',  ( -83.63106771943982665, -289.6671792578274562, -210.0348093011902222 ) ) ;
#74169 = CARTESIAN_POINT ( 'NONE',  ( 32.83002768453177822, -288.6854514182113576, -248.1535970871363190 ) ) ;
#74170 = LINE ( 'NONE', #65716, #62263 ) ;
#74171 = CARTESIAN_POINT ( 'NONE',  ( 29.57688611577420801, -288.7535752083965122, -300.0588731016520114 ) ) ;
#74172 = CARTESIAN_POINT ( 'NONE',  ( 21.89469560021595385, -296.1686814398810270, -316.9592505720563054 ) ) ;
#74173 = DIRECTION ( 'NONE',  ( -0.000000000000000000, -1.000000000000000000, -0.000000000000000000 ) ) ;
#74174 = CARTESIAN_POINT ( 'NONE',  ( -9.692263026995922459, -289.9039067114023851, -341.8000243749643801 ) ) ;
#74175 = CARTESIAN_POINT ( 'NONE',  ( -28.39472212691228847, -278.1850952643001733, -195.4864586905876820 ) ) ;
#74176 = CARTESIAN_POINT ( 'NONE',  ( -114.2106668508827170, -278.8339957343091555, -274.4728385972733236 ) ) ;
#74177 = CARTESIAN_POINT ( 'NONE',  ( -33.91196636635813633, -279.7609149242800868, -193.4587043800007962 ) ) ;
#74178 = CARTESIAN_POINT ( 'NONE',  ( -105.2246696219695679, -298.9429321745295738, -239.1923035306274983 ) ) ;
#74179 = CARTESIAN_POINT ( 'NONE',  ( -111.3918456094949505, -282.7058103652747718, -258.3813427142728187 ) ) ;
#74180 = CARTESIAN_POINT ( 'NONE',  ( -48.18343439339132317, -264.8229914578101329, -496.4753680103029296 ) ) ;
#74181 = CARTESIAN_POINT ( 'NONE',  ( 10.08355039165451394, -278.8531153773471942, -213.1826983043261237 ) ) ;
#74182 = CARTESIAN_POINT ( 'NONE',  ( -80.43381689840293802, -281.6355078497830959, -331.8089213787535527 ) ) ;
#74183 = CARTESIAN_POINT ( 'NONE',  ( 189.9243309297870610, 249.5000000000000568, 20.22542485937349355 ) ) ;
#74184 = CARTESIAN_POINT ( 'NONE',  ( 25.48492106058643714, -274.6100447701479652, -313.7598548026060143 ) ) ;
#74185 = CARTESIAN_POINT ( 'NONE',  ( -71.23258788700917421, -297.0281155915316731, -335.8131086055824426 ) ) ;
#74186 = CARTESIAN_POINT ( 'NONE',  ( -27.42574595424867212, -281.8494419526655292, -346.4613967982887743 ) ) ;
#74187 = CARTESIAN_POINT ( 'NONE',  ( -102.9737209920723870, -297.0529721176575890, -302.9694683793557033 ) ) ;
#74188 = CARTESIAN_POINT ( 'NONE',  ( -29.14231603631001732, -299.4679527596301227, -193.8524759526805497 ) ) ;
#74189 = CARTESIAN_POINT ( 'NONE',  ( -1.708603960716748027, -274.2049357877133957, -206.6100763448369548 ) ) ;
#74190 = CARTESIAN_POINT ( 'NONE',  ( -2.735465052274779207, -294.5098884657392091, -203.8223387212208024 ) ) ;
#74191 = CARTESIAN_POINT ( 'NONE',  ( 37.50491720582801491, -287.9456423537644696, -288.4995206869028834 ) ) ;
#74192 = CARTESIAN_POINT ( 'NONE',  ( -11.96942020510595484, -278.4595397325391559, -199.1334162389412654 ) ) ;
#74193 = CARTESIAN_POINT ( 'NONE',  ( -104.6089459959524817, -290.8712549167677253, -232.8895602642143388 ) ) ;
#74195 = CARTESIAN_POINT ( 'NONE',  ( -10.64947778649820798, -287.7541318172500837, -338.6132590646933522 ) ) ;
#74194 = CIRCLE ( 'NONE', #12671, 1.000000000000000888 ) ;
#74196 = CARTESIAN_POINT ( 'NONE',  ( 5.378483930638676469, -290.6302035946492310, -208.7170872873702479 ) ) ;
#74197 = EDGE_LOOP ( 'NONE', ( #92389, #82694, #82950, #67335 ) ) ;
#74198 = CARTESIAN_POINT ( 'NONE',  ( 154.1415209985679269, 20.37991841447902175, 11.45812909362559040 ) ) ;
#74199 = CARTESIAN_POINT ( 'NONE',  ( -98.89698570470234529, -289.5158858671409803, -309.7176328080411167 ) ) ;
#74200 = DIRECTION ( 'NONE',  ( 0.000000000000000000, 1.000000000000000000, 0.000000000000000000 ) ) ;
#74201 = CONICAL_SURFACE ( 'NONE', #1614, 6.500000000000024869, 0.7853981633974488341 ) ;
#74202 = CARTESIAN_POINT ( 'NONE',  ( -33.75036370400606955, -287.0375576705206413, -193.6804651681037797 ) ) ;
#74203 = CARTESIAN_POINT ( 'NONE',  ( 7.399455738971494334, -289.1948066931273615, -214.2051214447836571 ) ) ;
#74204 = CARTESIAN_POINT ( 'NONE',  ( -61.52883221686803239, -294.4174750897554986, -343.2713593892869994 ) ) ;
#74205 = CARTESIAN_POINT ( 'NONE',  ( 15.42559372803626694, -283.6399427132246274, -325.7588703823795981 ) ) ;
#74206 = CARTESIAN_POINT ( 'NONE',  ( -108.4257852916168474, -284.1656393340111890, -287.0305788076659610 ) ) ;
#74207 = CARTESIAN_POINT ( 'NONE',  ( 34.60067056430946053, -276.6697423702598257, -255.2817985388676334 ) ) ;
#74208 = CARTESIAN_POINT ( 'NONE',  ( 17.97365442908223443, -290.8692873434143848, -220.1648392913227497 ) ) ;
#74209 = CARTESIAN_POINT ( 'NONE',  ( -3.910196677923111430, -273.2982361392400890, -205.0058636741025566 ) ) ;
#74210 = ORIENTED_EDGE ( 'NONE', *, *, #12108, .T. ) ;
#74211 = CARTESIAN_POINT ( 'NONE',  ( 82.64890176555634582, -299.5541904835127980, -193.4639945212225882 ) ) ;
#74212 = CARTESIAN_POINT ( 'NONE',  ( -57.81342177691675488, -287.7060124194463242, -198.7377550460897453 ) ) ;
#74213 = CARTESIAN_POINT ( 'NONE',  ( -102.8444006202213501, -297.1088799957351512, -310.2470645987006037 ) ) ;
#74214 = CARTESIAN_POINT ( 'NONE',  ( -96.66239236556258163, -285.8003595659675966, -227.6203485177996697 ) ) ;
#74215 = CARTESIAN_POINT ( 'NONE',  ( -86.95229483053950048, -276.7816050235325633, -329.0106157297087179 ) ) ;
#74216 = CARTESIAN_POINT ( 'NONE',  ( -3.373863047587286168, -293.1402728206653023, -201.3574793792092237 ) ) ;
#74217 = CARTESIAN_POINT ( 'NONE',  ( 30.56957947083360949, -286.1318155425817054, -304.0704878820728823 ) ) ;
#74218 = CARTESIAN_POINT ( 'NONE',  ( -13.78447876091214930, -295.0878441723444894, -343.6468711199851782 ) ) ;
#74219 = CARTESIAN_POINT ( 'NONE',  ( -95.13372741009565914, -291.5136508546605683, -225.7273967675308768 ) ) ;
#74220 = DIRECTION ( 'NONE',  ( -0.000000000000000000, 1.000000000000000000, 0.000000000000000000 ) ) ;
#74221 = CARTESIAN_POINT ( 'NONE',  ( 197.1513938986460062, -147.7221692137691775, 1.978481845683761620 ) ) ;
#74222 = CARTESIAN_POINT ( 'NONE',  ( 202.9738562182569694, 291.9636489450776367, -53.99999999998589573 ) ) ;
#74223 = CARTESIAN_POINT ( 'NONE',  ( -110.2692008201007212, -286.3588767831299720, -247.7267792911372339 ) ) ;
#74224 = CARTESIAN_POINT ( 'NONE',  ( 99.50465036329318025, -297.2649936051624309, -195.4191791630918829 ) ) ;
#74225 = ORIENTED_EDGE ( 'NONE', *, *, #81096, .T. ) ;
#74226 = CARTESIAN_POINT ( 'NONE',  ( -16.05582445442620099, -281.6906413642141160, -340.5119381469079372 ) ) ;
#74227 = CARTESIAN_POINT ( 'NONE',  ( -109.7183351150041943, -277.8858906361336949, -296.7347603891257677 ) ) ;
#74228 = CARTESIAN_POINT ( 'NONE',  ( 37.17548521243185178, -283.4568815351546505, -262.9449483833741397 ) ) ;
#74229 = CARTESIAN_POINT ( 'NONE',  ( -53.95492635066413101, -170.5480224260624595, -362.9304601937118946 ) ) ;
#74230 = CARTESIAN_POINT ( 'NONE',  ( -47.19846773905869952, -281.7497809990708788, -346.1334772183409996 ) ) ;
#74231 = CARTESIAN_POINT ( 'NONE',  ( -37.25418869707253577, -284.0733264649528564, -195.7036466603310316 ) ) ;
#74232 = CARTESIAN_POINT ( 'NONE',  ( -41.15469939162760227, -275.8651894647484255, -194.6409025646760540 ) ) ;
#74233 = CARTESIAN_POINT ( 'NONE',  ( -109.7980990638689889, -297.1732283303375084, -260.5947241346065084 ) ) ;
#74234 = CARTESIAN_POINT ( 'NONE',  ( 4.080622000029026530, -293.1657283542152754, -331.0688992511239803 ) ) ;
#74235 = CARTESIAN_POINT ( 'NONE',  ( -110.5670492534069638, -278.9059964574320247, -294.0135811907408083 ) ) ;
#74236 = CARTESIAN_POINT ( 'NONE',  ( 23.98438602724380075, -276.1014720859656109, -310.0537069353559900 ) ) ;
#74237 = CARTESIAN_POINT ( 'NONE',  ( -99.32537813508778868, -274.2346074061051127, -225.1120375430513150 ) ) ;
#74238 = CARTESIAN_POINT ( 'NONE',  ( -96.82340113892685451, -276.8200872927554883, -318.7905676282600211 ) ) ;
#74239 = CARTESIAN_POINT ( 'NONE',  ( 199.3883137936200001, 289.5528945227777058, -97.47147507494776164 ) ) ;
#74240 = CARTESIAN_POINT ( 'NONE',  ( -88.15956483509424402, -275.7628482977409021, -325.5901777202634548 ) ) ;
#74241 = CARTESIAN_POINT ( 'NONE',  ( -27.80325290580884001, -296.3586970821630757, -346.2270913909829346 ) ) ;
#74242 = DIRECTION ( 'NONE',  ( 1.000000000000000000, 0.000000000000000000, 0.000000000000000000 ) ) ;
#74243 = CARTESIAN_POINT ( 'NONE',  ( 207.4345711710209343, 35.56792554197559042, 12.00000000000000000 ) ) ;
#74244 = CARTESIAN_POINT ( 'NONE',  ( -109.8017535281590114, -285.4814158217897671, -281.8114575661990102 ) ) ;
#74245 = CARTESIAN_POINT ( 'NONE',  ( -113.3275550324223957, -286.3167537601562458, -270.0091723368642533 ) ) ;
#74246 = CARTESIAN_POINT ( 'NONE',  ( 28.90582449703376966, -286.4840023110999141, -239.4554850190929756 ) ) ;
#74247 = CARTESIAN_POINT ( 'NONE',  ( -97.04098497541068014, -277.5526752548092304, -226.9740714690790071 ) ) ;
#74248 = CARTESIAN_POINT ( 'NONE',  ( -107.7106542079722686, -286.7233110525971256, -246.5552194900701863 ) ) ;
#74249 = CARTESIAN_POINT ( 'NONE',  ( -34.26518688321827000, -278.5713711660569629, -196.7193659866738074 ) ) ;
#74250 = CARTESIAN_POINT ( 'NONE',  ( -26.96422480088653373, -277.9967704120463168, -342.9320080064891840 ) ) ;
#74251 = CARTESIAN_POINT ( 'NONE',  ( 139.1539576904058606, 250.0000000000000568, 10.50000000000000000 ) ) ;
#74252 = CARTESIAN_POINT ( 'NONE',  ( -71.94240322811519661, -274.0743634838763114, -205.9558532541948068 ) ) ;
#74253 = CARTESIAN_POINT ( 'NONE',  ( 38.71289882921283976, -282.4921885438012623, -281.3090309299198566 ) ) ;
#74254 = CARTESIAN_POINT ( 'NONE',  ( 26.22622989088633005, -281.4713161893278084, -226.9248280585386226 ) ) ;
#74255 = ORIENTED_EDGE ( 'NONE', *, *, #17187, .F. ) ;
#74256 = ORIENTED_EDGE ( 'NONE', *, *, #36806, .F. ) ;
#74257 = CARTESIAN_POINT ( 'NONE',  ( 200.6868442215943844, 15.43634792868608940, -10.00000000000000355 ) ) ;
#74258 = CARTESIAN_POINT ( 'NONE',  ( 2.077802800986792153, -288.4343977221430464, -205.6586584570499099 ) ) ;
#74259 = CARTESIAN_POINT ( 'NONE',  ( -72.91647737234427495, -296.7650176620357456, -206.4311801504561004 ) ) ;
#74260 = EDGE_CURVE ( 'NONE', #15778, #92724, #54135, .T. ) ;
#74261 = CARTESIAN_POINT ( 'NONE',  ( -50.54069270061050645, -291.2364138903745356, -194.6042741902552393 ) ) ;
#74262 = CARTESIAN_POINT ( 'NONE',  ( 20.89355311358891854, -286.6623060109966445, -315.5408491286260073 ) ) ;
#74263 = CARTESIAN_POINT ( 'NONE',  ( 31.94815039128375744, -286.4542466626979262, -295.1460232981478953 ) ) ;
#74264 = CARTESIAN_POINT ( 'NONE',  ( -95.27990595236231286, -286.3888582228834707, -225.2819121754416187 ) ) ;
#74265 = CARTESIAN_POINT ( 'NONE',  ( -71.94129019521366786, -275.5093619187966851, -336.9176766755859376 ) ) ;
#74266 = CARTESIAN_POINT ( 'NONE',  ( -9.870945756821738470, -287.0991552338770703, -341.4371200483362827 ) ) ;
#74267 = CARTESIAN_POINT ( 'NONE',  ( -24.16303721481126843, -288.2204700402649564, -196.4752339651858790 ) ) ;
#74268 = CARTESIAN_POINT ( 'NONE',  ( -67.34603664332830419, -287.4445661234304339, -339.2796802088391246 ) ) ;
#74269 = CARTESIAN_POINT ( 'NONE',  ( 17.78986660362062011, -283.1789916838747558, -318.5681589442484096 ) ) ;
#74270 = CARTESIAN_POINT ( 'NONE',  ( -80.88947172212748171, -293.4626542202238397, -209.0943242593519926 ) ) ;
#74271 = CARTESIAN_POINT ( 'NONE',  ( 184.7149167944524493, 8.542400036368780647, 25.74970488511327815 ) ) ;
#74272 = CYLINDRICAL_SURFACE ( 'NONE', #89641, 239.0731808058633874 ) ;
#74273 = CARTESIAN_POINT ( 'NONE',  ( -90.63748525421374325, -299.2240114166103240, -216.7992520273537593 ) ) ;
#74274 = CARTESIAN_POINT ( 'NONE',  ( 22.25094745951394160, -280.1577587267901777, -227.9191802236357489 ) ) ;
#74275 = CARTESIAN_POINT ( 'NONE',  ( 19.09344709063815060, -280.2380545062007400, -319.7582313521128299 ) ) ;
#74276 = CARTESIAN_POINT ( 'NONE',  ( -2.050764562359526089, -293.7940121440358325, -338.6158517957313165 ) ) ;
#74277 = CARTESIAN_POINT ( 'NONE',  ( -68.36544722251517214, -296.0375658166813650, -203.3848713452751156 ) ) ;
#74278 = CARTESIAN_POINT ( 'NONE',  ( 28.01965655893107865, -274.1101830806572934, -306.0947473372763170 ) ) ;
#74279 = CARTESIAN_POINT ( 'NONE',  ( -39.68811552978801416, -296.3973767741737788, -343.8293186784129034 ) ) ;
#74280 = CARTESIAN_POINT ( 'NONE',  ( 199.0061125298537377, 250.5000000000000568, -7.725424859374024678 ) ) ;
#74281 = CARTESIAN_POINT ( 'NONE',  ( -34.76887997977183886, -296.5636955617469539, -194.0550975974727237 ) ) ;
#74282 = CARTESIAN_POINT ( 'NONE',  ( -110.6208171951045216, -294.5368397234319673, -290.4644763386635873 ) ) ;
#74283 = DIRECTION ( 'NONE',  ( -0.000000000000000000, 1.000000000000000000, -0.000000000000000000 ) ) ;
#74284 = CARTESIAN_POINT ( 'NONE',  ( 8.943109179223133864, -293.5086301619486449, -213.6357451189632286 ) ) ;
#74285 = CARTESIAN_POINT ( 'NONE',  ( 123.4306832106270946, -134.2391364535880882, 5.024999999999987921 ) ) ;
#74287 = CARTESIAN_POINT ( 'NONE',  ( 12.35487423371159821, -294.3371112082193122, -323.9023603761793879 ) ) ;
#74286 = CARTESIAN_POINT ( 'NONE',  ( -112.6811021722686235, -282.6131832261027625, -267.1586120766681915 ) ) ;
#74288 = CARTESIAN_POINT ( 'NONE',  ( -10.70203441136842493, -282.7142641241646857, -342.6626824732124987 ) ) ;
#74289 = CARTESIAN_POINT ( 'NONE',  ( -3.065630858972029138, -282.4214935763112635, -203.0082293663973019 ) ) ;
#74290 = CARTESIAN_POINT ( 'NONE',  ( -105.4114129437495535, -284.6844284073017661, -234.2990003802526928 ) ) ;
#74291 = CARTESIAN_POINT ( 'NONE',  ( -111.5138416205268754, -288.6846530816837344, -260.0519279142316122 ) ) ;
#74292 = CARTESIAN_POINT ( 'NONE',  ( -20.25526795762938548, -274.3380690714490129, -345.3683826091709648 ) ) ;
#74293 = CARTESIAN_POINT ( 'NONE',  ( -16.35131107719725208, -281.2656609137384862, -343.7787756204624543 ) ) ;
#74294 = CARTESIAN_POINT ( 'NONE',  ( -71.39193019565041709, -284.2773771114291321, -205.2318211071049916 ) ) ;
#74295 = CARTESIAN_POINT ( 'NONE',  ( -112.0131427866932796, -289.6920281034611548, -252.8777498112525564 ) ) ;
#74296 = CARTESIAN_POINT ( 'NONE',  ( 121.3395553409046670, -299.5541904835127980, -192.6222259952039622 ) ) ;
#74297 = CARTESIAN_POINT ( 'NONE',  ( -72.48781540059938777, -297.1256234784556796, -335.2692314726747327 ) ) ;
#74298 = CARTESIAN_POINT ( 'NONE',  ( -101.4071785498490641, -280.5296171531674645, -228.6213660314736558 ) ) ;
#74300 = CARTESIAN_POINT ( 'NONE',  ( 18.85509418752544164, -280.5576104057058728, -223.7154537223013904 ) ) ;
#74299 = CARTESIAN_POINT ( 'NONE',  ( -9.029914148653487516, -292.7039837757203600, -340.2508277693513037 ) ) ;
#74301 = CARTESIAN_POINT ( 'NONE',  ( 30.90332604778165049, -294.1788930963834900, -306.0208488668643554 ) ) ;
#74302 = CARTESIAN_POINT ( 'NONE',  ( -109.7354827147009360, -282.3547029023094979, -292.0499055703522231 ) ) ;
#74303 = CARTESIAN_POINT ( 'NONE',  ( -42.63881503186441790, -279.1191573715983054, -345.1738256140021122 ) ) ;
#74304 = CARTESIAN_POINT ( 'NONE',  ( -50.52529040036783670, -294.2834035789922495, -342.4000060569163679 ) ) ;
#74305 = CARTESIAN_POINT ( 'NONE',  ( -110.0384582495561432, -270.7993796880480204, -251.0517014249982708 ) ) ;
#74306 = ORIENTED_EDGE ( 'NONE', *, *, #39352, .T. ) ;
#74307 = DIRECTION ( 'NONE',  ( 0.000000000000000000, 0.000000000000000000, 1.000000000000000000 ) ) ;
#74308 = CARTESIAN_POINT ( 'NONE',  ( 35.55196497664078237, -283.7394077024633816, -286.4347110644710028 ) ) ;
#74309 = CARTESIAN_POINT ( 'NONE',  ( -68.54931480292256651, -294.9812553376125379, -336.4359937688024047 ) ) ;
#74310 = LINE ( 'NONE', #73405, #70058 ) ;
#74311 = CARTESIAN_POINT ( 'NONE',  ( 35.77081079830085031, -279.2666405000204009, -287.0812184334320705 ) ) ;
#74312 = CARTESIAN_POINT ( 'NONE',  ( -93.04804104595032754, -272.4743287490172179, -217.4178005367461708 ) ) ;
#74313 = ADVANCED_FACE ( 'NONE', ( #47953 ), #32371, .F. ) ;
#74314 = EDGE_CURVE ( 'NONE', #70030, #13153, #74998, .T. ) ;
#74315 = CARTESIAN_POINT ( 'NONE',  ( 38.29547707787573074, -288.7214397035533011, -258.7711607790917583 ) ) ;
#74316 = CARTESIAN_POINT ( 'NONE',  ( -89.81484536658261675, -291.1188366280158561, -219.6110536152962709 ) ) ;
#74317 = CARTESIAN_POINT ( 'NONE',  ( -74.87543661120152194, -281.0631348903510229, -206.8837973115952309 ) ) ;
#74318 = CARTESIAN_POINT ( 'NONE',  ( -21.78504608824203359, -275.8550072343882107, -198.2193760567121785 ) ) ;
#74319 = CARTESIAN_POINT ( 'NONE',  ( -67.45524397145867113, -278.4430546652495195, -203.4123589535383303 ) ) ;
#74320 = CARTESIAN_POINT ( 'NONE',  ( 13.11145476838443358, -278.3477951844204199, -325.9246729007232943 ) ) ;
#74321 = ORIENTED_EDGE ( 'NONE', *, *, #67056, .T. ) ;
#74322 = CARTESIAN_POINT ( 'NONE',  ( -76.43089144562425474, -273.3781816181504496, -203.9592119032449773 ) ) ;
#74323 = CARTESIAN_POINT ( 'NONE',  ( -63.32584561161473857, -293.6311159737196022, -200.6034059995096754 ) ) ;
#74324 = CARTESIAN_POINT ( 'NONE',  ( 159.6810783670777880, 8.542400036368780647, -9.000000000000001776 ) ) ;
#74325 = DIRECTION ( 'NONE',  ( 0.000000000000000000, 0.000000000000000000, 1.000000000000000000 ) ) ;
#74326 = CARTESIAN_POINT ( 'NONE',  ( -22.41359796218076283, -290.3807676340355783, -196.0280721708947453 ) ) ;
#74327 = CARTESIAN_POINT ( 'NONE',  ( -39.16460267741054935, -297.6954021136285178, -197.3503183705244908 ) ) ;
#74328 = DIRECTION ( 'NONE',  ( 0.000000000000000000, 0.000000000000000000, 1.000000000000000000 ) ) ;
#74329 = VECTOR ( 'NONE', #73755, 1000.000000000000000 ) ;
#74330 = CARTESIAN_POINT ( 'NONE',  ( -108.8311409013396656, -292.4144971234878199, -243.5277136732773897 ) ) ;
#74331 = CARTESIAN_POINT ( 'NONE',  ( -111.2586520408596868, -298.6233781216987495, -305.9938812882205070 ) ) ;
#74332 = CARTESIAN_POINT ( 'NONE',  ( -27.62305892795291129, -288.1760595998777035, -196.1615462988393972 ) ) ;
#74333 = CARTESIAN_POINT ( 'NONE',  ( 36.51239812411534302, -273.7112893900501263, -282.7400878787908027 ) ) ;
#74334 = CARTESIAN_POINT ( 'NONE',  ( 8.192834175133336672, -276.6007277210825350, -211.4720665324349511 ) ) ;
#74336 = CARTESIAN_POINT ( 'NONE',  ( -36.15920225219416295, -290.1469025963456829, -195.9177844392693544 ) ) ;
#74335 = CIRCLE ( 'NONE', #83377, 1.000000000000000888 ) ;
#74337 = CARTESIAN_POINT ( 'NONE',  ( -20.06134422237167669, -282.1321961327722079, -196.5393866169997352 ) ) ;
#74338 = VERTEX_POINT ( 'NONE', #76856 ) ;
#74339 = CARTESIAN_POINT ( 'NONE',  ( -21.37401719523599297, -282.1906402055314516, -341.7499092765669388 ) ) ;
#74340 = CARTESIAN_POINT ( 'NONE',  ( -112.9341364414093789, -279.7942230935132102, -257.4275924630767918 ) ) ;
#74341 = CARTESIAN_POINT ( 'NONE',  ( -35.92202204239944052, -281.8296820789292383, -346.9639398720143504 ) ) ;
#74342 = CARTESIAN_POINT ( 'NONE',  ( -95.96173002589530654, -278.8233761499683396, -319.9446178456882421 ) ) ;
#74343 =( NAMED_UNIT ( * ) SI_UNIT ( $, .STERADIAN. ) SOLID_ANGLE_UNIT ( ) );
#74344 = CARTESIAN_POINT ( 'NONE',  ( -1.773587678670080603, -278.1096710169149446, -337.8712441191687503 ) ) ;
#74345 = CARTESIAN_POINT ( 'NONE',  ( -6.998514795304313196, -282.9805209788415823, -207.2794874003663779 ) ) ;
#74346 = ORIENTED_EDGE ( 'NONE', *, *, #57468, .T. ) ;
#74347 = VERTEX_POINT ( 'NONE', #10110 ) ;
#74348 = CARTESIAN_POINT ( 'NONE',  ( -110.5383651108679430, -298.3424059769417340, -286.7088667224956566 ) ) ;
#74349 = CARTESIAN_POINT ( 'NONE',  ( -10.59857451505935266, -289.7747291194127115, -338.6726651190762141 ) ) ;
#74350 = CARTESIAN_POINT ( 'NONE',  ( -21.32410925686333414, -274.8659531575454480, -343.3202690396299204 ) ) ;
#74351 = CARTESIAN_POINT ( 'NONE',  ( -4.747138555727826947, -290.3888921443942763, -339.0162759747175301 ) ) ;
#74352 = CARTESIAN_POINT ( 'NONE',  ( -64.10121037084631723, -291.0422306162756172, -202.3194748939237115 ) ) ;
#74353 = CARTESIAN_POINT ( 'NONE',  ( -26.15969992683964307, -288.4210817735253727, -346.4826640427768325 ) ) ;
#74354 = DIRECTION ( 'NONE',  ( 0.5370370370370571855, -0.000000000000000000, 0.8435586647355706180 ) ) ;
#74355 = CARTESIAN_POINT ( 'NONE',  ( -110.2922948431506285, -282.8020485770121013, -281.8542908167387964 ) ) ;
#74356 = CARTESIAN_POINT ( 'NONE',  ( -109.6357122242981035, -292.6320679111305481, -253.4402205839576538 ) ) ;
#74357 = CARTESIAN_POINT ( 'NONE',  ( -57.56625575297894670, -284.2662901310447978, -199.4442311161974146 ) ) ;
#74358 = CARTESIAN_POINT ( 'NONE',  ( 9.578597816045999025, -282.0281943631513855, -213.7286431888898335 ) ) ;
#74359 = CARTESIAN_POINT ( 'NONE',  ( 37.79073451879185086, -288.2950721807467289, -254.5514875830503456 ) ) ;
#74360 = CARTESIAN_POINT ( 'NONE',  ( -107.8780378778167091, -278.7931810922888758, -289.4035311347136599 ) ) ;
#74361 = CARTESIAN_POINT ( 'NONE',  ( -71.97892723770681300, -290.3994350421806416, -202.0218469895243629 ) ) ;
#74362 = CARTESIAN_POINT ( 'NONE',  ( 38.62437946567852265, -288.2091809579479218, -258.7274406370387396 ) ) ;
#74363 = CARTESIAN_POINT ( 'NONE',  ( 38.72378295961302541, -287.8987456826200173, -258.7162333983712870 ) ) ;
#74364 = CARTESIAN_POINT ( 'NONE',  ( -110.3186946369728503, -284.6755760802865325, -273.6402521901212026 ) ) ;
#74365 = ORIENTED_EDGE ( 'NONE', *, *, #5214, .T. ) ;
#74366 = CARTESIAN_POINT ( 'NONE',  ( 194.2870706637142177, 27.48493576247232539, 14.58823529411773734 ) ) ;
#74367 = CARTESIAN_POINT ( 'NONE',  ( 1.053372854503991762, -294.4188834145718943, -204.9855999183268693 ) ) ;
#74368 = CARTESIAN_POINT ( 'NONE',  ( 15.12822800443399629, -293.0147362738269976, -326.0406017586187772 ) ) ;
#74369 = CARTESIAN_POINT ( 'NONE',  ( 20.19991521567041204, -275.2481289316073685, -315.6844109011823321 ) ) ;
#74370 = CARTESIAN_POINT ( 'NONE',  ( -33.33274563387125511, -297.4497003231595613, -193.4634797602432457 ) ) ;
#74371 = CARTESIAN_POINT ( 'NONE',  ( 35.98726964839713105, -291.9299183629871663, -262.5474586246740500 ) ) ;
#74372 = CARTESIAN_POINT ( 'NONE',  ( -109.1527491887405148, -295.0258693783389390, -252.3887151296896434 ) ) ;
#74373 = CARTESIAN_POINT ( 'NONE',  ( -41.63130488942617546, -293.2021424450839504, -197.0393842864601481 ) ) ;
#74374 = CARTESIAN_POINT ( 'NONE',  ( 6.257771624124649712, -295.5244042031038134, -329.3592016807214122 ) ) ;
#74375 = CARTESIAN_POINT ( 'NONE',  ( -71.26987233637623831, -293.4989171417172429, -337.4350142532647965 ) ) ;
#74376 = CARTESIAN_POINT ( 'NONE',  ( -39.87806681634610584, -300.0204473827804463, -195.4008640690309733 ) ) ;
#74377 = CARTESIAN_POINT ( 'NONE',  ( 25.14526171442063784, -287.9688531825754012, -232.1670340492557614 ) ) ;
#74378 = CARTESIAN_POINT ( 'NONE',  ( -37.10623521012158932, -279.0290699526048002, -345.7287345265697809 ) ) ;
#74379 = CARTESIAN_POINT ( 'NONE',  ( -1.666329217425129849, -275.3849138376474457, -338.1495877242780921 ) ) ;
#74380 = CARTESIAN_POINT ( 'NONE',  ( -95.00453865079963123, -272.5905489873999272, -219.4856834363111773 ) ) ;
#74381 = CARTESIAN_POINT ( 'NONE',  ( 36.86236028920718155, -279.7166023735151157, -276.9015252067166557 ) ) ;
#74382 = CARTESIAN_POINT ( 'NONE',  ( -110.6762066588404991, -276.6898771852445407, -291.0611317095278991 ) ) ;
#74383 = CARTESIAN_POINT ( 'NONE',  ( -75.93115960312972845, -294.2636857189538091, -332.9672154734957985 ) ) ;
#74384 = CARTESIAN_POINT ( 'NONE',  ( 184.7149167944524493, 8.542400036368780647, -9.000000000000001776 ) ) ;
#74385 = CARTESIAN_POINT ( 'NONE',  ( -68.33333082419196103, -274.2854179530394845, -204.1400633143957180 ) ) ;
#74386 = CARTESIAN_POINT ( 'NONE',  ( 200.4551663813218170, 64.49084098419280053, 0.000000000000000000 ) ) ;
#74387 = CIRCLE ( 'NONE', #23022, 25.00000000000000355 ) ;
#74389 = CARTESIAN_POINT ( 'NONE',  ( -40.77281631427023711, -273.8412531982428959, -197.3920957385186057 ) ) ;
#74388 = CARTESIAN_POINT ( 'NONE',  ( -112.4747267976864720, -288.4901308595647720, -276.7876747164512494 ) ) ;
#74390 = CARTESIAN_POINT ( 'NONE',  ( -111.9220341017839786, -290.3118881862409353, -289.5652037930871643 ) ) ;
#74391 = CARTESIAN_POINT ( 'NONE',  ( -110.0516000095905298, -274.7990515660800384, -251.1012609257627446 ) ) ;
#74392 = CARTESIAN_POINT ( 'NONE',  ( -109.7498088093044686, -294.3080251928071220, -289.3087866927871232 ) ) ;
#74393 = CARTESIAN_POINT ( 'NONE',  ( -88.22228193851803724, -282.9402523210974323, -328.0110311091816584 ) ) ;
#74394 = PLANE ( 'NONE',  #57800 ) ;
#74395 = VECTOR ( 'NONE', #34135, 1000.000000000000000 ) ;
#74396 = CARTESIAN_POINT ( 'NONE',  ( -14.76940321423028735, -280.7596475703621763, -341.9375972552663825 ) ) ;
#74397 = CARTESIAN_POINT ( 'NONE',  ( 200.5094052070897419, 25.16710152838790293, 9.999999999999998224 ) ) ;
#74398 = CARTESIAN_POINT ( 'NONE',  ( -102.0001744625215565, -288.8747207771212402, -305.2023618553584470 ) ) ;
#74399 = CARTESIAN_POINT ( 'NONE',  ( -64.52943918650947808, -281.5504621017586828, -339.4385551503341389 ) ) ;
#74400 = CARTESIAN_POINT ( 'NONE',  ( 197.4836817735085219, 42.27872732282709478, 11.66666666666667140 ) ) ;
#74401 = SURFACE_STYLE_FILL_AREA ( #22818 ) ;
#74402 = CARTESIAN_POINT ( 'NONE',  ( 35.90851475125332826, -291.3444308077713458, -254.1955369459573717 ) ) ;
#74403 = CARTESIAN_POINT ( 'NONE',  ( 20.38666278060578563, -276.4315573732993130, -224.5354333153332220 ) ) ;
#74404 = CARTESIAN_POINT ( 'NONE',  ( -90.15322104215556465, -284.9836560794788056, -325.9221400664249586 ) ) ;
#74406 = CARTESIAN_POINT ( 'NONE',  ( -93.25510141768785388, -285.2186397766125765, -223.4282770688946016 ) ) ;
#74405 = CARTESIAN_POINT ( 'NONE',  ( -63.04385334104880911, -271.7998665417416078, -199.3068182006708753 ) ) ;
#74407 = CARTESIAN_POINT ( 'NONE',  ( -8.491075900962258061, -278.0922386890936195, -338.0727508235528376 ) ) ;
#74408 = CARTESIAN_POINT ( 'NONE',  ( 26.91345581806242748, -276.8327314527761587, -305.4509997985492191 ) ) ;
#74409 = CARTESIAN_POINT ( 'NONE',  ( -98.15153259721294887, -285.9536657162455526, -314.3473572246385288 ) ) ;
#74410 = ORIENTED_EDGE ( 'NONE', *, *, #15525, .T. ) ;
#74411 = DIRECTION ( 'NONE',  ( -0.000000000000000000, 1.000000000000000000, -0.000000000000000000 ) ) ;
#74412 = CARTESIAN_POINT ( 'NONE',  ( -95.58288815029770547, -295.7050537587094254, -320.7294018751268254 ) ) ;
#74413 = CARTESIAN_POINT ( 'NONE',  ( 18.09565210015753678, -288.8318479730476724, -220.3565779592980789 ) ) ;
#74414 = CARTESIAN_POINT ( 'NONE',  ( 169.2494399300530290, -11.64849832608277325, -3.999999999999998224 ) ) ;
#74415 = CARTESIAN_POINT ( 'NONE',  ( -115.3288506153726871, -288.2666405000203440, -252.5284128619063608 ) ) ;
#74416 = CARTESIAN_POINT ( 'NONE',  ( -71.08614568659650956, -278.5375199563519004, -201.4930927078843297 ) ) ;
#74417 = EDGE_CURVE ( 'NONE', #11793, #81684, #33765, .T. ) ;
#74418 = CARTESIAN_POINT ( 'NONE',  ( 10.63111465465473948, -291.1018519268682212, -211.0897586184356953 ) ) ;
#74419 = CARTESIAN_POINT ( 'NONE',  ( -97.93697271887768352, -286.6513227032351097, -228.3993158769825698 ) ) ;
#74420 = CARTESIAN_POINT ( 'NONE',  ( -67.74273012630460755, -281.4077920386654341, -202.8658312501284229 ) ) ;
#74421 = CARTESIAN_POINT ( 'NONE',  ( -33.77314354132587226, -287.5214997728434128, -194.0337199024757240 ) ) ;
#74422 = CARTESIAN_POINT ( 'NONE',  ( -1.449737705333953519, -284.5764642520662164, -336.2299405513745114 ) ) ;
#74423 = CARTESIAN_POINT ( 'NONE',  ( 27.64996968141183231, -276.2611344248434762, -311.7528824236853211 ) ) ;
#74424 = CARTESIAN_POINT ( 'NONE',  ( -68.71638578619146642, -295.6578635449241119, -202.6162392225266728 ) ) ;
#74425 = CARTESIAN_POINT ( 'NONE',  ( -71.23268171405550220, -279.4503635259903263, -201.2206712695470117 ) ) ;
#74426 = CARTESIAN_POINT ( 'NONE',  ( -82.84327368075298637, -299.3449638387971845, -211.3812500184892826 ) ) ;
#74427 = CARTESIAN_POINT ( 'NONE',  ( 159.4851178187817879, 15.24064981607338432, 10.00000000000000178 ) ) ;
#74428 = CARTESIAN_POINT ( 'NONE',  ( 31.95455697924148097, -277.6233781216988064, -236.9535640164627637 ) ) ;
#74429 = CARTESIAN_POINT ( 'NONE',  ( -65.06756053210973789, -295.8334655272168447, -199.7956035823811760 ) ) ;
#74430 = FACE_OUTER_BOUND ( 'NONE', #35363, .T. ) ;
#74431 = CARTESIAN_POINT ( 'NONE',  ( -109.3478020360252998, -277.8957349463242963, -282.8088541779085858 ) ) ;
#74432 = CARTESIAN_POINT ( 'NONE',  ( -34.13525353535147389, -275.2967092788854870, -193.8253262272209554 ) ) ;
#74433 = CARTESIAN_POINT ( 'NONE',  ( 29.55096314886815989, -281.1022398462984597, -308.1283107966947910 ) ) ;
#74434 = CARTESIAN_POINT ( 'NONE',  ( 24.36657668382832043, -289.8718390835347805, -311.2506764947798956 ) ) ;
#74435 = CARTESIAN_POINT ( 'NONE',  ( -36.21675946851736683, -299.5861093703725828, -194.0541616449634432 ) ) ;
#74436 = CARTESIAN_POINT ( 'NONE',  ( -108.0028001540073603, -297.3774787112935201, -300.0790362160719269 ) ) ;
#74437 = CARTESIAN_POINT ( 'NONE',  ( -33.43763853027527233, -294.1015478300986388, -195.6168812054621924 ) ) ;
#74438 = CARTESIAN_POINT ( 'NONE',  ( 37.25436919034387984, -279.6366088427694763, -276.9369696465074639 ) ) ;
#74439 = CARTESIAN_POINT ( 'NONE',  ( -16.54233966998446448, -282.2431711383076163, -198.8859418724097452 ) ) ;
#74440 = CARTESIAN_POINT ( 'NONE',  ( -52.91290239512851912, -295.9310171204095923, -197.5149993817916538 ) ) ;
#74441 = CARTESIAN_POINT ( 'NONE',  ( -111.7395502861892567, -285.9440777478470181, -286.8353496933402198 ) ) ;
#74442 = CARTESIAN_POINT ( 'NONE',  ( -18.40686695056283995, -287.7228650447567588, -341.2355177415550997 ) ) ;
#74443 = CARTESIAN_POINT ( 'NONE',  ( -54.80317017044318106, -170.1808862240834799, -364.2540321147021132 ) ) ;
#74444 = ORIENTED_EDGE ( 'NONE', *, *, #43842, .T. ) ;
#74445 = CARTESIAN_POINT ( 'NONE',  ( -9.792831157893585825, -287.2739831076702899, -341.6328943831270522 ) ) ;
#74446 = CARTESIAN_POINT ( 'NONE',  ( -33.23322400512102348, -285.7718862169706995, -197.4058112397049740 ) ) ;
#74447 = ORIENTED_EDGE ( 'NONE', *, *, #62145, .T. ) ;
#74448 = CARTESIAN_POINT ( 'NONE',  ( -99.52971831975739292, -285.0333253451539122, -315.3290480821412984 ) ) ;
#74449 = CARTESIAN_POINT ( 'NONE',  ( 35.72006355777654107, -275.9015243157707005, -271.5810856146622427 ) ) ;
#74450 = CARTESIAN_POINT ( 'NONE',  ( -16.69655938608546109, -291.2331300248984576, -196.5013138080821307 ) ) ;
#74451 = CARTESIAN_POINT ( 'NONE',  ( 36.88444105832943620, -281.9510129430772736, -250.2166081798807227 ) ) ;
#74452 = CARTESIAN_POINT ( 'NONE',  ( 33.67201438717807349, -282.7134019369103726, -242.2928093641701821 ) ) ;
#74453 = CARTESIAN_POINT ( 'NONE',  ( -8.043001199000883616, -283.0121296584449055, -341.6028280931179779 ) ) ;
#74454 = CARTESIAN_POINT ( 'NONE',  ( -4.347568898116098701, -280.4995962340121878, -205.2289706140603585 ) ) ;
#74455 = CARTESIAN_POINT ( 'NONE',  ( -69.85430415644619018, -277.1237833571632905, -202.7746430608542312 ) ) ;
#74456 = CARTESIAN_POINT ( 'NONE',  ( -39.19203910876188957, -139.8860650072662395, -364.8865173942490401 ) ) ;
#74457 = VERTEX_POINT ( 'NONE', #26667 ) ;
#74458 = VECTOR ( 'NONE', #74032, 1000.000000000000000 ) ;
#74459 = CARTESIAN_POINT ( 'NONE',  ( 35.28238792420321346, -277.3199673538305206, -252.3120109468044916 ) ) ;
#74460 = CARTESIAN_POINT ( 'NONE',  ( 120.7794652203165384, 149.8366910277294721, -263.1582692822088916 ) ) ;
#74461 = VECTOR ( 'NONE', #93174, 1000.000000000000000 ) ;
#74462 = CARTESIAN_POINT ( 'NONE',  ( -102.6196269175759568, -296.3480666490015096, -237.3442557441241263 ) ) ;
#74463 = CARTESIAN_POINT ( 'NONE',  ( 19.37454105035772400, -292.3519631758443325, -218.3727068714760264 ) ) ;
#74464 = CARTESIAN_POINT ( 'NONE',  ( 6.721591756639591075, -59.76906970966732757, -351.2517004600837254 ) ) ;
#74465 = AXIS2_PLACEMENT_3D ( 'NONE', #38642, #60445, #75109 ) ;
#74466 = AXIS2_PLACEMENT_3D ( 'NONE', #43486, #43030, #72382 ) ;
#74468 = CARTESIAN_POINT ( 'NONE',  ( -111.1068926226098625, -288.9054794258566972, -273.9275184348696257 ) ) ;
#74467 = CARTESIAN_POINT ( 'NONE',  ( -113.3707211231467795, -271.3444403225931296, -261.8237742107333474 ) ) ;
#74469 = CARTESIAN_POINT ( 'NONE',  ( -41.07808676104863821, -296.9600592232346798, -344.5150127863178113 ) ) ;
#74470 = CARTESIAN_POINT ( 'NONE',  ( -54.89021727451788735, -287.1371130972721062, -198.9411534029229358 ) ) ;
#74471 = ORIENTED_EDGE ( 'NONE', *, *, #53345, .T. ) ;
#74472 = CARTESIAN_POINT ( 'NONE',  ( 25.52885602376467489, -295.0778638287242757, -314.4307816401636728 ) ) ;
#74473 = VECTOR ( 'NONE', #63815, 1000.000000000000000 ) ;
#74474 = CARTESIAN_POINT ( 'NONE',  ( -70.23702101035104306, -283.9901133535744293, -335.6122621973509013 ) ) ;
#74475 = CARTESIAN_POINT ( 'NONE',  ( -30.51309233569872958, -296.9307883448980192, -193.7595496953030931 ) ) ;
#74476 = CARTESIAN_POINT ( 'NONE',  ( -88.54949493537256444, -292.1580181088114614, -213.0730688708309515 ) ) ;
#74477 = CARTESIAN_POINT ( 'NONE',  ( 24.84024731074108772, -294.6465772469834974, -315.6926085923652749 ) ) ;
#74478 = CARTESIAN_POINT ( 'NONE',  ( -101.6421408529779455, -290.2462557845285005, -305.0291504973097858 ) ) ;
#74479 = ORIENTED_EDGE ( 'NONE', *, *, #46910, .F. ) ;
#74480 = CARTESIAN_POINT ( 'NONE',  ( 222.4306832106270804, -141.7221692137691775, -21.50000000000000000 ) ) ;
#74481 = CARTESIAN_POINT ( 'NONE',  ( -77.56705765604836245, -299.3787824471317549, -206.1565535717396358 ) ) ;
#74482 = CARTESIAN_POINT ( 'NONE',  ( -60.73518434341271188, -272.5502855448310129, -197.3622829227206807 ) ) ;
#74483 = CARTESIAN_POINT ( 'NONE',  ( 31.57194632179529492, -280.9417072537235640, -295.2964247345689728 ) ) ;
#74484 = ORIENTED_EDGE ( 'NONE', *, *, #23802, .F. ) ;
#74485 = CARTESIAN_POINT ( 'NONE',  ( -7.913978800448858486, -276.1844590866720068, -341.4636183676226437 ) ) ;
#74486 = CARTESIAN_POINT ( 'NONE',  ( -36.70896333572505199, -272.4601010954729645, -196.5512761557083650 ) ) ;
#74487 = CARTESIAN_POINT ( 'NONE',  ( -110.4993787953527118, -280.2481180415809945, -283.0384786833326984 ) ) ;
#74488 = CARTESIAN_POINT ( 'NONE',  ( -16.04886409159475136, -274.9135922770327056, -341.5309844200425573 ) ) ;
#74489 = CARTESIAN_POINT ( 'NONE',  ( -73.05342960719087841, -298.7726017082547969, -206.2377768113724130 ) ) ;
#74490 = CARTESIAN_POINT ( 'NONE',  ( -93.10069673837531923, -274.1667385059606659, -222.8618366217195330 ) ) ;
#74491 = CARTESIAN_POINT ( 'NONE',  ( -70.97471974561103991, -275.3745832571113965, -202.2230668747978655 ) ) ;
#74492 = CARTESIAN_POINT ( 'NONE',  ( 21.49037822252698149, -272.9275879052044047, -223.2535638062848307 ) ) ;
#74493 = CARTESIAN_POINT ( 'NONE',  ( 20.25809048107894839, -293.5697321689932551, -225.3280041404554481 ) ) ;
#74494 = CARTESIAN_POINT ( 'NONE',  ( 7.045982686199225853, -291.2449697668599811, -211.6660710887996117 ) ) ;
#74495 = LINE ( 'NONE', #67418, #74458 ) ;
#74496 = CARTESIAN_POINT ( 'NONE',  ( -80.18670820232593144, -278.1074201805467396, -334.3301169551698990 ) ) ;
#74497 = CARTESIAN_POINT ( 'NONE',  ( -29.99197734301977292, -274.3144461314024625, -197.7320495630668518 ) ) ;
#74498 = CARTESIAN_POINT ( 'NONE',  ( -94.97434894510037395, -282.5521186816318391, -320.6778752702667816 ) ) ;
#74499 = CIRCLE ( 'NONE', #32190, 24.49999999999999645 ) ;
#74500 = CARTESIAN_POINT ( 'NONE',  ( 35.33075626097016908, -295.7985704219074705, -289.5637873726855673 ) ) ;
#74501 = DIRECTION ( 'NONE',  ( -0.000000000000000000, -0.000000000000000000, 1.000000000000000000 ) ) ;
#74502 = EDGE_CURVE ( 'NONE', #72158, #16725, #42301, .T. ) ;
#74503 = CARTESIAN_POINT ( 'NONE',  ( -93.37219179858823281, -284.4159370588170077, -223.3166100077042415 ) ) ;
#74504 = CARTESIAN_POINT ( 'NONE',  ( -112.3799589767046143, -282.4853212626185268, -275.5648646428933830 ) ) ;
#74505 = CARTESIAN_POINT ( 'NONE',  ( 29.62976360303615664, -273.7175100886929613, -239.7386353479813863 ) ) ;
#74506 = CARTESIAN_POINT ( 'NONE',  ( 0.6748366296861562086, -282.5591208869451521, -205.6953921195959083 ) ) ;
#74507 = CARTESIAN_POINT ( 'NONE',  ( 30.65163309939041980, -277.1270872422682601, -298.1376447020237492 ) ) ;
#74508 = DIRECTION ( 'NONE',  ( 0.6522365350567651543, -0.2069344830099842103, -0.7292226148979034095 ) ) ;
#74509 = CARTESIAN_POINT ( 'NONE',  ( 193.9646936176698375, 19.99999999999999645, 15.00000000000039080 ) ) ;
#74510 = CARTESIAN_POINT ( 'NONE',  ( -73.54660511883022878, -271.9802241836293319, -203.2528950018933642 ) ) ;
#74511 = CARTESIAN_POINT ( 'NONE',  ( -48.20328226370995850, -279.1900778561374068, -344.7915089576744094 ) ) ;
#74512 = FACE_OUTER_BOUND ( 'NONE', #53655, .T. ) ;
#74513 = CARTESIAN_POINT ( 'NONE',  ( -43.57237465170776858, -287.8943063226583376, -195.0061790519320084 ) ) ;
#74514 = CARTESIAN_POINT ( 'NONE',  ( -46.33728359802502439, -287.1659958044081122, -344.8709239999969327 ) ) ;
#74515 = CARTESIAN_POINT ( 'NONE',  ( 113.5000000000000568, -190.7866584945343220, -490.8867980474134356 ) ) ;
#74516 = CARTESIAN_POINT ( 'NONE',  ( -100.2291351389269352, -295.8661852229679425, -232.4165611199517514 ) ) ;
#74517 = CARTESIAN_POINT ( 'NONE',  ( -45.52169314129997701, -287.2964876897261206, -344.1442677779785413 ) ) ;
#74518 = CARTESIAN_POINT ( 'NONE',  ( 196.7899183121812712, 289.3460118731243824, -81.74456998406768093 ) ) ;
#74519 = DIRECTION ( 'NONE',  ( 0.000000000000000000, 0.000000000000000000, 1.000000000000000000 ) ) ;
#74520 = CARTESIAN_POINT ( 'NONE',  ( 29.74383084652408371, -286.5079753812884178, -306.8341827236661175 ) ) ;
#74521 = CARTESIAN_POINT ( 'NONE',  ( -10.66781026394506959, -284.2986247113133800, -339.2262223411310629 ) ) ;
#74522 = CARTESIAN_POINT ( 'NONE',  ( -37.33711657186668731, -281.2919249635348820, -346.3606807609200473 ) ) ;
#74523 = CARTESIAN_POINT ( 'NONE',  ( -107.0016159787469689, -290.8419565030084186, -248.4902171929243764 ) ) ;
#74524 = AXIS2_PLACEMENT_3D ( 'NONE', #17920, #54820, #84630 ) ;
#74525 = CARTESIAN_POINT ( 'NONE',  ( -5.318355093415077839, -281.9073318073209862, -204.1049462552673219 ) ) ;
#74526 = CARTESIAN_POINT ( 'NONE',  ( -4.746056831878517457, -283.4142233113976204, -335.8601696216384767 ) ) ;
#74527 = ADVANCED_FACE ( 'NONE', ( #33290 ), #83465, .T. ) ;
#74528 = CARTESIAN_POINT ( 'NONE',  ( -86.29633191721167407, -291.7070242071380335, -327.7170751631025496 ) ) ;
#74529 = AXIS2_PLACEMENT_3D ( 'NONE', #41891, #35752, #5937 ) ;
#74530 = CARTESIAN_POINT ( 'NONE',  ( -65.54398275188748357, -297.8602344018348731, -198.6547647197295987 ) ) ;
#74531 = ORIENTED_EDGE ( 'NONE', *, *, #23350, .T. ) ;
#74532 = TOROIDAL_SURFACE ( 'NONE', #21620, 1.000000000000000000, 0.5000000000000000000 ) ;
#74533 = CARTESIAN_POINT ( 'NONE',  ( 34.99953025153173769, -285.9115961641270474, -292.2248193765338442 ) ) ;
#74534 = CARTESIAN_POINT ( 'NONE',  ( 30.54306557180798265, -276.0231117972085144, -306.8145663582024554 ) ) ;
#74535 = CARTESIAN_POINT ( 'NONE',  ( -5.359256051990131553, -294.4549278816123206, -202.9009752452699615 ) ) ;
#74536 = FACE_OUTER_BOUND ( 'NONE', #87017, .T. ) ;
#74537 = CARTESIAN_POINT ( 'NONE',  ( -4.829096099716510437, -288.9805209788416391, -202.7746430608542312 ) ) ;
#74538 = AXIS2_PLACEMENT_3D ( 'NONE', #46902, #61161, #61616 ) ;
#74539 = CARTESIAN_POINT ( 'NONE',  ( -38.54185504977358079, -275.0670126259199151, -345.5182071940267292 ) ) ;
#74540 = CARTESIAN_POINT ( 'NONE',  ( 209.8744251295252354, 28.03846817292548366, 15.00000000000000000 ) ) ;
#74541 = CARTESIAN_POINT ( 'NONE',  ( -62.56086652396250258, -296.1292289337201282, -198.4553876069790022 ) ) ;
#74542 = CARTESIAN_POINT ( 'NONE',  ( -109.2111646212260894, -292.3718225183703225, -253.5363135654050666 ) ) ;
#74543 = CARTESIAN_POINT ( 'NONE',  ( -24.57048249866506495, -273.5678994651693756, -198.3317608097948437 ) ) ;
#74544 = VECTOR ( 'NONE', #91536, 1000.000000000000000 ) ;
#74545 = CARTESIAN_POINT ( 'NONE',  ( -110.1005841813927617, -291.9183737462051340, -282.1387600919331362 ) ) ;
#74546 = CARTESIAN_POINT ( 'NONE',  ( -90.93953621487675321, -292.2088467961463607, -220.4358557993474790 ) ) ;
#74547 = CARTESIAN_POINT ( 'NONE',  ( -96.72150534157410107, -285.7010192338174761, -314.5427063229685700 ) ) ;
#74548 = CARTESIAN_POINT ( 'NONE',  ( -37.80977384094381932, -293.4716626462308113, -193.9517782229605416 ) ) ;
#74549 = CARTESIAN_POINT ( 'NONE',  ( -83.97907833090116014, -292.7419996236841939, -209.6457327047583021 ) ) ;
#74550 = CARTESIAN_POINT ( 'NONE',  ( 31.53934685475475419, -293.7089098982257838, -294.6868567051899959 ) ) ;
#74551 = CARTESIAN_POINT ( 'NONE',  ( 25.19072945925428542, -290.1118196254051895, -311.7934739645593254 ) ) ;
#74552 = CARTESIAN_POINT ( 'NONE',  ( 2.095961023225290543, -282.7060421323228070, -336.4948528492595301 ) ) ;
#74553 = CARTESIAN_POINT ( 'NONE',  ( -36.18671901538648683, -296.1463551561196823, -194.8014844089030646 ) ) ;
#74554 = CARTESIAN_POINT ( 'NONE',  ( -110.9253999516530200, -284.6723469387944760, -247.5004223799076328 ) ) ;
#74555 = VECTOR ( 'NONE', #80885, 1000.000000000000000 ) ;
#74556 = CARTESIAN_POINT ( 'NONE',  ( 36.74167249923987555, -277.6552678733329458, -279.9123376469342475 ) ) ;
#74557 = EDGE_CURVE ( 'NONE', #62353, #55580, #32830, .T. ) ;
#74558 = CARTESIAN_POINT ( 'NONE',  ( -109.3153428794948070, -283.5358074838680977, -255.9762212167196935 ) ) ;
#74559 = CARTESIAN_POINT ( 'NONE',  ( 34.77536254014806616, -285.2848066338809758, -249.5820697348338797 ) ) ;
#74560 = CARTESIAN_POINT ( 'NONE',  ( -86.31512814432410607, -275.8625889891196721, -328.2390265326181407 ) ) ;
#74561 = CARTESIAN_POINT ( 'NONE',  ( -36.19885267344637469, -282.5450916471686469, -343.4137178100369852 ) ) ;
#74562 = AXIS2_PLACEMENT_3D ( 'NONE', #64895, #93262, #27959 ) ;
#74563 = CARTESIAN_POINT ( 'NONE',  ( -86.56139755788984758, -280.5912267190093417, -211.5941817532333573 ) ) ;
#74564 = CARTESIAN_POINT ( 'NONE',  ( 20.38801330599852690, -287.2977451278451326, -320.9783517006832767 ) ) ;
#74565 = CARTESIAN_POINT ( 'NONE',  ( -0.2307040938277708231, -296.3118910867993350, -334.4567036891482985 ) ) ;
#74566 = CARTESIAN_POINT ( 'NONE',  ( -3.066506567493172408, -278.2071212142495824, -338.4318830179549309 ) ) ;
#74567 = CARTESIAN_POINT ( 'NONE',  ( 23.13856152000264998, -277.4971963590528503, -317.2378529591339316 ) ) ;
#74568 = CARTESIAN_POINT ( 'NONE',  ( -92.72802326105372117, -277.7084412444256145, -317.9148267163085961 ) ) ;
#74569 = CARTESIAN_POINT ( 'NONE',  ( -98.39281327570978419, -299.1417535791921978, -227.0853740671206253 ) ) ;
#74570 = CARTESIAN_POINT ( 'NONE',  ( 36.37782344695926895, -285.3826938240433151, -257.2051224602344064 ) ) ;
#74571 = CARTESIAN_POINT ( 'NONE',  ( -41.69428031497560738, -290.7062168319934585, -346.4497932967893234 ) ) ;
#74572 = VECTOR ( 'NONE', #49745, 1000.000000000000000 ) ;
#74573 = CARTESIAN_POINT ( 'NONE',  ( -55.89476207235227179, -294.2168998337880907, -341.3362892187378748 ) ) ;
#74574 = EDGE_LOOP ( 'NONE', ( #5627, #7486, #67637, #50765 ) ) ;
#74575 = CARTESIAN_POINT ( 'NONE',  ( 24.44288267907244006, -293.7574771579027129, -309.3759162100105300 ) ) ;
#74576 = ORIENTED_EDGE ( 'NONE', *, *, #23269, .F. ) ;
#74577 = CARTESIAN_POINT ( 'NONE',  ( -38.90005457043210413, -290.1509399999799257, -347.0361728722741645 ) ) ;
#74578 = CARTESIAN_POINT ( 'NONE',  ( -68.57435866483670850, -280.2819038159683487, -204.2671416360386445 ) ) ;
#74579 = CARTESIAN_POINT ( 'NONE',  ( -54.51253556097567099, -296.7568374629867094, -195.6171890023048263 ) ) ;
#74580 = CARTESIAN_POINT ( 'NONE',  ( 22.33130144436584175, -288.8553181748212637, -318.8838615061009136 ) ) ;
#74581 = B_SPLINE_CURVE_WITH_KNOTS ( 'NONE', 3,
 ( #71893, #59055, #35886, #21679, #22143, #93627 ),
 .UNSPECIFIED., .F., .F.,
 ( 4, 2, 4 ),
 ( 0.002740393443096640798, 0.004110592855002227590, 0.005480792266907814382 ),
 .UNSPECIFIED. ) ;
#74582 = CARTESIAN_POINT ( 'NONE',  ( -40.33368669971463305, -289.4220480538710945, -347.2948845676187375 ) ) ;
#74583 = CARTESIAN_POINT ( 'NONE',  ( -67.78931714311427470, -283.7964223850520398, -336.7315188022645884 ) ) ;
#74584 = CARTESIAN_POINT ( 'NONE',  ( -78.20562432208285486, -208.4051219816803098, -357.1155072845333507 ) ) ;
#74585 = CARTESIAN_POINT ( 'NONE',  ( 63.31788037795879376, 48.12403318353134551, -317.4058823860502230 ) ) ;
#74586 = CARTESIAN_POINT ( 'NONE',  ( 192.4389841540552766, 276.2114567146547301, -124.0227208457718575 ) ) ;
#74587 = CARTESIAN_POINT ( 'NONE',  ( -93.73702429105561862, -277.0898851584242948, -316.9872856407504287 ) ) ;
#74588 = CARTESIAN_POINT ( 'NONE',  ( -110.7013089757634958, -277.4690012365063012, -270.6255046054959053 ) ) ;
#74589 = CARTESIAN_POINT ( 'NONE',  ( -35.46747341460690706, -297.5826843317813655, -193.4228076759506223 ) ) ;
#74590 = CARTESIAN_POINT ( 'NONE',  ( -29.16725854433003917, -125.6520135956795343, -361.6366667242135122 ) ) ;
#74591 = CARTESIAN_POINT ( 'NONE',  ( -70.10512885389582038, -276.1595777985966151, -339.5119668820257175 ) ) ;
#74592 = ORIENTED_EDGE ( 'NONE', *, *, #42126, .F. ) ;
#74593 = CARTESIAN_POINT ( 'NONE',  ( -108.7214969898345203, -290.8383632685606131, -286.0049216929098179 ) ) ;
#74594 = CARTESIAN_POINT ( 'NONE',  ( -37.61736449087290168, -298.8516106606287508, -193.5230881369411406 ) ) ;
#74595 = CARTESIAN_POINT ( 'NONE',  ( 35.00421311571506067, -286.4064624732968696, -283.2960441815861827 ) ) ;
#74596 = CARTESIAN_POINT ( 'NONE',  ( 7.937813434781497257, -299.0971729166703881, -193.4189769336720985 ) ) ;
#74597 = CARTESIAN_POINT ( 'NONE',  ( -110.3743096031691806, -296.7402843377415138, -268.7350142468995386 ) ) ;
#74598 = VERTEX_POINT ( 'NONE', #24797 ) ;
#74599 = CARTESIAN_POINT ( 'NONE',  ( -43.18343439339132317, -296.0521521680024080, -430.6442049081568939 ) ) ;
#74600 = AXIS2_PLACEMENT_3D ( 'NONE', #71390, #50987, #79427 ) ;
#74601 = CARTESIAN_POINT ( 'NONE',  ( -61.91414478594938231, -279.2891147995922552, -341.8692121690097565 ) ) ;
#74602 = CARTESIAN_POINT ( 'NONE',  ( 31.01959451852300731, -281.5152315338775679, -305.6635300432021722 ) ) ;
#74603 = AXIS2_PLACEMENT_3D ( 'NONE', #53191, #88243, #8256 ) ;
#74604 = VECTOR ( 'NONE', #23250, 1000.000000000000000 ) ;
#74605 = CARTESIAN_POINT ( 'NONE',  ( -107.9196266286643890, -279.8933075908891510, -250.4907771230259641 ) ) ;
#74606 = CARTESIAN_POINT ( 'NONE',  ( -106.5061940358336017, -280.7213068450871560, -238.7661636572613304 ) ) ;
#74607 = CARTESIAN_POINT ( 'NONE',  ( -37.80818305410353020, -296.6209222390689888, -196.7733655183099586 ) ) ;
#74608 = CARTESIAN_POINT ( 'NONE',  ( 196.7679187601920034, 69.63253546436693853, -10.95639144170524837 ) ) ;
#74609 = CARTESIAN_POINT ( 'NONE',  ( -76.82364142031509857, -279.6742897887572781, -208.8990965991897042 ) ) ;
#74610 = VECTOR ( 'NONE', #82660, 1000.000000000000000 ) ;
#74611 = CARTESIAN_POINT ( 'NONE',  ( -101.0803355052465946, -273.9225869453792939, -227.3531469752605005 ) ) ;
#74612 = CARTESIAN_POINT ( 'NONE',  ( -30.05910102807533590, -276.1444902714620753, -195.7155260257193277 ) ) ;
#74613 = CARTESIAN_POINT ( 'NONE',  ( 37.64403716789804832, -273.9417716245968109, -255.6728404604151592 ) ) ;
#74614 = ORIENTED_EDGE ( 'NONE', *, *, #72732, .T. ) ;
#74615 = CARTESIAN_POINT ( 'NONE',  ( -23.40286736638519471, -122.5496321078137356, -21.50000000000000000 ) ) ;
#74616 = CIRCLE ( 'NONE', #83667, 8.500000000000007105 ) ;
#74617 = CARTESIAN_POINT ( 'NONE',  ( -69.07841855503879458, -290.8209576393734892, -204.4277702186211627 ) ) ;
#74618 = CARTESIAN_POINT ( 'NONE',  ( -109.8783495895170574, -284.2232261030928839, -244.8317766016182020 ) ) ;
#74619 = CARTESIAN_POINT ( 'NONE',  ( 22.61990526554245307, -280.3909596132652382, -313.7715161841854865 ) ) ;
#74621 = CARTESIAN_POINT ( 'NONE',  ( -82.32979142192327515, -283.5124790073619465, -211.0535650343738610 ) ) ;
#74620 = CARTESIAN_POINT ( 'NONE',  ( 34.33842590173269826, -279.9089483340678157, -253.7077564161002101 ) ) ;
#74622 = CARTESIAN_POINT ( 'NONE',  ( 14.64436009215091516, -290.3209326453991821, -324.4914692580782685 ) ) ;
#74623 = CARTESIAN_POINT ( 'NONE',  ( 33.49277846266131320, -282.5040700248410417, -251.0879014629102244 ) ) ;
#74624 = DIRECTION ( 'NONE',  ( -1.000000000000000000, 0.000000000000000000, 0.000000000000000000 ) ) ;
#74625 = CARTESIAN_POINT ( 'NONE',  ( -66.29138683552255884, -281.8247395054848994, -340.8617248607095007 ) ) ;
#74626 = CARTESIAN_POINT ( 'NONE',  ( 37.60914795013002987, -295.5871765860491678, -273.0760798960645843 ) ) ;
#74628 = CARTESIAN_POINT ( 'NONE',  ( -28.32273446397356764, -278.4048108225163105, -194.8586629213227752 ) ) ;
#74627 = CIRCLE ( 'NONE', #67138, 24.00000000000001066 ) ;
#74629 = CARTESIAN_POINT ( 'NONE',  ( -24.13369580814710957, -288.2204700384499461, -196.3110530287767119 ) ) ;
#74630 = CYLINDRICAL_SURFACE ( 'NONE', #29258, 3.000000000000000000 ) ;
#74631 = CARTESIAN_POINT ( 'NONE',  ( -87.70815786347243659, -293.2751597080068677, -214.0358649360418610 ) ) ;
#74632 = AXIS2_PLACEMENT_3D ( 'NONE', #38201, #66189, #1306 ) ;
#74633 = CARTESIAN_POINT ( 'NONE',  ( 36.08447192361377631, -273.3549442812906705, -255.0144107655211201 ) ) ;
#74634 = CARTESIAN_POINT ( 'NONE',  ( -17.77533050566854911, -288.0031866045580387, -344.6666763198309695 ) ) ;
#74635 = CARTESIAN_POINT ( 'NONE',  ( 35.99959510425156139, -292.0650627557170083, -279.0244636905586049 ) ) ;
#74636 = CARTESIAN_POINT ( 'NONE',  ( -48.18343439339133027, -261.1465603064251013, -445.1129026112485008 ) ) ;
#74637 = CARTESIAN_POINT ( 'NONE',  ( 7.870682762519501274, -275.1048211780591259, -328.3663010028109284 ) ) ;
#74638 = CARTESIAN_POINT ( 'NONE',  ( -109.3677199865572049, -294.9256108842549793, -252.3336631719506045 ) ) ;
#74639 = CARTESIAN_POINT ( 'NONE',  ( -61.40074955970969484, -290.6864848932543168, -339.8046606485491452 ) ) ;
#74640 = CARTESIAN_POINT ( 'NONE',  ( 175.2296996224749250, 250.5000000000000568, -24.99999999999999289 ) ) ;
#74641 = FACE_OUTER_BOUND ( 'NONE', #7962, .T. ) ;
#74642 = CARTESIAN_POINT ( 'NONE',  ( 31.56824404916997651, -291.6067402642401589, -237.4643740468311819 ) ) ;
#74643 = CARTESIAN_POINT ( 'NONE',  ( -11.76361223995900929, -287.9909596785881831, -201.1353869647859938 ) ) ;
#74644 = CARTESIAN_POINT ( 'NONE',  ( -82.27175383587551494, -287.8958367020495643, -331.6413291870662192 ) ) ;
#74645 = CARTESIAN_POINT ( 'NONE',  ( 29.33625009638695857, -288.5603536269874212, -239.2255134550925106 ) ) ;
#74646 = CARTESIAN_POINT ( 'NONE',  ( 169.8384340989974532, 214.5000000000000568, -24.41176470588233727 ) ) ;
#74647 = CARTESIAN_POINT ( 'NONE',  ( 26.50331050835565350, -287.8661213482336620, -234.5305204014277649 ) ) ;
#74648 = EDGE_CURVE ( 'NONE', #27540, #89945, #76395, .T. ) ;
#74649 = CARTESIAN_POINT ( 'NONE',  ( -14.26133472441101446, -296.7341899374411582, -342.0946773094296418 ) ) ;
#74650 = DIRECTION ( 'NONE',  ( -0.000000000000000000, -0.000000000000000000, -1.000000000000000000 ) ) ;
#74651 = CARTESIAN_POINT ( 'NONE',  ( -21.08328019671219167, -287.4613720088320861, -195.5034363540314075 ) ) ;
#74652 = CARTESIAN_POINT ( 'NONE',  ( -92.30367283701568226, -275.9098965787842417, -322.2869320629129106 ) ) ;
#74653 = CARTESIAN_POINT ( 'NONE',  ( -69.00279887320714067, -277.7904995120650256, -340.5418856368893898 ) ) ;
#74654 = VECTOR ( 'NONE', #28282, 1000.000000000000000 ) ;
#74655 = CARTESIAN_POINT ( 'NONE',  ( -41.00314227784342336, -279.6740111104205653, -193.4561961316451573 ) ) ;
#74656 = CARTESIAN_POINT ( 'NONE',  ( -111.7826102751215842, -274.5079294519437667, -267.6079199030569953 ) ) ;
#74657 = CARTESIAN_POINT ( 'NONE',  ( -74.52566161415958845, -283.5574047903530186, -205.2128744216350924 ) ) ;
#74658 = CARTESIAN_POINT ( 'NONE',  ( 165.2494399300530290, -11.64849832608277325, 10.00000000000000000 ) ) ;
#74659 = CARTESIAN_POINT ( 'NONE',  ( -19.21031484309129311, -278.4273714888736890, -198.3210066536638294 ) ) ;
#74660 = CARTESIAN_POINT ( 'NONE',  ( -34.57883112759889599, -281.0172621181535533, -345.3102154168523725 ) ) ;
#74661 = DIRECTION ( 'NONE',  ( -1.000000000000000000, 0.000000000000000000, 0.000000000000000000 ) ) ;
#74662 = CARTESIAN_POINT ( 'NONE',  ( 28.48795114482039992, -274.5389194072199643, -308.9508156319882914 ) ) ;
#74663 = CARTESIAN_POINT ( 'NONE',  ( -110.0437901406154850, -297.9148625708127156, -282.4074394538689035 ) ) ;
#74664 = CARTESIAN_POINT ( 'NONE',  ( -69.07116951183981257, -282.3800769487669413, -340.1947658067326188 ) ) ;
#74665 = CARTESIAN_POINT ( 'NONE',  ( -93.80262519537068044, -298.1526680131651688, -223.6985741638340244 ) ) ;
#74666 = CARTESIAN_POINT ( 'NONE',  ( -57.27746367952408235, -299.1154359049074856, -196.4423722683945641 ) ) ;
#74667 = CARTESIAN_POINT ( 'NONE',  ( -69.49644856640914270, -273.2835449454844365, -204.8007668567211113 ) ) ;
#74668 = CARTESIAN_POINT ( 'NONE',  ( 24.59875578216602676, -296.1260809153042715, -312.7412272011486607 ) ) ;
#74669 = CARTESIAN_POINT ( 'NONE',  ( 28.69745350106223114, -287.2012906447548630, -230.6624547502133566 ) ) ;
#74670 = CARTESIAN_POINT ( 'NONE',  ( -108.2462714497051337, -276.9700567163104097, -244.0978233810913025 ) ) ;
#74671 = CARTESIAN_POINT ( 'NONE',  ( -110.4302280783941228, -290.6923369096060696, -245.9648077804576474 ) ) ;
#74672 = EDGE_CURVE ( 'NONE', #17168, #10872, #4881, .T. ) ;
#74673 = CARTESIAN_POINT ( 'NONE',  ( -106.2580277091146570, -289.2819623090607593, -295.1390969273053315 ) ) ;
#74674 = CARTESIAN_POINT ( 'NONE',  ( 37.24519107588339750, -291.6590403477949280, -278.6985173699114853 ) ) ;
#74675 = ORIENTED_EDGE ( 'NONE', *, *, #90226, .F. ) ;
#74676 = CARTESIAN_POINT ( 'NONE',  ( -78.59295187722810283, -208.2960365483323244, -357.4574221067172743 ) ) ;
#74677 = CARTESIAN_POINT ( 'NONE',  ( 20.40224211447447544, -287.6899141941705693, -315.1432481485496737 ) ) ;
#74678 = DIRECTION ( 'NONE',  ( -1.000000000000000000, -0.000000000000000000, -0.000000000000000000 ) ) ;
#74679 = CARTESIAN_POINT ( 'NONE',  ( -111.6441841938612356, -285.2506829658910874, -289.6994918278102205 ) ) ;
#74680 = CARTESIAN_POINT ( 'NONE',  ( 8.719349482866910250, -291.7246806358665481, -208.8846716486493165 ) ) ;
#74681 = CARTESIAN_POINT ( 'NONE',  ( 38.18373531343226546, -283.0221040040140679, -282.6580890615919657 ) ) ;
#74682 = CARTESIAN_POINT ( 'NONE',  ( 9.907080499280741748, -282.2135394191683986, -326.0742696650880816 ) ) ;
#74683 = CARTESIAN_POINT ( 'NONE',  ( -57.38971816702794371, -297.8004735578203963, -195.9615257826633297 ) ) ;
#74684 = CIRCLE ( 'NONE', #32373, 4.499999999999990230 ) ;
#74685 = CARTESIAN_POINT ( 'NONE',  ( 21.06330951981307464, -276.2439090687676071, -225.7298909334321593 ) ) ;
#74686 = CARTESIAN_POINT ( 'NONE',  ( -44.43188863514384224, -289.9822598732267807, -196.0018478709972669 ) ) ;
#74687 = CARTESIAN_POINT ( 'NONE',  ( -19.15849291125192977, -273.0861830429902284, -199.1993213799163698 ) ) ;
#74688 = ORIENTED_EDGE ( 'NONE', *, *, #742, .F. ) ;
#74689 = CARTESIAN_POINT ( 'NONE',  ( 60.29495240252359878, -249.1689065933675238, -22.50000000000000000 ) ) ;
#74690 = CARTESIAN_POINT ( 'NONE',  ( -60.44838011321432703, -287.6703021060756100, -199.5981648483642061 ) ) ;
#74691 = AXIS2_PLACEMENT_3D ( 'NONE', #1857, #61037, #16531 ) ;
#74692 = CARTESIAN_POINT ( 'NONE',  ( -113.4696086260547503, -297.7482906846398691, -261.0856634291062051 ) ) ;
#74693 = AXIS2_PLACEMENT_3D ( 'NONE', #39147, #62363, #5066 ) ;
#74694 = CARTESIAN_POINT ( 'NONE',  ( -107.4550924571893944, -285.4790225035231401, -249.4972071373100846 ) ) ;
#74695 = CARTESIAN_POINT ( 'NONE',  ( -113.5342344903518921, -277.4882595307880138, -280.1376066241720082 ) ) ;
#74696 = CARTESIAN_POINT ( 'NONE',  ( 37.36296280046943963, -294.4325920663882812, -288.6515394447459357 ) ) ;
#74697 = CARTESIAN_POINT ( 'NONE',  ( 29.06060803431240913, -285.2103190098962955, -233.7687920394562298 ) ) ;
#74698 = CARTESIAN_POINT ( 'NONE',  ( -1.973414832039259714, -294.9299421931800680, -338.7338368609741792 ) ) ;
#74699 = CARTESIAN_POINT ( 'NONE',  ( -74.72308090585572415, -289.8978238285169482, -333.1031539349582431 ) ) ;
#74700 = CARTESIAN_POINT ( 'NONE',  ( 144.7857639756989272, -299.5541904835127980, -195.3611179825600175 ) ) ;
#74701 = CIRCLE ( 'NONE', #71754, 3.491568894204821749 ) ;
#74702 = CARTESIAN_POINT ( 'NONE',  ( 202.9738562182569694, 293.9636489450776367, -59.00000000000003553 ) ) ;
#74703 = CARTESIAN_POINT ( 'NONE',  ( 65.27003054854583297, 46.14720179368438835, -315.3780817363856954 ) ) ;
#74704 = CARTESIAN_POINT ( 'NONE',  ( -82.87778781722306576, -286.9624316419063916, -209.0647282615439337 ) ) ;
#74705 = CARTESIAN_POINT ( 'NONE',  ( -69.85430415644619018, -295.1237833571632905, -202.7746430608542312 ) ) ;
#74706 = VERTEX_POINT ( 'NONE', #3479 ) ;
#74707 = CARTESIAN_POINT ( 'NONE',  ( -107.2848808473092248, -283.1826639939407073, -292.3196594784668605 ) ) ;
#74708 = CARTESIAN_POINT ( 'NONE',  ( -109.5848754348886587, -278.5566739754412424, -243.6240218369687511 ) ) ;
#74709 = CARTESIAN_POINT ( 'NONE',  ( 34.73187271808695442, -283.8119169376137734, -290.4963737698603268 ) ) ;
#74710 = CARTESIAN_POINT ( 'NONE',  ( 47.10975143806707877, 10.86743066051956674, -330.5726880037435649 ) ) ;
#74711 = CARTESIAN_POINT ( 'NONE',  ( -95.83108803412343946, -282.4595386525951426, -319.5504424561300993 ) ) ;
#74712 = CARTESIAN_POINT ( 'NONE',  ( 10.09475186357033571, -284.7299907931557073, -212.7275355671475836 ) ) ;
#74713 = CARTESIAN_POINT ( 'NONE',  ( -82.85727382234014726, -275.2979259275561503, -209.7261570950452665 ) ) ;
#74714 = CIRCLE ( 'NONE', #6737, 2.500000000000002220 ) ;
#74715 = CARTESIAN_POINT ( 'NONE',  ( -23.50103805800856449, -295.3629202040891641, -342.1513509979731111 ) ) ;
#74716 = CARTESIAN_POINT ( 'NONE',  ( 9.173829443841141185, -291.3909643450470526, -213.3956335164136817 ) ) ;
#74717 = CARTESIAN_POINT ( 'NONE',  ( -99.56239595340080939, -278.6029753664799387, -315.5708686191259176 ) ) ;
#74718 = CARTESIAN_POINT ( 'NONE',  ( 32.09818047943307562, -275.8509181170630882, -292.8800651429879167 ) ) ;
#74719 = CARTESIAN_POINT ( 'NONE',  ( 39.39793777515723860, -274.4827912382892237, -271.1821122752888868 ) ) ;
#74720 = DIRECTION ( 'NONE',  ( 0.9998346970812742596, 0.000000000000000000, 0.01818181818181330636 ) ) ;
#74721 = CARTESIAN_POINT ( 'NONE',  ( 22.14339226843788921, -274.1785583418645160, -316.1226970260628946 ) ) ;
#74722 = CARTESIAN_POINT ( 'NONE',  ( -32.03517119519862177, -296.4117396034024523, -346.6005595134861892 ) ) ;
#74723 = DIRECTION ( 'NONE',  ( 0.000000000000000000, 0.000000000000000000, -1.000000000000000000 ) ) ;
#74724 = CARTESIAN_POINT ( 'NONE',  ( 208.4306832106271088, 0.04196010845015910040, -7.500000000000013323 ) ) ;
#74725 = CARTESIAN_POINT ( 'NONE',  ( -90.95819938144680350, -284.9158675454273180, -320.3560885456327583 ) ) ;
#74726 = CARTESIAN_POINT ( 'NONE',  ( -34.49420280291450069, -284.7769559991329515, -346.2944161767139235 ) ) ;
#74727 = CARTESIAN_POINT ( 'NONE',  ( -27.81506604715598030, -285.5249131026939722, -197.8825976396125270 ) ) ;
#74728 = CARTESIAN_POINT ( 'NONE',  ( -79.10128632590647157, -276.0253444707420840, -331.2721642435360536 ) ) ;
#74729 = CARTESIAN_POINT ( 'NONE',  ( 35.15167481083326351, -283.6199507831899496, -286.3478647997922053 ) ) ;
#74730 = CARTESIAN_POINT ( 'NONE',  ( -103.7642556815463735, -276.6028785229590312, -302.3971499174763835 ) ) ;
#74731 = CARTESIAN_POINT ( 'NONE',  ( -68.15488413106277221, -278.5462484948705537, -336.8938952929489687 ) ) ;
#74732 = CARTESIAN_POINT ( 'NONE',  ( 208.4306832106271088, -44.55766379199612004, 0.000000000000000000 ) ) ;
#74733 = CARTESIAN_POINT ( 'NONE',  ( -8.930341675178043559, -281.2173108727161548, -198.9681664298150281 ) ) ;
#74734 = CARTESIAN_POINT ( 'NONE',  ( -7.566598880602133370, -280.9244873450692239, -199.4033969406857238 ) ) ;
#74735 = ORIENTED_EDGE ( 'NONE', *, *, #55276, .F. ) ;
#74736 = VERTEX_POINT ( 'NONE', #55079 ) ;
#74737 = CARTESIAN_POINT ( 'NONE',  ( 195.1441566087187311, 40.16915684026574951, 15.11344275051338748 ) ) ;
#74738 = CARTESIAN_POINT ( 'NONE',  ( 37.07247553566636356, -289.2315434154735954, -256.1190695676899622 ) ) ;
#74739 = ADVANCED_FACE ( 'NONE', ( #91511 ), #37759, .F. ) ;
#74740 = CARTESIAN_POINT ( 'NONE',  ( -106.8570136222426754, -296.0532736473377327, -247.3921832803019356 ) ) ;
#74741 = CARTESIAN_POINT ( 'NONE',  ( -96.49513449550056521, -290.5625199193334538, -221.2064256652056997 ) ) ;
#74742 = CARTESIAN_POINT ( 'NONE',  ( 36.32215744010836289, -286.0771094970806985, -273.8114135028199030 ) ) ;
#74743 = CARTESIAN_POINT ( 'NONE',  ( 16.42919824622496705, -286.8444008847733357, -320.6757354959104873 ) ) ;
#74744 = CARTESIAN_POINT ( 'NONE',  ( -83.91159045529833804, -286.6012890637580313, -213.5643399303619674 ) ) ;
#74745 = CARTESIAN_POINT ( 'NONE',  ( -59.10951669156793997, -275.3337007887078585, -342.1327196678263363 ) ) ;
#74746 = CARTESIAN_POINT ( 'NONE',  ( 14.04898559246379364, -286.7452795909547945, -326.6948265027494358 ) ) ;
#74747 = AXIS2_PLACEMENT_3D ( 'NONE', #20606, #56119, #42829 ) ;
#74748 = CARTESIAN_POINT ( 'NONE',  ( 25.44904982844451169, -288.9990628942607032, -229.3449947107535536 ) ) ;
#74749 = CARTESIAN_POINT ( 'NONE',  ( -15.50967131853788672, -286.7702195614238576, -342.3418241194708571 ) ) ;
#74750 = CARTESIAN_POINT ( 'NONE',  ( 34.46374763106584282, -282.6835988905652925, -284.8251852979579439 ) ) ;
#74751 = CARTESIAN_POINT ( 'NONE',  ( -110.4729343686655625, -292.3290191794417865, -287.7899739523396647 ) ) ;
#74752 = CARTESIAN_POINT ( 'NONE',  ( 82.12354321084184505, -301.5426637435585349, -195.0595354636311924 ) ) ;
#74753 = DIRECTION ( 'NONE',  ( -0.000000000000000000, -0.000000000000000000, 1.000000000000000000 ) ) ;
#74754 = AXIS2_PLACEMENT_3D ( 'NONE', #40146, #76160, #41068 ) ;
#74755 = CARTESIAN_POINT ( 'NONE',  ( -111.4806179995697732, -298.6590389822279690, -255.7090317016075289 ) ) ;
#74756 = CARTESIAN_POINT ( 'NONE',  ( -19.48526938302004297, -279.4847846655044350, -199.3597877154836624 ) ) ;
#74757 = CARTESIAN_POINT ( 'NONE',  ( 20.00765610291796648, -280.2205166870371045, -318.7137670881525651 ) ) ;
#74758 = CARTESIAN_POINT ( 'NONE',  ( 39.34024589018421381, -292.8204604414252117, -276.0374227009869514 ) ) ;
#74759 = CARTESIAN_POINT ( 'NONE',  ( -35.77407587660231769, -296.4719660400812700, -196.5615479667378054 ) ) ;
#74760 = CARTESIAN_POINT ( 'NONE',  ( 34.97984321487042791, -273.8607736341372174, -288.0473391452588885 ) ) ;
#74761 = CARTESIAN_POINT ( 'NONE',  ( -35.62239879105807461, -296.3453436971453243, -343.8467374541819481 ) ) ;
#74762 = FACE_OUTER_BOUND ( 'NONE', #40367, .T. ) ;
#74763 = CARTESIAN_POINT ( 'NONE',  ( 30.04588848858884731, -297.3612107378443739, -194.0714852076413592 ) ) ;
#74765 = CARTESIAN_POINT ( 'NONE',  ( -112.6514675479462824, -294.6588674810529938, -280.8672498933675001 ) ) ;
#74764 = VECTOR ( 'NONE', #59527, 1000.000000000000000 ) ;
#74766 = TOROIDAL_SURFACE ( 'NONE', #12807, 4.499999999999990230, 0.5000000000000000000 ) ;
#74767 = CARTESIAN_POINT ( 'NONE',  ( -44.37444271633743398, -293.3868752960044048, -197.0574800988244704 ) ) ;
#74768 = DIRECTION ( 'NONE',  ( -1.000000000000000000, 0.000000000000000000, 0.000000000000000000 ) ) ;
#74769 = CARTESIAN_POINT ( 'NONE',  ( 35.45491819872999884, -294.2524986060451511, -262.5745906210389649 ) ) ;
#74770 = DIRECTION ( 'NONE',  ( 0.000000000000000000, 0.000000000000000000, -1.000000000000000000 ) ) ;
#74772 = CARTESIAN_POINT ( 'NONE',  ( -53.14937721894284550, -295.2603851840459583, -341.6810290768895015 ) ) ;
#74771 = CARTESIAN_POINT ( 'NONE',  ( -109.3467057471019217, -282.8594273508513197, -247.9666385871875320 ) ) ;
#74773 = VECTOR ( 'NONE', #24514, 1000.000000000000000 ) ;
#74774 = CARTESIAN_POINT ( 'NONE',  ( -63.91201610298173819, -283.3892812254445630, -342.6315705132724929 ) ) ;
#74775 = CARTESIAN_POINT ( 'NONE',  ( 5.350128041316613903, -282.5451605733809970, -208.0175376922692863 ) ) ;
#74776 = CARTESIAN_POINT ( 'NONE',  ( -67.17694600861631216, -285.3382476379308628, -199.3991394672190154 ) ) ;
#74777 = CARTESIAN_POINT ( 'NONE',  ( -111.7944044328310724, -288.6489923936499054, -262.8229984059123581 ) ) ;
#74778 = CARTESIAN_POINT ( 'NONE',  ( 1.722420631277537195, -281.0195122186840422, -335.9103530788731291 ) ) ;
#74779 = TOROIDAL_SURFACE ( 'NONE', #29372, 5.343514653206205445, 0.5000000000000000000 ) ;
#74780 = CARTESIAN_POINT ( 'NONE',  ( -44.05284660852944967, -284.6503451611625906, -197.1750264699281558 ) ) ;
#74781 = CARTESIAN_POINT ( 'NONE',  ( 38.48204486032361871, -286.3269807973474599, -258.7734843738759309 ) ) ;
#74782 = CARTESIAN_POINT ( 'NONE',  ( 157.4851178187871312, 69.18068689461284748, -7.000000000000000888 ) ) ;
#74783 = CARTESIAN_POINT ( 'NONE',  ( 23.60505849873323214, -295.7261133713067807, -312.0670162002215307 ) ) ;
#74784 = CARTESIAN_POINT ( 'NONE',  ( -111.8314114925341869, -280.1919948465773587, -253.3349852269796827 ) ) ;
#74786 = CARTESIAN_POINT ( 'NONE',  ( -100.8280979475137116, -278.7128352065659556, -234.2839121786687713 ) ) ;
#74785 = CARTESIAN_POINT ( 'NONE',  ( -66.31583001594192694, -293.4496828956232548, -339.9372684927440105 ) ) ;
#74787 = CARTESIAN_POINT ( 'NONE',  ( 39.60696130180528485, -293.7539912578243388, -273.1724359357992853 ) ) ;
#74788 = CIRCLE ( 'NONE', #33717, 5.343514653206204557 ) ;
#74789 = CARTESIAN_POINT ( 'NONE',  ( -106.5963192455231621, -283.0260877451271426, -240.0126481903064359 ) ) ;
#74790 = CARTESIAN_POINT ( 'NONE',  ( -64.35042687199577927, -279.4046283875090353, -340.3839925747799953 ) ) ;
#74791 = CARTESIAN_POINT ( 'NONE',  ( -9.151351836338086798, -293.7330361916733068, -337.9670199209332395 ) ) ;
#74792 = CARTESIAN_POINT ( 'NONE',  ( -48.64280816747923808, -295.9082238641929052, -196.1651650767377646 ) ) ;
#74793 = VERTEX_POINT ( 'NONE', #75452 ) ;
#74794 = CARTESIAN_POINT ( 'NONE',  ( 219.8344101925596021, 35.72494958537217968, 7.000000000000000000 ) ) ;
#74795 = CARTESIAN_POINT ( 'NONE',  ( -7.361458979222200050, -282.4271248920397284, -201.9875616782010184 ) ) ;
#74796 = CARTESIAN_POINT ( 'NONE',  ( -67.32619353486499847, -294.9639438699124412, -337.0000461916976064 ) ) ;
#74797 = CARTESIAN_POINT ( 'NONE',  ( -23.40286736638519471, -134.2391364535880598, -21.49999999999998579 ) ) ;
#74798 = CARTESIAN_POINT ( 'NONE',  ( -54.42813229853333468, -271.3380690714489560, -195.3538533559490702 ) ) ;
#74799 = CARTESIAN_POINT ( 'NONE',  ( -106.6930801248616518, -272.1743473409617877, -237.2772108291333666 ) ) ;
#74800 = CARTESIAN_POINT ( 'NONE',  ( 37.23513436521464826, -288.6517237077571281, -253.2269077795868384 ) ) ;
#74801 = CARTESIAN_POINT ( 'NONE',  ( -68.75990146923227542, -289.3104004548721377, -336.2541876411106045 ) ) ;
#74802 = CARTESIAN_POINT ( 'NONE',  ( -104.0052310366334467, -280.4941193760802776, -238.8296235851034339 ) ) ;
#74803 = CARTESIAN_POINT ( 'NONE',  ( -55.56454454115822728, -299.5747044636771648, -198.5731343292042084 ) ) ;
#74804 = ADVANCED_FACE ( 'NONE', ( #60790 ), #83948, .F. ) ;
#74805 = CARTESIAN_POINT ( 'NONE',  ( -5.371745099425447201, -279.2774097796182105, -204.2925741684289278 ) ) ;
#74806 = EDGE_LOOP ( 'NONE', ( #37992, #56528, #23610, #81307, #85416, #39031, #82750 ) ) ;
#74807 = CARTESIAN_POINT ( 'NONE',  ( -60.13777720807046023, -297.4313900022854682, -196.7795409625197749 ) ) ;
#74808 = CARTESIAN_POINT ( 'NONE',  ( 0.6228307675309368019, -294.4826844433272299, -206.3298085181062334 ) ) ;
#74809 = DIRECTION ( 'NONE',  ( -0.000000000000000000, -1.000000000000000000, -0.000000000000000000 ) ) ;
#74810 = EDGE_CURVE ( 'NONE', #35587, #67369, #93163, .T. ) ;
#74811 = CARTESIAN_POINT ( 'NONE',  ( -92.48315876940741020, -290.5195365815749255, -318.4295884558733292 ) ) ;
#74812 = DIRECTION ( 'NONE',  ( -0.000000000000000000, -1.000000000000000000, -0.000000000000000000 ) ) ;
#74813 = CARTESIAN_POINT ( 'NONE',  ( 32.20019090196863942, -291.3023189769452301, -240.2906861610345004 ) ) ;
#74814 = CARTESIAN_POINT ( 'NONE',  ( -95.30326288283188774, -296.8437399085175343, -225.9274061157932749 ) ) ;
#74815 = DIRECTION ( 'NONE',  ( 0.000000000000000000, 1.000000000000000000, 0.000000000000000000 ) ) ;
#74816 = CARTESIAN_POINT ( 'NONE',  ( -113.1226066050086416, -291.9539293853587196, -279.7384554647178447 ) ) ;
#74817 = CARTESIAN_POINT ( 'NONE',  ( -55.63300648810263738, -288.3376638359845288, -190.3683826091709363 ) ) ;
#74818 = CARTESIAN_POINT ( 'NONE',  ( 36.08793221653890981, -289.7388097344805828, -284.8537513898409088 ) ) ;
#74819 = CARTESIAN_POINT ( 'NONE',  ( 8.688526206528544904, -274.4199449389277561, -329.4292201027177498 ) ) ;
#74820 = CARTESIAN_POINT ( 'NONE',  ( 21.99936111227792424, -278.0916381359802472, -315.3050013448788604 ) ) ;
#74821 = CARTESIAN_POINT ( 'NONE',  ( -52.64232983163152824, -289.9345947764307425, -197.4576314366296685 ) ) ;
#74822 = CARTESIAN_POINT ( 'NONE',  ( -70.71224548923348152, -281.4771313512563324, -202.3411783547301468 ) ) ;
#74823 =( BOUNDED_CURVE ( )  B_SPLINE_CURVE ( 3, ( #84666, #90814, #25515, #84203 ),
 .UNSPECIFIED., .F., .F. ) 
 B_SPLINE_CURVE_WITH_KNOTS ( ( 4, 4 ),
 ( 1.570796326794894560, 2.004620063563922638 ),
 .UNSPECIFIED. ) 
 CURVE ( )  GEOMETRIC_REPRESENTATION_ITEM ( )  RATIONAL_B_SPLINE_CURVE ( ( 1.000000000000000000, 0.9843778111405747655, 0.9843778111405747655, 1.000000000000000000 ) ) 
 REPRESENTATION_ITEM ( '' )  );
#74824 = PRODUCT_DEFINITION ( 'UNKNOWN', '', #2384, #34327 ) ;
#74825 = ORIENTED_EDGE ( 'NONE', *, *, #41751, .F. ) ;
#74826 = CARTESIAN_POINT ( 'NONE',  ( 33.74733140475464666, -281.1258653181992599, -287.4508461675712852 ) ) ;
#74827 = CARTESIAN_POINT ( 'NONE',  ( -110.2600863869629535, -279.9337980626911531, -246.4353390318107131 ) ) ;
#74828 =( BOUNDED_CURVE ( )  B_SPLINE_CURVE ( 3, ( #13966, #72649, #65576, #58910 ),
 .UNSPECIFIED., .F., .F. ) 
 B_SPLINE_CURVE_WITH_KNOTS ( ( 4, 4 ),
 ( 1.570796326794902775, 2.411864997362830110 ),
 .UNSPECIFIED. ) 
 CURVE ( )  GEOMETRIC_REPRESENTATION_ITEM ( )  RATIONAL_B_SPLINE_CURVE ( ( 1.000000000000000000, 0.9419139527835183046, 0.9419139527835183046, 1.000000000000000000 ) ) 
 REPRESENTATION_ITEM ( '' )  );
#74829 = CARTESIAN_POINT ( 'NONE',  ( -71.57513316140291693, -282.2892814199485088, -338.8890741972012393 ) ) ;
#74830 = CIRCLE ( 'NONE', #53673, 203.9779373800640485 ) ;
#74831 = CARTESIAN_POINT ( 'NONE',  ( -56.85261729625045746, -278.2389087233992200, -344.6598165695388616 ) ) ;
#74832 = APPLICATION_PROTOCOL_DEFINITION ( 'draft international standard', 'automotive_design', 1998, #73513 ) ;
#74833 = CARTESIAN_POINT ( 'NONE',  ( -57.95311786317303415, -275.3108673175764238, -196.8359410454326337 ) ) ;
#74834 = CARTESIAN_POINT ( 'NONE',  ( 17.40634833298267736, -278.6948066931273047, -313.9805196606274080 ) ) ;
#74835 = ORIENTED_EDGE ( 'NONE', *, *, #37224, .T. ) ;
#74836 = CARTESIAN_POINT ( 'NONE',  ( -110.2370219626862422, -298.3250803578176260, -288.0581237040789802 ) ) ;
#74837 = CARTESIAN_POINT ( 'NONE',  ( -108.6478968032355965, -291.4082403328366695, -287.3802951183754431 ) ) ;
#74838 = CARTESIAN_POINT ( 'NONE',  ( -9.907990234155761300, -290.4588826358656775, -341.2227124832272693 ) ) ;
#74839 = CARTESIAN_POINT ( 'NONE',  ( -99.79439238707358584, -290.4232890279208732, -232.3669882039579591 ) ) ;
#74840 = CARTESIAN_POINT ( 'NONE',  ( 33.80491605301907754, -286.6857798815771616, -240.9356325364724398 ) ) ;
#74841 = LINE ( 'NONE', #2407, #89939 ) ;
#74842 = CARTESIAN_POINT ( 'NONE',  ( -68.13656191716009403, -281.8633256563235818, -337.4291200749680684 ) ) ;
#74843 = CARTESIAN_POINT ( 'NONE',  ( 35.74182787285965190, -289.5815393327949323, -283.3866090234290596 ) ) ;
#74844 = CARTESIAN_POINT ( 'NONE',  ( -111.0843622249936260, -283.0250433613940118, -270.8951863274088510 ) ) ;
#74845 = CARTESIAN_POINT ( 'NONE',  ( 34.42558532079772959, -283.0747971231998008, -286.1946336673440214 ) ) ;
#74846 = CARTESIAN_POINT ( 'NONE',  ( 39.40455292340610782, -288.4722885280886544, -268.6780092973235696 ) ) ;
#74847 = CARTESIAN_POINT ( 'NONE',  ( -106.5050140291096881, -279.3590035408768699, -246.6594963076486806 ) ) ;
#74848 = CARTESIAN_POINT ( 'NONE',  ( 29.13869172682219855, -291.8500721272266674, -232.3037111278238456 ) ) ;
#74849 = VECTOR ( 'NONE', #62873, 1000.000000000000000 ) ;
#74850 = CARTESIAN_POINT ( 'NONE',  ( 37.86334881235956829, -288.1566751647874867, -254.5380263817201296 ) ) ;
#74851 = CARTESIAN_POINT ( 'NONE',  ( -65.86038291797562749, -286.1812710007635019, -198.8892129976321996 ) ) ;
#74852 = CARTESIAN_POINT ( 'NONE',  ( -48.32658831639685815, -283.3625489863810003, -342.5298940285710501 ) ) ;
#74853 = VERTEX_POINT ( 'NONE', #53682 ) ;
#74854 = FACE_OUTER_BOUND ( 'NONE', #82232, .T. ) ;
#74855 = CARTESIAN_POINT ( 'NONE',  ( 29.79325560629463610, -294.9507952855915391, -235.1312481009662179 ) ) ;
#74856 = CARTESIAN_POINT ( 'NONE',  ( -4.728055235960237468, -293.3163640789113060, -339.5827794190420832 ) ) ;
#74857 = CARTESIAN_POINT ( 'NONE',  ( -66.90861186545470218, -276.5081731141227692, -337.3626566141915646 ) ) ;
#74858 = CARTESIAN_POINT ( 'NONE',  ( -103.7575757838931594, -296.4069320112704418, -231.4974030807680379 ) ) ;
#74859 = CARTESIAN_POINT ( 'NONE',  ( 18.48512608122216605, -292.7108980287340501, -318.4851670833149342 ) ) ;
#74860 = CARTESIAN_POINT ( 'NONE',  ( -70.90734541729170815, -295.8429429994072848, -204.3824678880895078 ) ) ;
#74861 = CARTESIAN_POINT ( 'NONE',  ( -34.85914000030421533, -293.2891090850193905, -197.0060404420374311 ) ) ;
#74862 = CARTESIAN_POINT ( 'NONE',  ( 13.10595554735863111, -293.8571499198620813, -217.1703282730994147 ) ) ;
#74863 = DIRECTION ( 'NONE',  ( -1.000000000000000000, -0.000000000000000000, -0.000000000000000000 ) ) ;
#74864 = CARTESIAN_POINT ( 'NONE',  ( 21.71506595407890572, -292.1892730876040787, -316.8825864470006763 ) ) ;
#74865 = CARTESIAN_POINT ( 'NONE',  ( -70.50246868630219410, -299.6151596358483289, -203.0762973128101692 ) ) ;
#74866 = CARTESIAN_POINT ( 'NONE',  ( 34.51735257475012730, -288.6800724584279010, -284.5569920796708061 ) ) ;
#74867 = EDGE_CURVE ( 'NONE', #33292, #76418, #20964, .T. ) ;
#74868 = ADVANCED_FACE ( 'NONE', ( #56504 ), #27132, .T. ) ;
#74869 = CARTESIAN_POINT ( 'NONE',  ( -31.55095382332170217, -278.9594100142318780, -345.5449938028233419 ) ) ;
#74870 = CARTESIAN_POINT ( 'NONE',  ( -75.15362639801952582, -276.3394030888983366, -336.9814373344150908 ) ) ;
#74871 = CARTESIAN_POINT ( 'NONE',  ( -63.51459467862234476, -273.0684028178719700, -198.0541862448038728 ) ) ;
#74872 = CARTESIAN_POINT ( 'NONE',  ( 36.95863206861560712, -279.5730284614820675, -265.8031764568244739 ) ) ;
#74873 = CARTESIAN_POINT ( 'NONE',  ( -3.103020481910842676, -275.0073822010312483, -338.4502570589072548 ) ) ;
#74874 = CARTESIAN_POINT ( 'NONE',  ( -100.5994214164760621, -294.7251764882240650, -307.8739816794015383 ) ) ;
#74875 = CARTESIAN_POINT ( 'NONE',  ( -82.73167276013245441, -275.4322983545054058, -210.5910720037404644 ) ) ;
#74876 = CARTESIAN_POINT ( 'NONE',  ( -89.32047147676225052, -273.9475478392272407, -218.9597561601831046 ) ) ;
#74877 = DIRECTION ( 'NONE',  ( -0.000000000000000000, 0.000000000000000000, -1.000000000000000000 ) ) ;
#74879 = CARTESIAN_POINT ( 'NONE',  ( 23.79465795860887667, -274.8326992061354304, -230.4694431067368612 ) ) ;
#74878 = CARTESIAN_POINT ( 'NONE',  ( -111.5478211001983340, -288.7397928283889428, -257.2516399299115051 ) ) ;
#74880 = CARTESIAN_POINT ( 'NONE',  ( 38.78557269228230098, -287.4064779481510641, -258.7131255145027922 ) ) ;
#74881 = CARTESIAN_POINT ( 'NONE',  ( 73.34442978824353077, -301.4111611709244585, -194.9687698576807122 ) ) ;
#74882 = CARTESIAN_POINT ( 'NONE',  ( -70.56022795400670589, -293.4910443592804654, -337.4174960522173023 ) ) ;
#74883 = CARTESIAN_POINT ( 'NONE',  ( -102.7859114191754202, -283.2219714936363744, -310.6254201458635293 ) ) ;
#74884 = CARTESIAN_POINT ( 'NONE',  ( -113.5000000000000568, -212.3147208684173108, -422.1836331355066818 ) ) ;
#74885 = CARTESIAN_POINT ( 'NONE',  ( -36.57589803479088175, -281.0423852956001269, -345.3697597730645725 ) ) ;
#74886 = CARTESIAN_POINT ( 'NONE',  ( 194.7272697301369533, 20.94006893973816119, -14.00764870559285136 ) ) ;
#74887 = CARTESIAN_POINT ( 'NONE',  ( -91.03927565630729646, -290.0628654286411461, -220.3055446783482978 ) ) ;
#74888 = CARTESIAN_POINT ( 'NONE',  ( -95.26341025021616815, -282.0463312047815521, -316.8134598304931160 ) ) ;
#74889 = FACE_OUTER_BOUND ( 'NONE', #76913, .T. ) ;
#74890 = DIRECTION ( 'NONE',  ( 0.000000000000000000, 0.000000000000000000, 1.000000000000000000 ) ) ;
#74891 = CARTESIAN_POINT ( 'NONE',  ( -110.3017899708364524, -288.3289069932375241, -287.7342565381404711 ) ) ;
#74892 = CARTESIAN_POINT ( 'NONE',  ( -8.719245150118359433, -275.9535910364672304, -202.3989496974445785 ) ) ;
#74893 = CARTESIAN_POINT ( 'NONE',  ( 1.903954844057003548, -283.7442703260256849, -336.1470380886358953 ) ) ;
#74895 = CARTESIAN_POINT ( 'NONE',  ( -110.3904209699347660, -284.5449207452787164, -270.9092993435457402 ) ) ;
#74894 = CARTESIAN_POINT ( 'NONE',  ( -60.40782733873081156, -271.8353223806120695, -198.3533003457394557 ) ) ;
#74896 = CARTESIAN_POINT ( 'NONE',  ( -6.009396192098829914, -278.0573377870063609, -336.9607461438483824 ) ) ;
#74897 = CARTESIAN_POINT ( 'NONE',  ( 33.40093977656022162, -276.6007997695163567, -289.0180369859816665 ) ) ;
#74898 = CARTESIAN_POINT ( 'NONE',  ( -67.06469123073790684, -285.4419288368255820, -339.2199914195545603 ) ) ;
#74899 = VERTEX_POINT ( 'NONE', #57433 ) ;
#74900 = DIRECTION ( 'NONE',  ( -0.000000000000000000, 1.000000000000000000, -0.000000000000000000 ) ) ;
#74901 = CARTESIAN_POINT ( 'NONE',  ( 24.02769098527455682, -294.0050566045246114, -316.8670083503797059 ) ) ;
#74902 = CARTESIAN_POINT ( 'NONE',  ( -16.74161553446928252, -288.2993147639137987, -198.5611211504140954 ) ) ;
#74903 = FACE_BOUND ( 'NONE', #88091, .T. ) ;
#74904 = CARTESIAN_POINT ( 'NONE',  ( -111.2586520408596868, -288.4809262143061801, -234.7283546768995564 ) ) ;
#74905 = CARTESIAN_POINT ( 'NONE',  ( -104.5161868564779297, -277.9536784139929750, -233.3600255426135277 ) ) ;
#74906 = CARTESIAN_POINT ( 'NONE',  ( -92.22162211281154498, -289.6840599446832698, -217.4217697551215736 ) ) ;
#74907 = CARTESIAN_POINT ( 'NONE',  ( -110.3013599312360213, -286.2078269172327509, -259.9882787384710241 ) ) ;
#74908 = VECTOR ( 'NONE', #82735, 1000.000000000000000 ) ;
#74909 = CARTESIAN_POINT ( 'NONE',  ( -54.16274406257657859, -279.0311278926650971, -342.4905113027081711 ) ) ;
#74910 = CARTESIAN_POINT ( 'NONE',  ( -23.90747783461152309, -287.6456743716511824, -195.0867894278129029 ) ) ;
#74911 = CARTESIAN_POINT ( 'NONE',  ( 33.24534612874339246, -283.8826458225866531, -295.8618016302511364 ) ) ;
#74912 = CARTESIAN_POINT ( 'NONE',  ( 36.06327344518754074, -276.0110979503392628, -293.6142867819698949 ) ) ;
#74913 = CARTESIAN_POINT ( 'NONE',  ( -93.05613846764882169, -295.2670227711166149, -220.6846832803128109 ) ) ;
#74914 = CARTESIAN_POINT ( 'NONE',  ( -114.0436957555450022, -278.4773857616074793, -263.0118140440122261 ) ) ;
#74915 = CARTESIAN_POINT ( 'NONE',  ( -50.22674051544231588, -299.8065700181458055, -197.0447492133035894 ) ) ;
#74916 = CARTESIAN_POINT ( 'NONE',  ( 165.4265872613447641, 2.973978534295030229, 8.999830714574057922 ) ) ;
#74917 = CARTESIAN_POINT ( 'NONE',  ( 222.8344101925596306, 35.72494958537217968, 7.000000000000000000 ) ) ;
#74918 = CARTESIAN_POINT ( 'NONE',  ( -9.648957191793451571, -296.5349061383343496, -194.6049747682645545 ) ) ;
#74919 = FACE_OUTER_BOUND ( 'NONE', #24004, .T. ) ;
#74920 = CARTESIAN_POINT ( 'NONE',  ( -108.2333168800458196, -277.8261538134307216, -288.0866214686623721 ) ) ;
#74921 = CARTESIAN_POINT ( 'NONE',  ( -32.72196284039141290, -275.3141968799232586, -193.8845356672919706 ) ) ;
#74922 = CARTESIAN_POINT ( 'NONE',  ( 39.38425109435739557, -280.6414980313104479, -272.8000975467962235 ) ) ;
#74923 = CARTESIAN_POINT ( 'NONE',  ( 26.58240732987940191, -289.8185032158293666, -307.7677501940842717 ) ) ;
#74924 = CARTESIAN_POINT ( 'NONE',  ( -67.93031800254712493, -296.9665896641506038, -340.2685153787912213 ) ) ;
#74925 = CARTESIAN_POINT ( 'NONE',  ( -86.13055729043941255, -296.9167229438172058, -329.4174989609309137 ) ) ;
#74926 = CARTESIAN_POINT ( 'NONE',  ( 21.61183459743630664, -294.9182611419863065, -224.2479829775269309 ) ) ;
#74927 = CARTESIAN_POINT ( 'NONE',  ( 17.14364192129744069, -280.2731301447624332, -321.7327876833887785 ) ) ;
#74928 = CARTESIAN_POINT ( 'NONE',  ( -32.90107183015801695, -282.0286959102318747, -196.0536821543844326 ) ) ;
#74929 = CARTESIAN_POINT ( 'NONE',  ( -106.0827918770839062, -295.0076637180445687, -241.7958155944000680 ) ) ;
#74930 = CARTESIAN_POINT ( 'NONE',  ( -103.7101143763073594, -285.6601231016950351, -307.9068764114813916 ) ) ;
#74931 = ADVANCED_FACE ( 'NONE', ( #63148 ), #77802, .F. ) ;
#74932 = CARTESIAN_POINT ( 'NONE',  ( 25.22165381111244642, -285.9482554238093144, -232.1504804965943265 ) ) ;
#74933 = CARTESIAN_POINT ( 'NONE',  ( 38.04397856571704040, -281.0907911423005885, -285.5371594570767684 ) ) ;
#74934 = CARTESIAN_POINT ( 'NONE',  ( 199.0721941440129115, 283.7445530891940280, -111.5641654068537463 ) ) ;
#74935 = VERTEX_POINT ( 'NONE', #41790 ) ;
#74936 = CARTESIAN_POINT ( 'NONE',  ( -48.79871030906058138, -287.7699243380597522, -345.9616115326194858 ) ) ;
#74937 = CARTESIAN_POINT ( 'NONE',  ( -12.01066960404757999, -286.0578619286990829, -201.8744303757225964 ) ) ;
#74938 = ORIENTED_EDGE ( 'NONE', *, *, #30297, .F. ) ;
#74939 = CARTESIAN_POINT ( 'NONE',  ( -94.16085711432764072, -284.9290770016187366, -321.8886088185550989 ) ) ;
#74940 = CARTESIAN_POINT ( 'NONE',  ( 34.39347784178688983, -275.7055030471343002, -256.7173747838750728 ) ) ;
#74941 = CARTESIAN_POINT ( 'NONE',  ( -68.19175489789289202, -290.5767579684503517, -200.1345132356656791 ) ) ;
#74942 = CARTESIAN_POINT ( 'NONE',  ( 23.32761967868425046, -282.8358363006686886, -317.6322293528140221 ) ) ;
#74943 = CARTESIAN_POINT ( 'NONE',  ( 195.1051073005702960, 20.04979238141099174, -15.17562376660917067 ) ) ;
#74944 = CARTESIAN_POINT ( 'NONE',  ( -53.63151622411897534, -281.3670620229088399, -195.7594043319838875 ) ) ;
#74945 = CARTESIAN_POINT ( 'NONE',  ( 37.96309648552013272, -281.6849037842736720, -254.3314863607673431 ) ) ;
#74946 = CARTESIAN_POINT ( 'NONE',  ( -67.68488546085839630, -289.1237833571631768, -207.2794874003663779 ) ) ;
#74947 = CARTESIAN_POINT ( 'NONE',  ( 65.37179972839517461, 47.69369081529824683, -319.0422732978356635 ) ) ;
#74948 = VERTEX_POINT ( 'NONE', #34705 ) ;
#74949 = CARTESIAN_POINT ( 'NONE',  ( 35.37389569884855689, -277.7804538021955523, -288.0920117263862039 ) ) ;
#74950 = CARTESIAN_POINT ( 'NONE',  ( -96.18930935400858573, -239.3917820358037147, -341.2764046406296075 ) ) ;
#74951 = CARTESIAN_POINT ( 'NONE',  ( -2.356358904441790969, -278.5374919569934491, -204.4082177598831151 ) ) ;
#74952 = CARTESIAN_POINT ( 'NONE',  ( -68.08283579577219768, -296.9861272120068065, -204.0234178517839609 ) ) ;
#74953 = CARTESIAN_POINT ( 'NONE',  ( 29.51808526316253278, -293.5558047644756812, -308.5383472440107653 ) ) ;
#74954 = DIRECTION ( 'NONE',  ( -0.8571673007021122226, 1.049727191138618696E-16, 0.5150380749100541555 ) ) ;
#74956 = CARTESIAN_POINT ( 'NONE',  ( -93.02865121654770064, -288.2683587841124222, -318.8668834992717507 ) ) ;
#74955 = CARTESIAN_POINT ( 'NONE',  ( -36.53001837626698034, -296.6368610634120841, -193.9505346561512908 ) ) ;
#74957 = CARTESIAN_POINT ( 'NONE',  ( -72.69225968962392415, -297.3858689795047781, -335.6535200827408971 ) ) ;
#74958 = CARTESIAN_POINT ( 'NONE',  ( 2.701783047342122934, -287.9169486293366162, -208.7351256373478350 ) ) ;
#74959 = ORIENTED_EDGE ( 'NONE', *, *, #49120, .T. ) ;
#74960 = CARTESIAN_POINT ( 'NONE',  ( 20.19436347908770557, -293.8029380839086002, -219.5237299995925468 ) ) ;
#74961 = CARTESIAN_POINT ( 'NONE',  ( -107.0426873680625732, -284.7544289292448525, -292.2645610786594261 ) ) ;
#74962 = CARTESIAN_POINT ( 'NONE',  ( -36.53035058957745207, -296.8570283620464920, -193.7583493993183197 ) ) ;
#74963 = CARTESIAN_POINT ( 'NONE',  ( -2.138946065623450465, -293.3089572078238803, -202.0461164777274519 ) ) ;
#74964 = CARTESIAN_POINT ( 'NONE',  ( -88.61314469272407734, -291.8475827130143330, -212.9959205599886900 ) ) ;
#74965 = CARTESIAN_POINT ( 'NONE',  ( -75.86693808531906313, -289.7490311545278132, -332.3676180034215690 ) ) ;
#74966 = ORIENTED_EDGE ( 'NONE', *, *, #90748, .F. ) ;
#74967 = CARTESIAN_POINT ( 'NONE',  ( -98.93149485913795615, -299.0067802050005525, -226.2362648170815476 ) ) ;
#74968 = CARTESIAN_POINT ( 'NONE',  ( -95.71509681338280018, -272.0194528579862094, -220.7369422418896363 ) ) ;
#74969 = CARTESIAN_POINT ( 'NONE',  ( 15.98900708128109294, -281.3318678153616474, -320.6263401596224867 ) ) ;
#74970 = EDGE_LOOP ( 'NONE', ( #68882, #69720, #24398, #39963 ) ) ;
#74971 = ORIENTED_EDGE ( 'NONE', *, *, #71679, .F. ) ;
#74972 = CARTESIAN_POINT ( 'NONE',  ( -96.10624957826553327, -277.3900087657607969, -320.0428544424643746 ) ) ;
#74973 = CARTESIAN_POINT ( 'NONE',  ( -81.53393939933268086, -271.8397045178370490, -211.1912845992768268 ) ) ;
#74974 = CARTESIAN_POINT ( 'NONE',  ( -105.3943992517899204, -280.0188803207770434, -300.1494931195694562 ) ) ;
#74975 = CARTESIAN_POINT ( 'NONE',  ( -43.32995393014883945, -275.2681635241457343, -344.3544034679648007 ) ) ;
#74976 = CARTESIAN_POINT ( 'NONE',  ( -109.2707992808299480, -297.5647754325951837, -285.0296439101198303 ) ) ;
#74977 = CARTESIAN_POINT ( 'NONE',  ( -43.51386669990820621, -274.9136702676119626, -197.3355026116745137 ) ) ;
#74978 = CARTESIAN_POINT ( 'NONE',  ( -89.08022788900238709, -298.9395783275885492, -214.3471053572679352 ) ) ;
#74979 = CARTESIAN_POINT ( 'NONE',  ( -49.42999155827750002, -271.9190247064548203, -195.9291656270295618 ) ) ;
#74980 = CARTESIAN_POINT ( 'NONE',  ( 24.93035956269229914, -293.6753372697427267, -231.9755710365363086 ) ) ;
#74981 = CARTESIAN_POINT ( 'NONE',  ( 34.22502406583749490, -291.9020001822214567, -253.1730831051700079 ) ) ;
#74982 = CARTESIAN_POINT ( 'NONE',  ( 123.4306832106270946, -178.2391364535880882, 4.999999999999990230 ) ) ;
#74983 = CARTESIAN_POINT ( 'NONE',  ( -82.50508948364219464, -278.1432255321193452, -332.6491197564680533 ) ) ;
#74984 = EDGE_CURVE ( 'NONE', #43035, #22436, #86100, .T. ) ;
#74985 = CARTESIAN_POINT ( 'NONE',  ( -55.30296780347217833, -298.1480740145520372, -199.5311087887484405 ) ) ;
#74986 = AXIS2_PLACEMENT_3D ( 'NONE', #36748, #80769, #79398 ) ;
#74987 = CARTESIAN_POINT ( 'NONE',  ( 19.40639413506759325, -280.9389721845145687, -321.7509049821683789 ) ) ;
#74988 = CARTESIAN_POINT ( 'NONE',  ( 19.98632690472514639, -296.2235695314948885, -318.9772238127679316 ) ) ;
#74989 = DIRECTION ( 'NONE',  ( 0.000000000000000000, 0.000000000000000000, 1.000000000000000000 ) ) ;
#74990 = CARTESIAN_POINT ( 'NONE',  ( -53.73577489193964851, -282.4649882219028427, -341.7143434471876162 ) ) ;
#74991 = CARTESIAN_POINT ( 'NONE',  ( -65.90378027287727036, -281.4247720116724736, -339.9036388608907373 ) ) ;
#74992 = CARTESIAN_POINT ( 'NONE',  ( 24.29687438552565482, -273.5743099281897912, -230.1608561809034654 ) ) ;
#74993 = CARTESIAN_POINT ( 'NONE',  ( 35.64905448056661896, -283.7743637483688985, -287.6596787865418037 ) ) ;
#74994 = CARTESIAN_POINT ( 'NONE',  ( 184.7149167944524493, 8.542400036368780647, 9.000000000000001776 ) ) ;
#74995 = DIRECTION ( 'NONE',  ( 0.6056179655966479336, -0.7957555401921982963, 0.000000000000000000 ) ) ;
#74996 = CARTESIAN_POINT ( 'NONE',  ( -10.60898051455994029, -272.7948574946798317, -198.9481130326471998 ) ) ;
#74997 = CARTESIAN_POINT ( 'NONE',  ( -91.98333423252027785, -279.8295787475494762, -322.0528317694735279 ) ) ;
#74998 = LINE ( 'NONE', #11038, #83108 ) ;
#74999 = CARTESIAN_POINT ( 'NONE',  ( 11.13464723912138155, -288.6370904760748886, -212.3328932701232361 ) ) ;
#75000 =( NAMED_UNIT ( * ) PLANE_ANGLE_UNIT ( ) SI_UNIT ( $, .RADIAN. ) );
#75001 = CARTESIAN_POINT ( 'NONE',  ( -110.9014145276504166, -288.3633514973482193, -285.0530060899549198 ) ) ;
#75002 = DIRECTION ( 'NONE',  ( -1.000000000000000000, 0.000000000000000000, 0.000000000000000000 ) ) ;
#75003 = CARTESIAN_POINT ( 'NONE',  ( -110.7711711056071806, -295.3687492845581346, -268.7087269803420213 ) ) ;
#75004 = CARTESIAN_POINT ( 'NONE',  ( -81.15530590461534644, -287.7937389005547857, -330.3519999747874749 ) ) ;
#75005 = CARTESIAN_POINT ( 'NONE',  ( -110.2140130185358942, -271.2396475792842807, -270.3444066551136871 ) ) ;
#75006 = CARTESIAN_POINT ( 'NONE',  ( -106.8240884546824105, -294.1838755858004220, -298.5958193036719308 ) ) ;
#75007 = CARTESIAN_POINT ( 'NONE',  ( -7.211669185547437522, -287.1439547021541330, -340.4814972528461112 ) ) ;
#75008 = CARTESIAN_POINT ( 'NONE',  ( 21.95978501899401891, -282.5427527767596985, -226.4106600185252205 ) ) ;
#75009 = CARTESIAN_POINT ( 'NONE',  ( -55.48227051209320848, -281.5223412516061785, -344.1506410698469836 ) ) ;
#75010 = CARTESIAN_POINT ( 'NONE',  ( -60.25896621304476497, -291.7467374322102387, -200.9986347882887685 ) ) ;
#75011 = CARTESIAN_POINT ( 'NONE',  ( 30.55824450589305030, -282.5998743493864822, -241.9890818482705583 ) ) ;
#75012 = CARTESIAN_POINT ( 'NONE',  ( 10.02099698800581429, -283.1828960342839423, -326.1895338140733998 ) ) ;
#75013 = CARTESIAN_POINT ( 'NONE',  ( 37.93307386394651814, -289.4749126423944290, -265.8903018629110306 ) ) ;
#75014 = CARTESIAN_POINT ( 'NONE',  ( -46.13197965235344356, -298.1102525112013950, -193.8645102774957252 ) ) ;
#75015 = CARTESIAN_POINT ( 'NONE',  ( 21.73062588760889469, -276.2168232603145270, -319.7520108586359129 ) ) ;
#75016 = CARTESIAN_POINT ( 'NONE',  ( -32.06563897406375929, -294.0989051586685719, -195.8901044153024031 ) ) ;
#75017 = DIRECTION ( 'NONE',  ( 0.000000000000000000, 0.000000000000000000, 1.000000000000000000 ) ) ;
#75018 = CARTESIAN_POINT ( 'NONE',  ( -54.42813229853333468, -285.7662352645560873, -345.3683826091709648 ) ) ;
#75019 = CARTESIAN_POINT ( 'NONE',  ( 26.08775556333124257, -274.0946431784811921, -310.7905922601033240 ) ) ;
#75020 = FACE_OUTER_BOUND ( 'NONE', #89222, .T. ) ;
#75021 = CARTESIAN_POINT ( 'NONE',  ( -72.88909305817860229, -295.9894778522260026, -202.9024242050108455 ) ) ;
#75022 = CARTESIAN_POINT ( 'NONE',  ( -109.4399411817046399, -291.9459649576813831, -286.1768208103741244 ) ) ;
#75023 = CARTESIAN_POINT ( 'NONE',  ( -4.050869510497753900, -273.8518091038874331, -205.2654755580136339 ) ) ;
#75024 = CARTESIAN_POINT ( 'NONE',  ( -94.84395932248192196, -292.7176838635762124, -224.2520377888179439 ) ) ;
#75025 = CARTESIAN_POINT ( 'NONE',  ( -101.3350937672449561, -291.9800218234397562, -234.6443747098917925 ) ) ;
#75026 = CARTESIAN_POINT ( 'NONE',  ( -109.7061544568813076, -286.1093759542301882, -285.9569864571572566 ) ) ;
#75027 = CARTESIAN_POINT ( 'NONE',  ( -113.5234499958223893, -291.8947469192067388, -276.9212109880714934 ) ) ;
#75028 = CARTESIAN_POINT ( 'NONE',  ( -44.86532644363411038, -293.2741064018957218, -194.1725158200438273 ) ) ;
#75029 = CARTESIAN_POINT ( 'NONE',  ( 30.58478177080551319, -293.7447035494981833, -297.2387664234243516 ) ) ;
#75030 = CARTESIAN_POINT ( 'NONE',  ( 37.68025710328415556, -289.5249655824406432, -268.2309175286733876 ) ) ;
#75031 = CARTESIAN_POINT ( 'NONE',  ( 32.02054409016238878, -281.2885222562746321, -236.8037600104784701 ) ) ;
#75032 = CARTESIAN_POINT ( 'NONE',  ( -37.23068762374366969, -296.1333855492536600, -194.8003966492061068 ) ) ;
#75033 = CARTESIAN_POINT ( 'NONE',  ( -68.49881234312341860, -285.4872935870988613, -199.9320107437874583 ) ) ;
#75034 = CARTESIAN_POINT ( 'NONE',  ( 35.98463295030797582, -277.3518478826539422, -256.3934523764798996 ) ) ;
#75035 = CARTESIAN_POINT ( 'NONE',  ( -71.60778444644189733, -282.3104605907287237, -335.2684825200851151 ) ) ;
#75036 = CARTESIAN_POINT ( 'NONE',  ( -5.596708187631768361, -284.4695189655774357, -202.4107232842063411 ) ) ;
#75037 = CARTESIAN_POINT ( 'NONE',  ( -110.9803579279968062, -276.4645190657357716, -288.2383647405698071 ) ) ;
#75038 = CARTESIAN_POINT ( 'NONE',  ( 207.4410801934303379, 29.85817334154656422, 14.41714557868295898 ) ) ;
#75039 = CARTESIAN_POINT ( 'NONE',  ( -82.83793702502916290, -283.2011666578981703, -327.5931726714594561 ) ) ;
#75040 = CARTESIAN_POINT ( 'NONE',  ( -36.77100394507235848, -281.2642460662276562, -193.7473369856338934 ) ) ;
#75041 = CARTESIAN_POINT ( 'NONE',  ( 37.87533220225556363, -286.8033008045121051, -285.6979449421966137 ) ) ;
#75042 = CARTESIAN_POINT ( 'NONE',  ( 36.21661521024648778, -295.4247907433466480, -279.0069592076075651 ) ) ;
#75043 = CARTESIAN_POINT ( 'NONE',  ( 15.45788751321450682, -276.3839091825635705, -215.4189305574670357 ) ) ;
#75044 = CARTESIAN_POINT ( 'NONE',  ( -13.23385828139068465, -275.6740776308764111, -197.7518194496450405 ) ) ;
#75045 = CARTESIAN_POINT ( 'NONE',  ( -69.25333309265458581, -277.3173327406349244, -336.0304780688007327 ) ) ;
#75046 = CARTESIAN_POINT ( 'NONE',  ( -97.62429825329751054, -275.1358554311934199, -226.2541291272155206 ) ) ;
#75047 = CARTESIAN_POINT ( 'NONE',  ( 35.79720624615365665, -285.7564829527370307, -286.2555383435764611 ) ) ;
#75048 = AXIS2_PLACEMENT_3D ( 'NONE', #55373, #85638, #41605 ) ;
#75049 = CARTESIAN_POINT ( 'NONE',  ( -113.2123576640155846, -292.2486240136522611, -262.7374718060261785 ) ) ;
#75050 = CARTESIAN_POINT ( 'NONE',  ( 35.84421031392759005, -292.4061056126957396, -265.3086779758943976 ) ) ;
#75051 = ORIENTED_EDGE ( 'NONE', *, *, #1761, .T. ) ;
#75052 = CARTESIAN_POINT ( 'NONE',  ( 27.50726076503848816, -292.7625326869556943, -236.7947693910804503 ) ) ;
#75053 = VERTEX_POINT ( 'NONE', #63618 ) ;
#75054 = CARTESIAN_POINT ( 'NONE',  ( 5.396507794224528531, -289.5679308636480869, -334.0395137907563026 ) ) ;
#75055 = CARTESIAN_POINT ( 'NONE',  ( -22.18135550578324455, -280.9027802450719378, -198.7965567756323821 ) ) ;
#75056 = CARTESIAN_POINT ( 'NONE',  ( -87.25062962735587746, -296.2960774483836985, -212.0623382339854857 ) ) ;
#75057 = CARTESIAN_POINT ( 'NONE',  ( 12.00580347735084530, -287.3685537827529402, -211.3159110462754313 ) ) ;
#75058 = CARTESIAN_POINT ( 'NONE',  ( 22.07114813388301400, -287.2276021418553000, -221.4136180153494990 ) ) ;
#75059 = CARTESIAN_POINT ( 'NONE',  ( -107.3764512311631307, -285.1609418250956196, -249.5163859517256526 ) ) ;
#75060 = CARTESIAN_POINT ( 'NONE',  ( -48.42808399934508401, -154.7767485661955220, -365.1229883189888596 ) ) ;
#75061 = CARTESIAN_POINT ( 'NONE',  ( 200.1221584904331792, 292.9742979738146005, -82.85065899227846842 ) ) ;
#75062 = CARTESIAN_POINT ( 'NONE',  ( 84.11129044875666239, 81.79000652128765125, -298.7613687047784765 ) ) ;
#75063 = CARTESIAN_POINT ( 'NONE',  ( 3.215143990356036152, -275.6888087619737462, -331.2523663012747193 ) ) ;
#75064 = CARTESIAN_POINT ( 'NONE',  ( -97.14579705661100206, -276.8826996728543577, -312.7821710251181457 ) ) ;
#75065 = CARTESIAN_POINT ( 'NONE',  ( -33.33216815981333525, -297.6087474355353493, -193.4229804999733346 ) ) ;
#75066 = CARTESIAN_POINT ( 'NONE',  ( -75.59557456435523193, -208.9939761195755921, -354.3369844704666889 ) ) ;
#75067 = CARTESIAN_POINT ( 'NONE',  ( -25.86060984566115195, -275.5936643199162859, -346.0016021008059965 ) ) ;
#75068 = CARTESIAN_POINT ( 'NONE',  ( -68.77878093516920899, -289.9693209652417636, -336.3133612515398454 ) ) ;
#75069 = CARTESIAN_POINT ( 'NONE',  ( -31.93394254334309323, -298.9210700721320109, -193.5218773760562385 ) ) ;
#75070 = CARTESIAN_POINT ( 'NONE',  ( -114.0799253280429895, -273.2751830130413850, -264.6420974808686992 ) ) ;
#75071 = CARTESIAN_POINT ( 'NONE',  ( -38.34016387664090786, -295.2316939061437324, -343.3542894075472418 ) ) ;
#75072 = EDGE_LOOP ( 'NONE', ( #17882, #9922, #28140, #25553 ) ) ;
#75073 = CARTESIAN_POINT ( 'NONE',  ( -20.42426950876691549, -278.7568184255255233, -344.0566180169374775 ) ) ;
#75074 = EDGE_CURVE ( 'NONE', #30244, #13595, #81904, .T. ) ;
#75075 = CARTESIAN_POINT ( 'NONE',  ( 35.54876346154662770, -281.3721211855328761, -295.1540119256617913 ) ) ;
#75076 = CARTESIAN_POINT ( 'NONE',  ( -109.3442982440810880, -279.4499591290078797, -284.2060585748386075 ) ) ;
#75077 = CARTESIAN_POINT ( 'NONE',  ( -31.50543159089326650, -278.7396945082627440, -346.1752553180350560 ) ) ;
#75078 = CARTESIAN_POINT ( 'NONE',  ( -100.3923504785746843, -295.6460241302178815, -232.3148560197450934 ) ) ;
#75079 = CARTESIAN_POINT ( 'NONE',  ( 184.7149167944524493, 8.542400036368780647, 25.74970488511327815 ) ) ;
#75080 = EDGE_CURVE ( 'NONE', #24375, #610, #60431, .T. ) ;
#75081 = CARTESIAN_POINT ( 'NONE',  ( -105.2670220793525004, -278.3612027709063454, -297.1034185998467478 ) ) ;
#75082 = CARTESIAN_POINT ( 'NONE',  ( -21.39829406683040247, -275.0544505095984960, -195.1948581104310563 ) ) ;
#75083 = CARTESIAN_POINT ( 'NONE',  ( 35.47323088189300222, -286.5341576688471150, -293.8405578095191117 ) ) ;
#75084 = CARTESIAN_POINT ( 'NONE',  ( 12.61287353947355960, -276.7482455577631981, -214.3494362579301935 ) ) ;
#75085 = CARTESIAN_POINT ( 'NONE',  ( 12.30788512090503417, -274.9512057929173920, -328.4431718026235103 ) ) ;
#75086 = DIRECTION ( 'NONE',  ( -0.5505044217881672752, 0.8348322475753291450, 0.000000000000000000 ) ) ;
#75087 = CARTESIAN_POINT ( 'NONE',  ( -68.83673463839879503, -288.6743509334596069, -336.3964458666311543 ) ) ;
#75088 = ADVANCED_FACE ( 'NONE', ( #28088 ), #48419, .T. ) ;
#75089 = CARTESIAN_POINT ( 'NONE',  ( -78.46094456981056453, -284.8626585114653835, -205.3801936818713614 ) ) ;
#75090 = CARTESIAN_POINT ( 'NONE',  ( -4.395952960888336314, -280.8516643341324084, -336.6374467878439987 ) ) ;
#75092 = CARTESIAN_POINT ( 'NONE',  ( -86.66229079310933514, -283.4405736102248170, -214.5356880583871657 ) ) ;
#75091 = CARTESIAN_POINT ( 'NONE',  ( 33.88931698763983036, -280.3694859963403587, -288.8914438805327904 ) ) ;
#75093 = CARTESIAN_POINT ( 'NONE',  ( 17.52777596615658595, -290.2681200034230642, -321.5104330038002445 ) ) ;
#75094 = CARTESIAN_POINT ( 'NONE',  ( -24.82367629390176234, -281.4204964335653472, -198.0394090487811241 ) ) ;
#75095 = CARTESIAN_POINT ( 'NONE',  ( 197.0526033736561260, 285.3763917366303531, -111.7597979621280189 ) ) ;
#75096 = CARTESIAN_POINT ( 'NONE',  ( -13.68979532640991437, -281.1500305604588448, -342.7974887736113487 ) ) ;
#75097 = CARTESIAN_POINT ( 'NONE',  ( 27.84919351127164688, -296.0479111339789711, -307.5490808290019800 ) ) ;
#75098 = CARTESIAN_POINT ( 'NONE',  ( -58.99169560465021789, -278.0156349317891227, -197.5239591445619283 ) ) ;
#75099 = CARTESIAN_POINT ( 'NONE',  ( -73.37420219773780161, -285.5286868711398824, -336.3865040498762369 ) ) ;
#75100 = CARTESIAN_POINT ( 'NONE',  ( 200.9306832106270804, -199.2391364535880882, 0.000000000000000000 ) ) ;
#75101 = CARTESIAN_POINT ( 'NONE',  ( -11.66600671786804888, -294.3039262087660290, -199.2422707158225705 ) ) ;
#75102 = CARTESIAN_POINT ( 'NONE',  ( -7.978507348678490096, -274.6673593749728752, -339.3880970375254265 ) ) ;
#75103 = CARTESIAN_POINT ( 'NONE',  ( 38.13349909226820955, -286.5687254150570880, -255.9509436752776992 ) ) ;
#75104 = CARTESIAN_POINT ( 'NONE',  ( -70.56278798530524909, -290.0063903003613746, -204.4611958364363602 ) ) ;
#75105 = CARTESIAN_POINT ( 'NONE',  ( -43.46159258565068484, -256.7356084326983137, -442.5391655924274801 ) ) ;
#75106 = CARTESIAN_POINT ( 'NONE',  ( -36.47706440237539738, -275.7259521424711579, -343.8617359984473865 ) ) ;
#75107 = CARTESIAN_POINT ( 'NONE',  ( -5.024846877644730370, -292.7616979509086832, -337.2069370877067627 ) ) ;
#75108 = CARTESIAN_POINT ( 'NONE',  ( -110.2768796039921568, -291.7488928151328196, -279.4000931797045837 ) ) ;
#75109 = DIRECTION ( 'NONE',  ( 0.000000000000000000, 0.000000000000000000, 1.000000000000000000 ) ) ;
#75110 = DIRECTION ( 'NONE',  ( -0.000000000000000000, 1.000000000000000000, -0.000000000000000000 ) ) ;
#75111 = CARTESIAN_POINT ( 'NONE',  ( -1.115791215868618069, -291.0038824809078051, -203.2016713106322356 ) ) ;
#75112 = CARTESIAN_POINT ( 'NONE',  ( -92.12865823314830038, -286.8533822087449039, -220.8407847019724954 ) ) ;
#75113 = CARTESIAN_POINT ( 'NONE',  ( -86.74287878492778248, -287.9675926800250068, -328.1666967194076960 ) ) ;
#75114 = CARTESIAN_POINT ( 'NONE',  ( 36.21983522669755473, -289.0220297267323986, -273.7691624788020022 ) ) ;
#75115 = DIRECTION ( 'NONE',  ( -1.000000000000000000, 0.000000000000000000, 0.000000000000000000 ) ) ;
#75116 = CARTESIAN_POINT ( 'NONE',  ( 15.13822182214966716, -287.6195731863443825, -219.3860307436418680 ) ) ;
#75117 = CARTESIAN_POINT ( 'NONE',  ( -8.983120647694706307, -296.6631289151063697, -340.2318574784262069 ) ) ;
#75118 = DIRECTION ( 'NONE',  ( 0.000000000000000000, 0.000000000000000000, 1.000000000000000000 ) ) ;
#75119 = CARTESIAN_POINT ( 'NONE',  ( 11.81098053230759604, -287.9221272078049765, -211.5379960580004877 ) ) ;
#75120 = CARTESIAN_POINT ( 'NONE',  ( -37.15553436594755254, -275.1296553738495732, -345.9337066439591695 ) ) ;
#75121 = CARTESIAN_POINT ( 'NONE',  ( -114.0576561173024430, -278.7982106933513364, -277.3333872815952077 ) ) ;
#75122 = CARTESIAN_POINT ( 'NONE',  ( -7.541254893382253854, -280.0989923328306759, -199.3702183362086942 ) ) ;
#75123 = CARTESIAN_POINT ( 'NONE',  ( -37.17059980140709996, -300.0342024511551244, -195.7133385678558284 ) ) ;
#75124 = CARTESIAN_POINT ( 'NONE',  ( -48.18343439339133738, -271.8989017423947985, -505.6992907147873666 ) ) ;
#75125 = CARTESIAN_POINT ( 'NONE',  ( -37.25363422452094397, -284.0530614461757750, -195.3483864762255848 ) ) ;
#75126 = CARTESIAN_POINT ( 'NONE',  ( -48.18343439339134449, -272.5190275734764782, -500.7427710990145329 ) ) ;
#75127 = CARTESIAN_POINT ( 'NONE',  ( -110.0930979341945317, -276.8841374057031999, -255.5291876289126947 ) ) ;
#75128 = CARTESIAN_POINT ( 'NONE',  ( 1.047956534388809535, -280.5395511379381333, -334.7911956633159889 ) ) ;
#75129 = CARTESIAN_POINT ( 'NONE',  ( 139.6925840978351516, 15.36528803885690664, 21.50000000000000000 ) ) ;
#75130 = CARTESIAN_POINT ( 'NONE',  ( 31.22371092281886007, -274.4673064654773498, -303.9700947675825660 ) ) ;
#75131 = CARTESIAN_POINT ( 'NONE',  ( -105.4099573643679122, -298.4473858951712941, -242.1224900475620530 ) ) ;
#75132 = CARTESIAN_POINT ( 'NONE',  ( -70.34958911028151363, -282.3973219750861290, -339.5995918340052526 ) ) ;
#75133 = CARTESIAN_POINT ( 'NONE',  ( -109.0118782206890842, -297.6922083110581525, -255.2410904326320349 ) ) ;
#75134 = CARTESIAN_POINT ( 'NONE',  ( -106.0776466100415263, -298.3015003357391493, -236.7654645040389312 ) ) ;
#75135 = CARTESIAN_POINT ( 'NONE',  ( -36.73163066710183955, -273.7267430296075190, -197.3301036909300308 ) ) ;
#75136 = CARTESIAN_POINT ( 'NONE',  ( 35.39169231792075720, -295.7873720920933351, -288.6601418791511264 ) ) ;
#75137 = CARTESIAN_POINT ( 'NONE',  ( 37.82540773039051629, -287.9284466310153334, -287.1217955889143241 ) ) ;
#75138 = CARTESIAN_POINT ( 'NONE',  ( -93.86797833422095039, -277.3243317398768113, -220.2203753507405679 ) ) ;
#75139 = CARTESIAN_POINT ( 'NONE',  ( -108.7992501029185917, -290.0214358306701570, -299.0459320151213660 ) ) ;
#75140 = CARTESIAN_POINT ( 'NONE',  ( 34.75120964406034574, -286.7803240818519726, -283.2460242351291981 ) ) ;
#75141 = CARTESIAN_POINT ( 'NONE',  ( -30.84446364412297825, -290.1339811201954149, -195.5916829181566925 ) ) ;
#75142 = ORIENTED_EDGE ( 'NONE', *, *, #51451, .T. ) ;
#75143 = CARTESIAN_POINT ( 'NONE',  ( 207.9738562182569979, 291.4636489450775798, -54.00000000000000711 ) ) ;
#75144 = CARTESIAN_POINT ( 'NONE',  ( -21.12177084167196384, -288.3460269611088052, -341.5994667520130292 ) ) ;
#75145 = CARTESIAN_POINT ( 'NONE',  ( 203.6865049563636774, 300.2141583696141538, -4.993328456907190294 ) ) ;
#75146 = CARTESIAN_POINT ( 'NONE',  ( -99.59061886654667717, -284.8949282948299242, -315.3708891146958422 ) ) ;
#75147 = CARTESIAN_POINT ( 'NONE',  ( 39.37130992499004378, -292.6462375692264573, -273.1779070958779698 ) ) ;
#75148 = CARTESIAN_POINT ( 'NONE',  ( 18.78690920761983207, -282.1545319301108066, -218.3719124981581956 ) ) ;
#75149 = CARTESIAN_POINT ( 'NONE',  ( -97.53355314180242885, -283.8094717073392417, -311.7522583352538277 ) ) ;
#75150 = CARTESIAN_POINT ( 'NONE',  ( -70.72904229054118730, -297.6238744718751832, -200.9760663984699818 ) ) ;
#75151 = CARTESIAN_POINT ( 'NONE',  ( -40.81489845350044021, -275.3228678541352679, -196.9000451500173767 ) ) ;
#75152 = CARTESIAN_POINT ( 'NONE',  ( -67.19934872118521696, -289.6788351480227561, -201.9479056206777159 ) ) ;
#75153 = CARTESIAN_POINT ( 'NONE',  ( -32.65040574288002517, -272.9074813964646182, -197.1015287273976639 ) ) ;
#75154 = VERTEX_POINT ( 'NONE', #56975 ) ;
#75155 = DIRECTION ( 'NONE',  ( -1.000000000000000000, 0.000000000000000000, 0.000000000000000000 ) ) ;
#75156 = CARTESIAN_POINT ( 'NONE',  ( -104.2974026483663295, -286.0390227736058932, -303.0101445029939100 ) ) ;
#75157 = CARTESIAN_POINT ( 'NONE',  ( -4.621884663425820605, -295.7108218673145643, -339.7362274928041757 ) ) ;
#75158 = CARTESIAN_POINT ( 'NONE',  ( -73.61340645483336687, -286.2085504889698200, -206.8780575459666409 ) ) ;
#75159 = CARTESIAN_POINT ( 'NONE',  ( -48.47175576450237600, -276.2491390529971795, -346.3684008123586295 ) ) ;
#75160 = CARTESIAN_POINT ( 'NONE',  ( -19.41859543215960926, -292.9281362805288040, -195.5261913122782857 ) ) ;
#75161 = CARTESIAN_POINT ( 'NONE',  ( 17.47447081539952762, -284.9642408447560911, -217.9834899676512805 ) ) ;
#75162 = CARTESIAN_POINT ( 'NONE',  ( -47.74473749351228236, -292.2567392274605140, -194.0346617641090461 ) ) ;
#75163 = CARTESIAN_POINT ( 'NONE',  ( -109.1989692998816963, -290.7141853976572747, -283.3465080036577888 ) ) ;
#75164 = CARTESIAN_POINT ( 'NONE',  ( 140.6539576904058606, 275.0000000000000568, 11.50000000000000000 ) ) ;
#75165 = FACE_OUTER_BOUND ( 'NONE', #26599, .T. ) ;
#75166 = CARTESIAN_POINT ( 'NONE',  ( 65.43520553966946807, 46.08562840962796514, -315.4480577230399376 ) ) ;
#75167 = CARTESIAN_POINT ( 'NONE',  ( -75.77440977838452341, -287.0693869736280703, -204.3788351212604084 ) ) ;
#75168 = CARTESIAN_POINT ( 'NONE',  ( -37.30987171927208834, -277.5523547857346784, -190.3611179825600175 ) ) ;
#75169 = ORIENTED_EDGE ( 'NONE', *, *, #67180, .T. ) ;
#75170 = CARTESIAN_POINT ( 'NONE',  ( -82.99793080373400755, -282.6139369486199939, -327.7824756983355883 ) ) ;
#75171 = CARTESIAN_POINT ( 'NONE',  ( -80.21793177351976567, -277.2819247761232191, -334.3578544847962917 ) ) ;
#75172 = CARTESIAN_POINT ( 'NONE',  ( 27.15166740907138987, -284.0620442495107909, -308.4192565516710829 ) ) ;
#75173 = CARTESIAN_POINT ( 'NONE',  ( -81.69423236938992261, -220.3794719950213903, -351.4091104718835936 ) ) ;
#75174 = CARTESIAN_POINT ( 'NONE',  ( 11.10489089610397961, -280.9715107882265102, -329.5187785198529582 ) ) ;
#75175 = CARTESIAN_POINT ( 'NONE',  ( -1.372143591914971816, -284.5513449184772412, -204.8964043238619297 ) ) ;
#75176 = CARTESIAN_POINT ( 'NONE',  ( -34.82413875304405337, -299.8433936276347254, -194.3737023588105046 ) ) ;
#75177 = CARTESIAN_POINT ( 'NONE',  ( -106.0429118097728889, -296.7118090073012127, -295.3721027996700172 ) ) ;
#75178 = ORIENTED_EDGE ( 'NONE', *, *, #6569, .T. ) ;
#75179 = CARTESIAN_POINT ( 'NONE',  ( 34.43504269336288814, -292.0293064091196698, -254.5122796499099138 ) ) ;
#75180 = CARTESIAN_POINT ( 'NONE',  ( -70.24985648337967348, -278.1258464599048352, -339.8763704906940006 ) ) ;
#75181 = CARTESIAN_POINT ( 'NONE',  ( 22.28083267413327917, -274.9639657297968824, -228.2187767536633771 ) ) ;
#75182 = CARTESIAN_POINT ( 'NONE',  ( 31.57145899864639915, -274.9076861586110567, -304.1342088131229957 ) ) ;
#75183 = PLANE ( 'NONE',  #79454 ) ;
#75184 = CARTESIAN_POINT ( 'NONE',  ( -49.99709029990158626, -271.8906435319648267, -196.3846513585159528 ) ) ;
#75185 = CARTESIAN_POINT ( 'NONE',  ( -37.66810429572120711, -296.4813938062350758, -346.7841728759144075 ) ) ;
#75186 = EDGE_CURVE ( 'NONE', #1315, #53167, #59008, .T. ) ;
#75187 = CARTESIAN_POINT ( 'NONE',  ( 196.1227023549103592, 250.0000000000000568, -11.81026827902096521 ) ) ;
#75188 = CARTESIAN_POINT ( 'NONE',  ( 197.5461146819721137, 68.31320778628679591, 9.184551779176434394 ) ) ;
#75189 = CARTESIAN_POINT ( 'NONE',  ( -66.67066573470455637, -284.5252904046245703, -337.5613349114591983 ) ) ;
#75190 = CARTESIAN_POINT ( 'NONE',  ( -21.90959676427218739, -284.6171576765306099, -344.7642375212583943 ) ) ;
#75191 = CARTESIAN_POINT ( 'NONE',  ( -99.69193064015632899, -284.4270119998699897, -232.1026485640697956 ) ) ;
#75192 = CARTESIAN_POINT ( 'NONE',  ( 16.16400927475245197, -274.6768332154045993, -321.1900416037742616 ) ) ;
#75193 = CARTESIAN_POINT ( 'NONE',  ( -36.15034286070351044, -284.8974740403209012, -344.5867614710153362 ) ) ;
#75194 = CARTESIAN_POINT ( 'NONE',  ( -43.28209599835645349, -275.6084025865883405, -343.8146369557525190 ) ) ;
#75195 = CARTESIAN_POINT ( 'NONE',  ( 21.09159888046461973, -277.2512914091990410, -314.6304712809431408 ) ) ;
#75196 = CYLINDRICAL_SURFACE ( 'NONE', #10990, 24.00000000000001066 ) ;
#75197 = CARTESIAN_POINT ( 'NONE',  ( -112.5615815435449321, -279.5523904734822054, -254.6091494186943294 ) ) ;
#75198 = CARTESIAN_POINT ( 'NONE',  ( 1.337606918146148072, -281.0463607288460821, -203.7915311398326708 ) ) ;
#75199 = ORIENTED_EDGE ( 'NONE', *, *, #79173, .F. ) ;
#75200 = CARTESIAN_POINT ( 'NONE',  ( 195.1832308150864037, 40.36708659705613655, 15.06199699808708381 ) ) ;
#75201 = CARTESIAN_POINT ( 'NONE',  ( 33.68786813897401800, -289.0737900418604340, -243.9962566957020158 ) ) ;
#75202 = CARTESIAN_POINT ( 'NONE',  ( -110.2610756439923989, -295.6631948843017881, -276.9039334352452784 ) ) ;
#75203 = EDGE_CURVE ( 'NONE', #78913, #69774, #74132, .T. ) ;
#75204 = CARTESIAN_POINT ( 'NONE',  ( -113.0701926592480930, -290.0680571836127797, -257.0004216787720566 ) ) ;
#75205 = CARTESIAN_POINT ( 'NONE',  ( 0.7085943880477741930, -284.8064485845953300, -206.8179028991024779 ) ) ;
#75207 = CARTESIAN_POINT ( 'NONE',  ( -101.1893004257353965, -288.2838404942792181, -307.8981629085842542 ) ) ;
#75206 = CARTESIAN_POINT ( 'NONE',  ( -33.18738715785291760, -284.6800714410216528, -196.8390201679295899 ) ) ;
#75208 = CARTESIAN_POINT ( 'NONE',  ( -96.90600122926278459, -286.3539326375493488, -227.4534901750206188 ) ) ;
#75209 = CARTESIAN_POINT ( 'NONE',  ( -45.45914416374635181, -275.1547142853006562, -344.9722231697173243 ) ) ;
#75210 = CARTESIAN_POINT ( 'NONE',  ( 20.86461581374804553, -286.6215580877141633, -319.5390114096213665 ) ) ;
#75211 = CARTESIAN_POINT ( 'NONE',  ( 35.76426420316494159, -289.3365992337932084, -253.5555168046678034 ) ) ;
#75212 = CARTESIAN_POINT ( 'NONE',  ( 36.49421464330887943, -285.3715910766461548, -256.2797075733649308 ) ) ;
#75213 = EDGE_CURVE ( 'NONE', #74347, #87117, #35648, .T. ) ;
#75214 = CARTESIAN_POINT ( 'NONE',  ( -2.305587835448050793, -283.5177268165709279, -334.6862566555413991 ) ) ;
#75215 = CARTESIAN_POINT ( 'NONE',  ( -86.17360724881899614, -291.7272892405834455, -327.5737827586361277 ) ) ;
#75216 = CARTESIAN_POINT ( 'NONE',  ( 82.12901144365632433, -301.1131897426192268, -194.1079538098041724 ) ) ;
#75217 = CARTESIAN_POINT ( 'NONE',  ( 183.0442525570908288, 291.1800221208779931, 7.500000000000000000 ) ) ;
#75218 = CARTESIAN_POINT ( 'NONE',  ( -106.4657733041606917, -298.8705224153829931, -239.7164733156501200 ) ) ;
#75219 = CARTESIAN_POINT ( 'NONE',  ( 37.34647655466836369, -279.4572050383280839, -262.9791462903383490 ) ) ;
#75220 = CARTESIAN_POINT ( 'NONE',  ( -19.41450350732463903, -291.4741245015094933, -195.5884428077315818 ) ) ;
#75221 = CARTESIAN_POINT ( 'NONE',  ( -101.9046953734307692, -295.4353501694183706, -234.6111521316276196 ) ) ;
#75222 = CARTESIAN_POINT ( 'NONE',  ( 26.89796567893247925, -279.7521574817377541, -234.6608544840322566 ) ) ;
#75223 = CARTESIAN_POINT ( 'NONE',  ( -10.95739305308923583, -272.4785094481035230, -200.6986525670266133 ) ) ;
#75224 = CARTESIAN_POINT ( 'NONE',  ( -20.72046952621861493, -296.1496045391317011, -342.0025305447263690 ) ) ;
#75225 = CARTESIAN_POINT ( 'NONE',  ( 17.06571399127465583, -89.54582641780471874, 22.50000000000000000 ) ) ;
#75226 = CARTESIAN_POINT ( 'NONE',  ( -23.49674637501712127, -296.7023972115603101, -194.0579500639032062 ) ) ;
#75227 = CARTESIAN_POINT ( 'NONE',  ( 35.39309751281768968, -292.0737742304446556, -292.5306180513165941 ) ) ;
#75228 = CARTESIAN_POINT ( 'NONE',  ( -22.64051395442955084, -293.6693083814956822, -198.2552926939281690 ) ) ;
#75229 = CARTESIAN_POINT ( 'NONE',  ( 179.7289557593406357, 275.5000000000000568, -24.91818181818184641 ) ) ;
#75230 = CARTESIAN_POINT ( 'NONE',  ( 35.80382008721097975, -294.3961171214106116, -273.4856931472226051 ) ) ;
#75231 = DIRECTION ( 'NONE',  ( 0.000000000000000000, 1.000000000000000000, 0.000000000000000000 ) ) ;
#75233 = CARTESIAN_POINT ( 'NONE',  ( 30.58556167352163868, -293.9113567539073415, -297.2367953213710052 ) ) ;
#75232 = CARTESIAN_POINT ( 'NONE',  ( -37.34015228191829294, -281.0722095964095502, -345.7291079347724008 ) ) ;
#75234 = CARTESIAN_POINT ( 'NONE',  ( 31.07714474574143537, -282.0074994817105676, -305.6862034903373342 ) ) ;
#75235 = CARTESIAN_POINT ( 'NONE',  ( 32.97520123358409450, -283.1133696276980345, -242.5625521931111166 ) ) ;
#75236 = CARTESIAN_POINT ( 'NONE',  ( -18.18318485867174417, -285.9591214211972670, -195.7493696748659886 ) ) ;
#75237 = CARTESIAN_POINT ( 'NONE',  ( -102.7131092270129642, -289.0390828449675382, -233.8321282387747715 ) ) ;
#75238 = CARTESIAN_POINT ( 'NONE',  ( -33.11666398719405890, -281.4797592383476967, -346.5637458061077041 ) ) ;
#75239 = CARTESIAN_POINT ( 'NONE',  ( 37.98914964576849229, -286.2919313450086065, -255.9821200031829846 ) ) ;
#75240 = DIRECTION ( 'NONE',  ( 0.000000000000000000, 1.000000000000000000, 0.000000000000000000 ) ) ;
#75241 = CARTESIAN_POINT ( 'NONE',  ( -34.24747818468571126, -296.6127322976963683, -344.0962263578530838 ) ) ;
#75242 = CARTESIAN_POINT ( 'NONE',  ( 36.32245510802563615, -277.2342699753088482, -290.7126212003955175 ) ) ;
#75244 = CARTESIAN_POINT ( 'NONE',  ( -87.54208127033960807, -278.9950118524668028, -217.2628624188239428 ) ) ;
#75243 = CARTESIAN_POINT ( 'NONE',  ( 37.22807805006183912, -291.4291010117114524, -259.1587148546435628 ) ) ;
#75245 = CARTESIAN_POINT ( 'NONE',  ( 30.89793999602319019, -293.2573319643981904, -234.5763028660053919 ) ) ;
#75246 = CARTESIAN_POINT ( 'NONE',  ( -112.7134655645136121, -282.7087573052382368, -264.3382097483162738 ) ) ;
#75247 = CARTESIAN_POINT ( 'NONE',  ( -15.15634930496033839, -278.7651667279599224, -342.0591375166766852 ) ) ;
#75248 = CARTESIAN_POINT ( 'NONE',  ( 18.14287874211904494, -293.2896744372609419, -318.1805482482629372 ) ) ;
#75249 = CARTESIAN_POINT ( 'NONE',  ( -9.995406632704115779, -296.3943103766233662, -195.3704328563498223 ) ) ;
#75250 = EDGE_LOOP ( 'NONE', ( #75199, #17858, #61668, #46295, #21282 ) ) ;
#75251 = CARTESIAN_POINT ( 'NONE',  ( -56.02477538461528184, -229.5268262511776527, 21.50000000000000000 ) ) ;
#75252 = CARTESIAN_POINT ( 'NONE',  ( -68.00448871744069379, -281.6275074730502865, -202.2910477437457075 ) ) ;
#75253 = CARTESIAN_POINT ( 'NONE',  ( 34.01126211579226322, -292.8520000139972694, -254.5951841277714323 ) ) ;
#75254 = DIRECTION ( 'NONE',  ( 1.000000000000000000, 0.000000000000000000, 0.000000000000000000 ) ) ;
#75255 = CARTESIAN_POINT ( 'NONE',  ( -110.4542110544635705, -276.2666405000204009, -253.6410175316879361 ) ) ;
#75256 = CARTESIAN_POINT ( 'NONE',  ( -68.07221948050482752, -296.7173024705481339, -199.9592402143491654 ) ) ;
#75257 = CARTESIAN_POINT ( 'NONE',  ( 9.936434745182769035, -289.7317894805787546, -330.5789735285498523 ) ) ;
#75258 = CARTESIAN_POINT ( 'NONE',  ( 12.15424199531149085, -288.1740223768405826, -324.0875322261592828 ) ) ;
#75259 = CARTESIAN_POINT ( 'NONE',  ( -71.27802072453108906, -281.1157834562762901, -204.9325702088000014 ) ) ;
#75260 = CARTESIAN_POINT ( 'NONE',  ( -96.10712921652623209, -298.9368236130865739, -225.3449228262869042 ) ) ;
#75261 = CARTESIAN_POINT ( 'NONE',  ( -69.90270273723888295, -278.4083762322092639, -204.5679346886585677 ) ) ;
#75262 = ORIENTED_EDGE ( 'NONE', *, *, #13973, .F. ) ;
#75263 = CARTESIAN_POINT ( 'NONE',  ( -26.20926470230388361, -297.8546836819828059, -193.3828706296505686 ) ) ;
#75264 = CARTESIAN_POINT ( 'NONE',  ( -52.69009729901044636, -293.7742849741289888, -197.4676726259614270 ) ) ;
#75265 = CARTESIAN_POINT ( 'NONE',  ( 25.85972067148311737, -295.7189814082070711, -312.9289558919719525 ) ) ;
#75266 = DIRECTION ( 'NONE',  ( 0.000000000000000000, 0.000000000000000000, 1.000000000000000000 ) ) ;
#75267 = ADVANCED_FACE ( 'NONE', ( #93389 ), #27606, .T. ) ;
#75268 = CARTESIAN_POINT ( 'NONE',  ( -101.2167761406611532, -291.6902297003558715, -234.7062159187138377 ) ) ;
#75269 = CARTESIAN_POINT ( 'NONE',  ( 157.1811212665062101, 275.9651295423822717, 16.89756555088535350 ) ) ;
#75270 = CARTESIAN_POINT ( 'NONE',  ( 38.00051562053408816, -291.5840409800447901, -261.8879754339709507 ) ) ;
#75271 = CARTESIAN_POINT ( 'NONE',  ( -99.32937735309978677, -272.5931160627417853, -231.6892119803141270 ) ) ;
#75272 = CARTESIAN_POINT ( 'NONE',  ( -97.60007241036942105, -291.4413513588268643, -317.1760336096171500 ) ) ;
#75273 = CARTESIAN_POINT ( 'NONE',  ( -19.11405058567862625, -288.7662352645559167, -190.3538533559490702 ) ) ;
#75274 = CARTESIAN_POINT ( 'NONE',  ( 35.15855799789352432, -289.3129832592465505, -251.7692137556176704 ) ) ;
#75275 = CARTESIAN_POINT ( 'NONE',  ( -3.247226104629870491, -272.5032799758094484, -203.7314525690737241 ) ) ;
#75276 = CARTESIAN_POINT ( 'NONE',  ( 35.23229767130369083, -277.2573763744300663, -253.7413302163571984 ) ) ;
#75277 = CARTESIAN_POINT ( 'NONE',  ( -41.65224650118132388, -290.0774172856012001, -195.9951922068460135 ) ) ;
#75278 = CARTESIAN_POINT ( 'NONE',  ( -108.4551717096112640, -280.7500177086495796, -244.0718165073823513 ) ) ;
#75279 = VERTEX_POINT ( 'NONE', #20511 ) ;
#75280 = CARTESIAN_POINT ( 'NONE',  ( -32.14672447486484685, -282.3334752730351624, -343.2782277459201623 ) ) ;
#75281 = CARTESIAN_POINT ( 'NONE',  ( -113.4123183080833002, -279.7591301606798311, -260.2224168589726219 ) ) ;
#75282 = CARTESIAN_POINT ( 'NONE',  ( -3.817452920253944892, -279.2795266825058320, -201.4690018977922534 ) ) ;
#75283 = CARTESIAN_POINT ( 'NONE',  ( 172.0454967774839758, 241.8891635430174460, -177.5408160709527294 ) ) ;
#75284 = CARTESIAN_POINT ( 'NONE',  ( 23.43917387236569994, -275.8654640167657703, -223.4515018542266489 ) ) ;
#75285 = APPLICATION_PROTOCOL_DEFINITION ( 'draft international standard', 'automotive_design', 1998, #54134 ) ;
#75286 = CARTESIAN_POINT ( 'NONE',  ( -65.98508653526388912, -275.2042228488130604, -199.6203872412735620 ) ) ;
#75287 = CARTESIAN_POINT ( 'NONE',  ( 27.33386217378599881, -277.6233781216988064, -239.1787733560258573 ) ) ;
#75288 = ORIENTED_EDGE ( 'NONE', *, *, #58215, .T. ) ;
#75289 = ORIENTED_EDGE ( 'NONE', *, *, #76892, .F. ) ;
#75290 = VECTOR ( 'NONE', #62810, 1000.000000000000000 ) ;
#75291 = DIRECTION ( 'NONE',  ( 0.000000000000000000, 0.000000000000000000, -1.000000000000000000 ) ) ;
#75292 = CARTESIAN_POINT ( 'NONE',  ( -104.3245834902642315, -291.2309609334361653, -300.2776941623626499 ) ) ;
#75293 = CARTESIAN_POINT ( 'NONE',  ( -86.70884949778225348, -291.4873085994771600, -328.1957597084564782 ) ) ;
#75294 = CARTESIAN_POINT ( 'NONE',  ( -110.4085784052586234, -289.8540419052837365, -273.9056393316333811 ) ) ;
#75295 = CARTESIAN_POINT ( 'NONE',  ( 14.21030148547296257, -286.2608757155883268, -213.1764317135298654 ) ) ;
#75296 = CARTESIAN_POINT ( 'NONE',  ( 202.8019728163925492, 61.40723988820079171, 7.000000000000000000 ) ) ;
#75297 = CARTESIAN_POINT ( 'NONE',  ( 24.79310128011774594, -280.4980631039326795, -310.2759600145307672 ) ) ;
#75298 = CARTESIAN_POINT ( 'NONE',  ( -29.01138261004551921, -290.8058670193477724, -344.1274469505269735 ) ) ;
#75299 = CARTESIAN_POINT ( 'NONE',  ( -96.48969585351893841, -282.4212863938078613, -314.3181692438258210 ) ) ;
#75300 = CARTESIAN_POINT ( 'NONE',  ( 34.54407498774808261, -282.6662708677534397, -255.0146650815508451 ) ) ;
#75301 = CARTESIAN_POINT ( 'NONE',  ( 36.91984624388441460, -288.7375258160590761, -289.8044444484485780 ) ) ;
#75302 = CARTESIAN_POINT ( 'NONE',  ( -74.54251828192542462, -280.0355259030642969, -207.4214289296987488 ) ) ;
#75303 = CARTESIAN_POINT ( 'NONE',  ( -101.9745294075216009, -288.8042359777514889, -311.5757410587415279 ) ) ;
#75304 = CARTESIAN_POINT ( 'NONE',  ( -110.7747526308671127, -285.6417031317057535, -247.5601590194017376 ) ) ;
#75305 = CARTESIAN_POINT ( 'NONE',  ( -54.95661389131981167, -286.3238594502032583, -195.4662468886860722 ) ) ;
#75306 = CARTESIAN_POINT ( 'NONE',  ( -97.53114532118206625, -284.1427779865191496, -311.7557601251275514 ) ) ;
#75307 = VERTEX_POINT ( 'NONE', #11357 ) ;
#75308 = CARTESIAN_POINT ( 'NONE',  ( 194.7373591563044783, 27.48493576247233250, 14.00000000000007461 ) ) ;
#75309 = CARTESIAN_POINT ( 'NONE',  ( -42.00203842906732632, -293.8544102891200964, -194.7397801981711609 ) ) ;
#75310 = CARTESIAN_POINT ( 'NONE',  ( -16.65641623173852892, -293.4753148378163132, -344.0734252268142654 ) ) ;
#75311 = CARTESIAN_POINT ( 'NONE',  ( -35.12247642981180462, -276.0823494035944918, -343.5627811801691678 ) ) ;
#75312 = EDGE_CURVE ( 'NONE', #64758, #52349, #43846, .T. ) ;
#75313 = CARTESIAN_POINT ( 'NONE',  ( -112.5072827329021123, -295.6974813788014558, -286.5921986236854764 ) ) ;
#75314 = CARTESIAN_POINT ( 'NONE',  ( -12.00380657687494157, -290.8677333333762931, -201.1062971438530553 ) ) ;
#75315 = CARTESIAN_POINT ( 'NONE',  ( 10.93578421656968835, -292.6131472422081288, -326.4615503911931000 ) ) ;
#75316 = CARTESIAN_POINT ( 'NONE',  ( -108.8176499621582849, -291.9768338629787650, -253.6233617919739913 ) ) ;
#75317 = CARTESIAN_POINT ( 'NONE',  ( -1.115838972928507866, -293.6246253637290806, -206.6134433889496336 ) ) ;
#75318 = DIRECTION ( 'NONE',  ( 0.000000000000000000, 1.000000000000000000, 0.000000000000000000 ) ) ;
#75319 = CARTESIAN_POINT ( 'NONE',  ( -28.00151579417840964, -292.9338161732316053, -344.9972500138078431 ) ) ;
#75320 = CARTESIAN_POINT ( 'NONE',  ( -38.16888550275267278, -297.0626855024811448, -345.3691057194579344 ) ) ;
#75321 = CARTESIAN_POINT ( 'NONE',  ( 35.68753111600568673, -288.5739884109801778, -276.4891305649846913 ) ) ;
#75322 = CARTESIAN_POINT ( 'NONE',  ( 35.99704987304163240, -277.7539764534426467, -287.7325100432989871 ) ) ;
#75323 = CARTESIAN_POINT ( 'NONE',  ( -62.29124493179421052, -276.1643886034883053, -342.8431639951513716 ) ) ;
#75324 = EDGE_CURVE ( 'NONE', #90952, #85642, #63565, .T. ) ;
#75325 = CARTESIAN_POINT ( 'NONE',  ( -96.85190254110702313, -272.5556876607107029, -221.6389443325548712 ) ) ;
#75326 = CARTESIAN_POINT ( 'NONE',  ( 29.07706990278712311, -279.1831142298798341, -236.6333423517621952 ) ) ;
#75327 = CARTESIAN_POINT ( 'NONE',  ( -68.70492063670869243, -275.8574026286449339, -339.8216766797372657 ) ) ;
#75328 = EDGE_CURVE ( 'NONE', #84307, #65773, #70070, .T. ) ;
#75329 = CARTESIAN_POINT ( 'NONE',  ( -104.3933690947992403, -294.8329245121622648, -300.5740712314096186 ) ) ;
#75330 = CARTESIAN_POINT ( 'NONE',  ( -69.75615881439807708, -275.6256097503289766, -202.7135829966783263 ) ) ;
#75331 = CARTESIAN_POINT ( 'NONE',  ( -56.89685064867380504, -274.4447684151328986, -199.8704901249973602 ) ) ;
#75332 = CARTESIAN_POINT ( 'NONE',  ( 210.6909600361163371, -5.082197683525803883E-17, 7.166288341785294058 ) ) ;
#75334 = CARTESIAN_POINT ( 'NONE',  ( 20.68282252024792101, -274.7622947492533854, -226.0443253088345443 ) ) ;
#75333 = CARTESIAN_POINT ( 'NONE',  ( -68.69641587537209659, -287.4823015945534053, -338.8974120948885798 ) ) ;
#75335 = CARTESIAN_POINT ( 'NONE',  ( 39.09056570307249245, -287.6742402772570131, -280.1231841771567019 ) ) ;
#75336 = CARTESIAN_POINT ( 'NONE',  ( -99.70216693761570070, -275.1197216756281705, -228.3017489483409292 ) ) ;
#75337 = CARTESIAN_POINT ( 'NONE',  ( -104.1580704829187027, -294.9995364125176707, -236.5471354320052910 ) ) ;
#75338 = CARTESIAN_POINT ( 'NONE',  ( 15.63479333641765834, -281.5222773165192507, -326.0176536307007495 ) ) ;
#75339 = FACE_OUTER_BOUND ( 'NONE', #17996, .T. ) ;
#75340 = CARTESIAN_POINT ( 'NONE',  ( -67.10673074314206588, -277.6619532058171558, -201.4657905397364175 ) ) ;
#75341 = CARTESIAN_POINT ( 'NONE',  ( 197.4352353745718744, 215.0000000000000568, -12.47235818614446146 ) ) ;
#75342 = CARTESIAN_POINT ( 'NONE',  ( -64.20271485585210769, -290.4886574501826431, -202.0421951684783437 ) ) ;
#75343 = CARTESIAN_POINT ( 'NONE',  ( -81.37758304822348521, -281.7973128115350505, -330.1888434668369996 ) ) ;
#75344 = FACE_OUTER_BOUND ( 'NONE', #33099, .T. ) ;
#75345 = CARTESIAN_POINT ( 'NONE',  ( 191.4749582765727212, 14.19731191252289015, 10.00000000000000000 ) ) ;
#75346 = CARTESIAN_POINT ( 'NONE',  ( -52.75661796808977044, -289.8546012373262784, -196.9090188413492513 ) ) ;
#75347 = CARTESIAN_POINT ( 'NONE',  ( 23.61505529878225929, -276.5014874611289883, -228.9261539381503496 ) ) ;
#75348 = CARTESIAN_POINT ( 'NONE',  ( 22.94927417554640314, -283.6095701445305508, -317.3248361464147820 ) ) ;
#75350 = CARTESIAN_POINT ( 'NONE',  ( -56.31889993073173883, -283.3035837589264361, -340.8513008994051461 ) ) ;
#75349 = CARTESIAN_POINT ( 'NONE',  ( -46.67836583503722636, -272.0143457914076635, -195.3801812718675706 ) ) ;
#75351 = CARTESIAN_POINT ( 'NONE',  ( 17.71441209160705910, -276.2845628980930996, -221.4573699871448582 ) ) ;
#75352 = CARTESIAN_POINT ( 'NONE',  ( 35.86057388107091981, -276.3710001678674075, -271.5774712844498708 ) ) ;
#75353 = CARTESIAN_POINT ( 'NONE',  ( 32.72829147636313962, -283.8999001108152811, -297.1042839005453970 ) ) ;
#75354 = CONICAL_SURFACE ( 'NONE', #64864, 2.390969801828402019, 0.09862129276974965220 ) ;
#75355 = VERTEX_POINT ( 'NONE', #10410 ) ;
#75356 = CARTESIAN_POINT ( 'NONE',  ( 216.5288609127277084, 293.9636489450776935, 13.99999999999999112 ) ) ;
#75357 = CARTESIAN_POINT ( 'NONE',  ( 25.71343354142396720, -293.9701106841199589, -314.5774547246325028 ) ) ;
#75358 = CARTESIAN_POINT ( 'NONE',  ( -55.17315685265742076, -287.8017243051488094, -197.8239431479683788 ) ) ;
#75359 = CARTESIAN_POINT ( 'NONE',  ( 195.7122344542522399, 26.11845659094913685, 14.66853270682850940 ) ) ;
#75360 = CARTESIAN_POINT ( 'NONE',  ( -37.30987171927208834, -283.5523547857346784, -190.3611179825600175 ) ) ;
#75361 = CARTESIAN_POINT ( 'NONE',  ( -113.9191096521135478, -277.6622799374305259, -277.3062882068961699 ) ) ;
#75362 = CARTESIAN_POINT ( 'NONE',  ( -8.791848100974863911, -290.8193944210870541, -199.7116568020229295 ) ) ;
#75363 = CARTESIAN_POINT ( 'NONE',  ( -60.21200603465616297, -287.2703344579918507, -200.3064474805385657 ) ) ;
#75364 =( BOUNDED_SURFACE ( )  B_SPLINE_SURFACE ( 3, 2, ( 
 ( #47115, #62295, #48530 ),
 ( #4065, #54241, #76500 ),
 ( #90660, #62789, #26303 ),
 ( #60896, #82652, #25820 ),
 ( #10680, #32000, #18739 ),
 ( #4997, #83576, #55198 ),
 ( #47598, #91624, #89745 ),
 ( #26777, #19662, #54700 ),
 ( #24906, #33396, #84053 ),
 ( #76964, #11624, #40470 ) ),
 .UNSPECIFIED., .F., .F., .F. ) 
 B_SPLINE_SURFACE_WITH_KNOTS ( ( 4, 2, 2, 2, 4 ),
 ( 3, 3 ),
 ( -2.168404344971008868E-19, 0.002513556688247616140, 0.005027113376495232280, 0.007540670064742848420, 0.01005422675299046456 ),
 ( 0.000000000000000000, 1.000000000000000000 ),
 .UNSPECIFIED. ) 
 GEOMETRIC_REPRESENTATION_ITEM ( )  RATIONAL_B_SPLINE_SURFACE ( (
 ( 1.000000000000000000, 0.8168508380123963297, 1.000000000000000000),
 ( 1.000000000000000000, 0.8469576315469661276, 1.000000000000000000),
 ( 1.000000000000000000, 0.8738409315860931059, 1.000000000000000000),
 ( 1.000000000000000000, 0.9200669567820307648, 1.000000000000000000),
 ( 1.000000000000000000, 0.9394145480633124823, 1.000000000000000000),
 ( 1.000000000000000000, 0.9701920524516296496, 1.000000000000000000),
 ( 1.000000000000000000, 0.9815163856011694943, 1.000000000000000000),
 ( 1.000000000000000000, 0.9964122006648195029, 1.000000000000000000),
 ( 1.000000000000000000, 1.000002041055502389, 1.000000000000000000),
 ( 1.000000000000000000, 1.000000000000000000, 1.000000000000000000) ) ) 
 REPRESENTATION_ITEM ( '' )  SURFACE ( )  );
#75365 = CARTESIAN_POINT ( 'NONE',  ( -46.00476219779407216, -278.9235134409516945, -343.9170399857970892 ) ) ;
#75366 = CARTESIAN_POINT ( 'NONE',  ( -82.93892312404993561, -286.8675972362315747, -208.9803675943674364 ) ) ;
#75367 = CARTESIAN_POINT ( 'NONE',  ( 37.12874587794093628, -283.6719962762423393, -279.6821982932442552 ) ) ;
#75368 = CARTESIAN_POINT ( 'NONE',  ( 39.31709503734047217, -275.6214960333552426, -262.5782332446160581 ) ) ;
#75369 = CARTESIAN_POINT ( 'NONE',  ( -113.2995155449436311, -278.2275700493729573, -282.9868964382306444 ) ) ;
#75370 =( BOUNDED_CURVE ( )  B_SPLINE_CURVE ( 3, ( #88367, #24914, #23517, #53791 ),
 .UNSPECIFIED., .F., .F. ) 
 B_SPLINE_CURVE_WITH_KNOTS ( ( 4, 4 ),
 ( 4.712388980384689674, 6.283185307179586232 ),
 .UNSPECIFIED. ) 
 CURVE ( )  GEOMETRIC_REPRESENTATION_ITEM ( )  RATIONAL_B_SPLINE_CURVE ( ( 1.000000000000000000, 0.8047378541243649375, 0.8047378541243649375, 1.000000000000000000 ) ) 
 REPRESENTATION_ITEM ( '' )  );
#75371 = CARTESIAN_POINT ( 'NONE',  ( -108.0827537339674507, -298.7758212115975311, -247.0238949430231798 ) ) ;
#75372 = DIRECTION ( 'NONE',  ( 0.000000000000000000, 0.000000000000000000, 1.000000000000000000 ) ) ;
#75373 = CARTESIAN_POINT ( 'NONE',  ( 31.98288692825981272, -278.4805209788417528, -303.7098442033569654 ) ) ;
#75374 = CARTESIAN_POINT ( 'NONE',  ( -112.0675664805953602, -270.9702663037409707, -256.2959009891208098 ) ) ;
#75375 = CARTESIAN_POINT ( 'NONE',  ( 207.0561972617101674, 35.35788477359429294, 14.49999999999999822 ) ) ;
#75376 = CARTESIAN_POINT ( 'NONE',  ( -93.65746993446894919, -277.4003203043759527, -316.9266403862098969 ) ) ;
#75377 = CARTESIAN_POINT ( 'NONE',  ( 25.80849035868142138, -276.1817352553266574, -226.9781913343555573 ) ) ;
#75378 = CARTESIAN_POINT ( 'NONE',  ( 9.057031034392009516, -281.4912993696004833, -331.5164771819336238 ) ) ;
#75379 = CARTESIAN_POINT ( 'NONE',  ( 36.66867560463269626, -289.3209148574447340, -271.0231563411240927 ) ) ;
#75380 = CARTESIAN_POINT ( 'NONE',  ( -79.08138327671389334, -297.1243357125612761, -334.2399611328908122 ) ) ;
#75381 = CARTESIAN_POINT ( 'NONE',  ( -50.38473620873794800, -296.4200609167568246, -345.8991389058134587 ) ) ;
#75382 = CARTESIAN_POINT ( 'NONE',  ( -1.585301103958060009, -294.5273562399443108, -204.6083880934220076 ) ) ;
#75383 = CARTESIAN_POINT ( 'NONE',  ( -86.67413386912890871, -277.3642737467271218, -214.0908824675673543 ) ) ;
#75384 = CARTESIAN_POINT ( 'NONE',  ( -19.20696102403819694, -282.2073331598957111, -198.1105339240040735 ) ) ;
#75385 = CARTESIAN_POINT ( 'NONE',  ( -109.2198446831052649, -294.8833523136493113, -250.9511066080622470 ) ) ;
#75386 = CARTESIAN_POINT ( 'NONE',  ( -89.87173445043413267, -285.3786451039043754, -325.6334107386399523 ) ) ;
#75387 = CARTESIAN_POINT ( 'NONE',  ( 4.914718632275406840, -285.5581694718601966, -210.3938894123811565 ) ) ;
#75388 = CARTESIAN_POINT ( 'NONE',  ( -1.176032765980912442, -279.8678231192329235, -202.4983351698289766 ) ) ;
#75389 = CARTESIAN_POINT ( 'NONE',  ( -69.20386377067950434, -197.1553935057814329, -359.8476434964631494 ) ) ;
#75390 = ORIENTED_EDGE ( 'NONE', *, *, #31774, .T. ) ;
#75391 = CARTESIAN_POINT ( 'NONE',  ( -22.45137806013714510, -285.9146668119472565, -198.8223991060767446 ) ) ;
#75392 = VERTEX_POINT ( 'NONE', #40670 ) ;
#75393 = CARTESIAN_POINT ( 'NONE',  ( -50.02877699809521772, -284.2899392448449021, -346.0489649473844906 ) ) ;
#75394 = CARTESIAN_POINT ( 'NONE',  ( 35.60785113091043286, -275.8296825684327018, -266.1335175944963680 ) ) ;
#75395 = CARTESIAN_POINT ( 'NONE',  ( 29.79101526281119661, -285.8655537276382006, -233.3564738196167809 ) ) ;
#75396 = CARTESIAN_POINT ( 'NONE',  ( -64.26734567658402852, -290.6293759687758325, -198.4963863440569583 ) ) ;
#75397 = CARTESIAN_POINT ( 'NONE',  ( 22.68380223392676243, -281.8505438747735639, -222.4887952267571336 ) ) ;
#75399 = CARTESIAN_POINT ( 'NONE',  ( -61.84349475687296405, -281.2596210423544676, -198.0394208202278890 ) ) ;
#75398 = B_SPLINE_CURVE_WITH_KNOTS ( 'NONE', 3,
 ( #81141, #2080, #36661, #58915, #58460, #16285, #87761, #57993, #86847, #66038 ),
 .UNSPECIFIED., .F., .F.,
 ( 4, 2, 2, 2, 4 ),
 ( 8.886119947416682612E-17, 0.0005219798220732356541, 0.001043959644146382404, 0.001565939466219529261, 0.002087919288292675903 ),
 .UNSPECIFIED. ) ;
#75400 = CARTESIAN_POINT ( 'NONE',  ( 10.80647592606522345, -281.0302018658910015, -210.2303526422367099 ) ) ;
#75401 = CARTESIAN_POINT ( 'NONE',  ( -6.941161984400256557, -277.9809262143061233, -207.3071070584150277 ) ) ;
#75402 = CARTESIAN_POINT ( 'NONE',  ( -55.52635933303225357, -169.8022349263865465, -364.5488151334876079 ) ) ;
#75403 = ORIENTED_EDGE ( 'NONE', *, *, #74502, .F. ) ;
#75404 = CARTESIAN_POINT ( 'NONE',  ( 17.90133156924967750, -278.2588308063758404, -320.8602921365193197 ) ) ;
#75405 = CARTESIAN_POINT ( 'NONE',  ( 24.53442447440543717, -22.56791868723661310, -344.6573901678291350 ) ) ;
#75406 = CARTESIAN_POINT ( 'NONE',  ( 31.54898167787137453, -279.1952580483235806, -241.6222808393749517 ) ) ;
#75407 = CARTESIAN_POINT ( 'NONE',  ( -99.97986236466763899, -296.4197585603535003, -232.5751212401761165 ) ) ;
#75408 = CARTESIAN_POINT ( 'NONE',  ( -77.13206452982005601, -291.0419367364358436, -204.4494397070376692 ) ) ;
#75409 = CARTESIAN_POINT ( 'NONE',  ( 153.6987871352777404, 19.48326534539592458, 11.45812909364015297 ) ) ;
#75411 = CARTESIAN_POINT ( 'NONE',  ( 19.28860886320061496, -285.2874478753681160, -223.0186112760830781 ) ) ;
#75410 = CARTESIAN_POINT ( 'NONE',  ( -82.60680842947836311, -296.0222551359900081, -208.7350419860082695 ) ) ;
#75412 = CARTESIAN_POINT ( 'NONE',  ( 35.54152331504181461, -295.5955191682776899, -284.4643524746339835 ) ) ;
#75413 = CARTESIAN_POINT ( 'NONE',  ( -22.37566657928664071, -287.5628567668544520, -198.3557010508719713 ) ) ;
#75414 = ORIENTED_EDGE ( 'NONE', *, *, #63294, .F. ) ;
#75415 = CARTESIAN_POINT ( 'NONE',  ( 19.23412005513974776, -293.7853309483400039, -218.4766618935138922 ) ) ;
#75416 = CARTESIAN_POINT ( 'NONE',  ( -94.32907488382490158, -284.3987133522176691, -316.1022113187067930 ) ) ;
#75417 = CARTESIAN_POINT ( 'NONE',  ( -104.8961631381495749, -295.8175168407189517, -234.1321119835277500 ) ) ;
#75418 = CARTESIAN_POINT ( 'NONE',  ( -64.34165984888359446, -292.5115763540368903, -198.3664673955713340 ) ) ;
#75419 = CARTESIAN_POINT ( 'NONE',  ( -104.5592611150223377, -291.5301760400951139, -232.9268235716128856 ) ) ;
#75420 = CARTESIAN_POINT ( 'NONE',  ( -3.364479692689621881, -288.7573924854837060, -335.0278493176429606 ) ) ;
#75421 = ORIENTED_EDGE ( 'NONE', *, *, #36276, .F. ) ;
#75422 = CARTESIAN_POINT ( 'NONE',  ( 140.6539576904058606, 131.0000000000000568, -11.50000000000000000 ) ) ;
#75423 = CARTESIAN_POINT ( 'NONE',  ( -79.95026689803805198, -299.3432684683767775, -207.6496786365150626 ) ) ;
#75424 = CARTESIAN_POINT ( 'NONE',  ( -110.6526080846042674, -271.6294500476170697, -247.9646197041413132 ) ) ;
#75425 = CARTESIAN_POINT ( 'NONE',  ( 24.32210373110764934, -281.1568332811862660, -309.9636086721840798 ) ) ;
#75426 = VERTEX_POINT ( 'NONE', #53976 ) ;
#75427 = CARTESIAN_POINT ( 'NONE',  ( -38.55028482043721283, -276.5745819193871284, -347.2900866910381410 ) ) ;
#75428 = CIRCLE ( 'NONE', #34609, 8.550761578869359170 ) ;
#75429 = CARTESIAN_POINT ( 'NONE',  ( -83.67722140541020792, -271.8037732317044970, -212.9201928424127459 ) ) ;
#75430 = CARTESIAN_POINT ( 'NONE',  ( -97.07301344490083750, -279.8047577323887367, -314.4622951484155919 ) ) ;
#75431 = CARTESIAN_POINT ( 'NONE',  ( -56.94885020070252324, -275.4471545935467134, -342.0135678286415555 ) ) ;
#75432 = CARTESIAN_POINT ( 'NONE',  ( -107.9808136697012912, -297.4951821191953059, -290.2921526658607831 ) ) ;
#75433 = CARTESIAN_POINT ( 'NONE',  ( -60.62705750101235935, -298.8226808384153514, -200.7946990238000353 ) ) ;
#75434 = CARTESIAN_POINT ( 'NONE',  ( -46.05879257339719146, -299.5434698108736598, -194.6613642591835003 ) ) ;
#75435 = CARTESIAN_POINT ( 'NONE',  ( -32.75693280770970262, -272.1297432355383421, -195.1326468809630796 ) ) ;
#75436 = CARTESIAN_POINT ( 'NONE',  ( 28.48995345694742554, -294.6344645119119718, -302.2597342487869696 ) ) ;
#75437 = CARTESIAN_POINT ( 'NONE',  ( 18.93885819975810492, -291.4587117284910391, -222.9493718335389474 ) ) ;
#75438 = DIRECTION ( 'NONE',  ( -0.01818181818181330636, 0.000000000000000000, 0.9998346970812744816 ) ) ;
#75439 = CARTESIAN_POINT ( 'NONE',  ( 23.58026961463914262, -275.4166318513267129, -223.3498842020389645 ) ) ;
#75440 = CARTESIAN_POINT ( 'NONE',  ( -108.5353678881545108, -272.9317305373718341, -254.2222928887280489 ) ) ;
#75441 = CARTESIAN_POINT ( 'NONE',  ( -92.09259267088177126, -282.4992613816153266, -323.7992882179617027 ) ) ;
#75442 = FACE_OUTER_BOUND ( 'NONE', #10751, .T. ) ;
#75443 = CARTESIAN_POINT ( 'NONE',  ( -95.25050953846822210, -283.1209787989429856, -315.0936674656495029 ) ) ;
#75444 = CARTESIAN_POINT ( 'NONE',  ( -101.3700716200489467, -282.0248365383689588, -309.7361871153909192 ) ) ;
#75445 = ADVANCED_FACE ( 'NONE', ( #47311 ), #13, .T. ) ;
#75446 = CARTESIAN_POINT ( 'NONE',  ( -16.22904348933836971, -275.3486658582631890, -340.9101579455689262 ) ) ;
#75447 = CARTESIAN_POINT ( 'NONE',  ( 18.82090464115082185, -282.8604287763149046, -220.5785614886872850 ) ) ;
#75448 = CYLINDRICAL_SURFACE ( 'NONE', #86688, 0.5000000000000004441 ) ;
#75449 = SPHERICAL_SURFACE ( 'NONE', #48865, 35.00000000000000000 ) ;
#75450 = CARTESIAN_POINT ( 'NONE',  ( -100.5335881872930486, -271.5200136539978644, -227.6852286739031399 ) ) ;
#75451 = CARTESIAN_POINT ( 'NONE',  ( -85.89117158931847484, -279.7225441514551676, -327.8136690351561811 ) ) ;
#75452 = CARTESIAN_POINT ( 'NONE',  ( 113.5000000000000568, -211.8141737103562434, -420.2472828204663529 ) ) ;
#75453 = CARTESIAN_POINT ( 'NONE',  ( -88.92145780250835685, -287.2548237929879633, -215.0736053048038059 ) ) ;
#75454 = CARTESIAN_POINT ( 'NONE',  ( 158.5846220834750113, 17.31716537717171889, -10.56280983457258316 ) ) ;
#75455 = CARTESIAN_POINT ( 'NONE',  ( -95.85189033846208417, -287.9063580454692328, -317.3019677763954292 ) ) ;
#75456 = CARTESIAN_POINT ( 'NONE',  ( -110.4443161140219871, -295.4404229792202159, -263.2459833580459758 ) ) ;
#75457 = CARTESIAN_POINT ( 'NONE',  ( -56.40526817440679963, -287.4398563908156348, -342.1602714547207142 ) ) ;
#75458 = CARTESIAN_POINT ( 'NONE',  ( -32.04911714649202992, -124.5213432794980974, -365.6788127701597659 ) ) ;
#75459 = CARTESIAN_POINT ( 'NONE',  ( -76.22636613857584109, -295.5326814296889779, -206.1683707727777346 ) ) ;
#75460 = CARTESIAN_POINT ( 'NONE',  ( 37.61280969453202516, -285.8515519814939694, -256.0597470183237192 ) ) ;
#75461 = CARTESIAN_POINT ( 'NONE',  ( 34.84346732286840620, -282.9511790556244932, -254.9470931158175233 ) ) ;
#75462 = CARTESIAN_POINT ( 'NONE',  ( -102.0668173571852435, -282.2648171203965717, -310.1685696986380094 ) ) ;
#75463 = CARTESIAN_POINT ( 'NONE',  ( -23.78517560321560254, -288.8742271508500608, -342.1430102089080378 ) ) ;
#75464 = CARTESIAN_POINT ( 'NONE',  ( 36.29264799876062142, -282.9897620476032216, -271.3033343605562209 ) ) ;
#75465 = CARTESIAN_POINT ( 'NONE',  ( 35.68040274552090807, -282.2955766887364462, -265.8473370328452461 ) ) ;
#75466 = CARTESIAN_POINT ( 'NONE',  ( 23.36296611403582091, -288.9260064859467434, -225.7141662209383242 ) ) ;
#75467 = CARTESIAN_POINT ( 'NONE',  ( -114.3207138216981775, -272.9212413174133189, -267.4986742080367890 ) ) ;
#75468 = ORIENTED_EDGE ( 'NONE', *, *, #56056, .T. ) ;
#75469 = CARTESIAN_POINT ( 'NONE',  ( -55.33361865955895809, -273.8268481185501173, -195.4926274971984128 ) ) ;
#75470 = CARTESIAN_POINT ( 'NONE',  ( 23.92382483820542305, -294.9504984232843867, -227.6961137215915016 ) ) ;
#75471 = DIRECTION ( 'NONE',  ( 1.000000000000000000, 0.000000000000000000, 0.000000000000000000 ) ) ;
#75472 = CARTESIAN_POINT ( 'NONE',  ( -69.85430415644619018, -279.9805209788416391, -337.9475929042657754 ) ) ;
#75473 = EDGE_LOOP ( 'NONE', ( #60265, #73219, #32073 ) ) ;
#75474 = CARTESIAN_POINT ( 'NONE',  ( 32.47179602852396130, -273.9156722061202345, -298.3599745655197353 ) ) ;
#75475 = CARTESIAN_POINT ( 'NONE',  ( 208.4306832106270804, -147.7221692137691775, -8.500000000000007105 ) ) ;
#75476 = CARTESIAN_POINT ( 'NONE',  ( -89.05031925654860459, -295.7398368506991346, -214.3194964663088058 ) ) ;
#75477 = CARTESIAN_POINT ( 'NONE',  ( -59.49865158884114180, -273.1062489779997691, -200.6449195533147076 ) ) ;
#75478 = CARTESIAN_POINT ( 'NONE',  ( -92.92201667035706691, -291.3881049729789652, -318.8267731078408929 ) ) ;
#75479 = CARTESIAN_POINT ( 'NONE',  ( -77.39382854392350453, -292.4414631337652963, -209.0485135921806261 ) ) ;
#75480 = CARTESIAN_POINT ( 'NONE',  ( 22.64622667818251500, -283.9106732801743078, -313.7351348400027859 ) ) ;
#75481 = CARTESIAN_POINT ( 'NONE',  ( -112.7754452456914294, -291.8239159292358522, -282.5412818059990059 ) ) ;
#75482 = CARTESIAN_POINT ( 'NONE',  ( -88.33334392329902585, -292.6702770558816837, -213.3247214041538768 ) ) ;
#75483 = CARTESIAN_POINT ( 'NONE',  ( 21.32520173268260777, -293.9945727066852328, -313.8029714257997966 ) ) ;
#75484 = CARTESIAN_POINT ( 'NONE',  ( 27.43596741592070387, -290.0584838143359434, -308.2640377754182168 ) ) ;
#75485 = CARTESIAN_POINT ( 'NONE',  ( 32.39329112684018952, -282.1383118845998865, -303.1368738788993937 ) ) ;
#75486 = CARTESIAN_POINT ( 'NONE',  ( -103.9720348149101738, -295.1025535926976318, -234.6171638881198191 ) ) ;
#75487 = CARTESIAN_POINT ( 'NONE',  ( -94.40058091006845586, -283.6829267836913573, -322.0844857593970687 ) ) ;
#75488 = CARTESIAN_POINT ( 'NONE',  ( 36.24293263423945177, -277.3693427529578912, -257.7494534230675072 ) ) ;
#75489 = CIRCLE ( 'NONE', #34675, 3.000000000000002665 ) ;
#75490 = CARTESIAN_POINT ( 'NONE',  ( -110.6386073502017524, -276.4471613113626063, -289.5920658546791060 ) ) ;
#75491 = DIRECTION ( 'NONE',  ( 0.000000000000000000, 0.000000000000000000, 1.000000000000000000 ) ) ;
#75492 = CARTESIAN_POINT ( 'NONE',  ( 18.53737438131143378, -281.7280861414042761, -317.4498203518813852 ) ) ;
#75493 = CARTESIAN_POINT ( 'NONE',  ( -19.86182089997161881, -281.4769613736951328, -195.7247144114786579 ) ) ;
#75494 = CARTESIAN_POINT ( 'NONE',  ( 7.416498944221869394, -285.7044324591514055, -207.9295940157504390 ) ) ;
#75495 = CARTESIAN_POINT ( 'NONE',  ( 25.69938988429784033, -294.7838866398691948, -231.4850727887573214 ) ) ;
#75496 = CARTESIAN_POINT ( 'NONE',  ( 30.52841517487776812, -276.7014170784158296, -235.7188336728002582 ) ) ;
#75497 = EDGE_CURVE ( 'NONE', #55526, #83549, #18936, .T. ) ;
#75498 = CARTESIAN_POINT ( 'NONE',  ( 22.36292467856653232, -276.2221205815426401, -222.5004490848821774 ) ) ;
#75500 = ADVANCED_FACE ( 'NONE', ( #39274 ), #24183, .F. ) ;
#75499 = CARTESIAN_POINT ( 'NONE',  ( -107.8208158827665102, -278.1342603841832783, -289.3793788641613673 ) ) ;
#75501 = CARTESIAN_POINT ( 'NONE',  ( -58.44559637772922400, -299.7788533558973540, -198.5651989685439105 ) ) ;
#75502 = CARTESIAN_POINT ( 'NONE',  ( 36.94106174778084295, -285.6685888657775649, -279.4220072260627035 ) ) ;
#75503 = CARTESIAN_POINT ( 'NONE',  ( -30.59703257196175841, -294.6357889647652541, -347.0439306009369602 ) ) ;
#75504 = CARTESIAN_POINT ( 'NONE',  ( -72.78351026826467773, -291.1136839774639498, -337.8317681975417486 ) ) ;
#75505 = CARTESIAN_POINT ( 'NONE',  ( 11.14551424664102264, -291.6624211656057923, -215.3095878084267554 ) ) ;
#75506 = VERTEX_POINT ( 'NONE', #33132 ) ;
#75507 = CARTESIAN_POINT ( 'NONE',  ( 21.82433282734990598, -292.6201021311567843, -227.5441993546482422 ) ) ;
#75508 = ORIENTED_EDGE ( 'NONE', *, *, #56743, .F. ) ;
#75509 = CARTESIAN_POINT ( 'NONE',  ( -8.337244887857906406, -289.7608717291013249, -341.3699342028843375 ) ) ;
#75510 = CARTESIAN_POINT ( 'NONE',  ( -81.35585617356750276, -280.0873078208157949, -211.9310644025564727 ) ) ;
#75511 = CARTESIAN_POINT ( 'NONE',  ( -113.8114384287864453, -295.5538293187850059, -263.8828272511983073 ) ) ;
#75512 = CARTESIAN_POINT ( 'NONE',  ( 21.41650567535096172, -288.8727355960625118, -319.9674284450643995 ) ) ;
#75513 = CARTESIAN_POINT ( 'NONE',  ( 23.84204542667185933, -287.2621871429266207, -223.6244821193059238 ) ) ;
#75514 = CARTESIAN_POINT ( 'NONE',  ( -94.29883822965433637, -284.2396730946844627, -316.0753385126189414 ) ) ;
#75515 = CARTESIAN_POINT ( 'NONE',  ( 44.85892074982627520, 12.63905672353519272, -331.9659920184308248 ) ) ;
#75516 = CARTESIAN_POINT ( 'NONE',  ( 198.0048462530024835, 289.0459362520341529, -97.09714635992116882 ) ) ;
#75517 = CARTESIAN_POINT ( 'NONE',  ( -98.40372196300425855, -246.1885688021466763, -331.2951966265923147 ) ) ;
#75518 = CARTESIAN_POINT ( 'NONE',  ( -37.82105694835537690, -276.2554370994141095, -343.5335049148077360 ) ) ;
#75519 = CARTESIAN_POINT ( 'NONE',  ( 35.68744478371312567, -274.3810996434528420, -263.4050330088518876 ) ) ;
#75520 = CARTESIAN_POINT ( 'NONE',  ( -112.4217224872212881, -272.4314421411885405, -253.3689275932013345 ) ) ;
#75521 = CARTESIAN_POINT ( 'NONE',  ( 162.0739375835457281, 217.5763800931431149, -202.8919388766017278 ) ) ;
#75522 = CARTESIAN_POINT ( 'NONE',  ( -2.961819958517478923, -275.2922904668048432, -338.7227716373371891 ) ) ;
#75523 = CARTESIAN_POINT ( 'NONE',  ( -34.01728514677294157, -275.8546823244878397, -196.4224793688113664 ) ) ;
#75524 = VERTEX_POINT ( 'NONE', #90856 ) ;
#75525 = CARTESIAN_POINT ( 'NONE',  ( -107.0088747935059956, -290.7509747666633757, -292.5391565758814068 ) ) ;
#75526 = CARTESIAN_POINT ( 'NONE',  ( -36.19766262801284995, -298.8689617876239595, -193.5224416173093402 ) ) ;
#75527 = CARTESIAN_POINT ( 'NONE',  ( -107.1079312135632193, -296.6290083186109428, -302.7987489562058272 ) ) ;
#75528 = CARTESIAN_POINT ( 'NONE',  ( 14.31777978567131271, -294.4679853012818285, -322.0102727936088627 ) ) ;
#75529 = ORIENTED_EDGE ( 'NONE', *, *, #85679, .F. ) ;
#75530 = CARTESIAN_POINT ( 'NONE',  ( -3.350576749848003910, -278.5270951069018679, -337.8582451197406726 ) ) ;
#75531 = CARTESIAN_POINT ( 'NONE',  ( -5.486724394857766640, -282.1518654395823660, -340.3953055234222234 ) ) ;
#75532 = ADVANCED_FACE ( 'NONE', ( #77162 ), #69126, .F. ) ;
#75533 = CARTESIAN_POINT ( 'NONE',  ( -109.9298667100904510, -279.7711835162901934, -259.7524929787789461 ) ) ;
#75534 = CARTESIAN_POINT ( 'NONE',  ( -51.10676383128398470, -278.9859116570374340, -345.0906103715138329 ) ) ;
#75535 = CARTESIAN_POINT ( 'NONE',  ( -52.74081829727114012, -296.4258192511982770, -198.3488129022006490 ) ) ;
#75536 = CARTESIAN_POINT ( 'NONE',  ( 175.2296996224750103, 138.1603916158177583, 0.000000000000000000 ) ) ;
#75537 = CARTESIAN_POINT ( 'NONE',  ( -90.96640795698880311, -278.0067604918602342, -319.9663575602717174 ) ) ;
#75538 = CARTESIAN_POINT ( 'NONE',  ( -81.16669618310218937, -274.2763950910264725, -207.1814360051211565 ) ) ;
#75539 = CARTESIAN_POINT ( 'NONE',  ( -26.23281384118568482, -287.5983874803950471, -346.0571609255298995 ) ) ;
#75540 = CARTESIAN_POINT ( 'NONE',  ( 14.62250010335176320, -276.7838768361430084, -216.2804140178161276 ) ) ;
#75541 = CARTESIAN_POINT ( 'NONE',  ( 37.32598281151900466, -274.3321727037697428, -286.6500436654783357 ) ) ;
#75542 = DIRECTION ( 'NONE',  ( 0.000000000000000000, 0.000000000000000000, 1.000000000000000000 ) ) ;
#75543 = CARTESIAN_POINT ( 'NONE',  ( -66.40255638834896956, -288.6397127836306140, -337.5574081931004002 ) ) ;
#75544 = CARTESIAN_POINT ( 'NONE',  ( -114.2243790779740493, -283.9414484010326873, -267.1104305919835724 ) ) ;
#75545 = CARTESIAN_POINT ( 'NONE',  ( -6.856294350873071153, -280.8863254607354634, -337.8184333113400726 ) ) ;
#75547 = CARTESIAN_POINT ( 'NONE',  ( -110.3362999244276921, -282.8208447903838305, -255.7630838256315542 ) ) ;
#75546 = CARTESIAN_POINT ( 'NONE',  ( 35.61943195404269602, -279.9963577087116846, -260.3873852803664590 ) ) ;
#75549 = CARTESIAN_POINT ( 'NONE',  ( -102.1093901187677631, -292.0459073519975846, -308.2800806593347716 ) ) ;
#75548 = AXIS2_PLACEMENT_3D ( 'NONE', #85264, #48795, #50206 ) ;
#75550 = CARTESIAN_POINT ( 'NONE',  ( -97.20068485962379157, -279.1670777993381876, -312.8568427931883775 ) ) ;
#75551 = CARTESIAN_POINT ( 'NONE',  ( 153.3221070565148807, 19.65277508768675574, -12.04734487801197140 ) ) ;
#75552 = CARTESIAN_POINT ( 'NONE',  ( 37.63472146234818894, -280.1248233117642599, -284.0340992244089762 ) ) ;
#75553 = CARTESIAN_POINT ( 'NONE',  ( 0.7755028547181611609, -296.5439030358364789, -334.9527543265875806 ) ) ;
#75554 = CARTESIAN_POINT ( 'NONE',  ( -68.23968056714322472, -277.8917835280247459, -200.9258260093619413 ) ) ;
#75555 = CIRCLE ( 'NONE', #19596, 2.336627660646517501 ) ;
#75556 = CARTESIAN_POINT ( 'NONE',  ( -95.34884929620213256, -278.5785463339040575, -314.8477824328130055 ) ) ;
#75557 = CARTESIAN_POINT ( 'NONE',  ( -35.90799773116832228, -285.0343997545045909, -345.5269191039802763 ) ) ;
#75558 = CARTESIAN_POINT ( 'NONE',  ( 198.4468466364687060, 24.69666864892464275, 10.58981561310753250 ) ) ;
#75559 = CARTESIAN_POINT ( 'NONE',  ( -110.1477862413914011, -292.2142253722082046, -290.5746783988967081 ) ) ;
#75560 = CARTESIAN_POINT ( 'NONE',  ( 21.97205936250373171, -286.0916722070055016, -221.5140427754677717 ) ) ;
#75561 = CARTESIAN_POINT ( 'NONE',  ( -64.34556793961483834, -290.0936685552413792, -201.6653334189272471 ) ) ;
#75562 = CARTESIAN_POINT ( 'NONE',  ( -48.18343439337932210, -275.7009706631373547, -431.5134930252627896 ) ) ;
#75563 = CARTESIAN_POINT ( 'NONE',  ( 9.968811875681153012, -275.0689077901557198, -326.6013076209559927 ) ) ;
#75564 = CARTESIAN_POINT ( 'NONE',  ( -45.24540603004871286, -293.2927583535905001, -344.2257062649113095 ) ) ;
#75565 = DIRECTION ( 'NONE',  ( -1.000000000000000000, 0.000000000000000000, 0.000000000000000000 ) ) ;
#75566 = CARTESIAN_POINT ( 'NONE',  ( 140.6539576904058606, 275.5000000000000568, 12.50000000000000000 ) ) ;
#75567 = CARTESIAN_POINT ( 'NONE',  ( 21.68535148986741845, -291.3767933418693019, -222.0029239246068187 ) ) ;
#75568 = CARTESIAN_POINT ( 'NONE',  ( -106.3198232020318130, -286.4988033804119709, -244.1226166710571874 ) ) ;
#75569 = CARTESIAN_POINT ( 'NONE',  ( -31.92173493456361300, -287.2246484879873947, -346.2061088682024774 ) ) ;
#75570 = CARTESIAN_POINT ( 'NONE',  ( -35.94030054764591853, -287.4953448964360518, -196.7852320008686036 ) ) ;
#75571 = CARTESIAN_POINT ( 'NONE',  ( 201.0876323342543515, 25.81167821795958162, 10.49999999999999822 ) ) ;
#75572 = CARTESIAN_POINT ( 'NONE',  ( 16.13596863575206442, -289.0721462814268534, -320.3626107389182494 ) ) ;
#75573 = CARTESIAN_POINT ( 'NONE',  ( 22.65013893752675145, -294.9108322113206668, -224.7396072971405090 ) ) ;
#75574 = DIRECTION ( 'NONE',  ( 0.000000000000000000, 0.000000000000000000, 1.000000000000000000 ) ) ;
#75575 = CARTESIAN_POINT ( 'NONE',  ( 9.555495966421391429, -287.8862709523839953, -209.7916395636346749 ) ) ;
#75576 = CARTESIAN_POINT ( 'NONE',  ( -77.07880479656978423, -275.6596411057477667, -334.6891594915077803 ) ) ;
#75577 = CARTESIAN_POINT ( 'NONE',  ( -97.90964294489629083, -278.2501198563418257, -317.8718388211117940 ) ) ;
#75578 = CARTESIAN_POINT ( 'NONE',  ( -5.194173601533837115, -290.5518041158099436, -201.9809253793999062 ) ) ;
#75579 = CARTESIAN_POINT ( 'NONE',  ( -56.55665423666910385, -279.8112414680044822, -195.7421482812434874 ) ) ;
#75580 = CARTESIAN_POINT ( 'NONE',  ( -104.0125327661936439, -298.9789486562990533, -236.6774143496517411 ) ) ;
#75581 = CARTESIAN_POINT ( 'NONE',  ( -48.18343439338108425, -263.3051960260782494, -501.2887401258802811 ) ) ;
#75582 = CARTESIAN_POINT ( 'NONE',  ( -110.3054443252012362, -282.7755235712349418, -252.9481042794747907 ) ) ;
#75583 = CARTESIAN_POINT ( 'NONE',  ( -110.3882400659495033, -273.0210997072354075, -270.3670888080694112 ) ) ;
#75584 = CARTESIAN_POINT ( 'NONE',  ( -110.8413992618360737, -276.8315705250254268, -259.5812321447068598 ) ) ;
#75585 = CARTESIAN_POINT ( 'NONE',  ( 34.55395801893807572, -279.8291311987075574, -291.8940776148406826 ) ) ;
#75586 = CARTESIAN_POINT ( 'NONE',  ( -42.77628441597607889, -275.5994431365209039, -346.4740146987608114 ) ) ;
#75587 = CARTESIAN_POINT ( 'NONE',  ( -72.43788831395643513, -297.0456299846624688, -335.1749445751922281 ) ) ;
#75588 = CARTESIAN_POINT ( 'NONE',  ( -5.596071932459578235, -281.5646362357951489, -340.1730625288862484 ) ) ;
#75589 = CARTESIAN_POINT ( 'NONE',  ( -110.6193688495461345, -297.4787155192013302, -271.4786303251781874 ) ) ;
#75590 = CARTESIAN_POINT ( 'NONE',  ( -51.72443379259166818, -299.1871589961564837, -195.1643586863121982 ) ) ;
#75591 = CARTESIAN_POINT ( 'NONE',  ( -59.47801267278511261, -273.4243297800937285, -200.7231899841992515 ) ) ;
#75592 = CARTESIAN_POINT ( 'NONE',  ( 18.20267363971293761, -294.8486975109893820, -219.8883203971818148 ) ) ;
#75593 = CARTESIAN_POINT ( 'NONE',  ( 39.64000551281363016, -287.6978412453868827, -268.6827255662338985 ) ) ;
#75594 = CARTESIAN_POINT ( 'NONE',  ( -110.9925362049629598, -276.8471102391508794, -253.4830686850930022 ) ) ;
#75595 = CARTESIAN_POINT ( 'NONE',  ( -90.78440842374472197, -291.1528845215802903, -214.8535836960148515 ) ) ;
#75596 = CARTESIAN_POINT ( 'NONE',  ( 16.17473577180080824, -287.3283430989260410, -320.4293012437802872 ) ) ;
#75597 = CARTESIAN_POINT ( 'NONE',  ( -44.67545329771427731, -289.9593064398290494, -195.6689869793197829 ) ) ;
#75598 = ORIENTED_EDGE ( 'NONE', *, *, #43751, .T. ) ;
#75599 = CARTESIAN_POINT ( 'NONE',  ( 197.0349383350915105, 285.8449894349855640, -111.9383547020201064 ) ) ;
#75600 = CARTESIAN_POINT ( 'NONE',  ( -68.79014287673274453, -288.9847860389822358, -336.3079442182998378 ) ) ;
#75601 = DIRECTION ( 'NONE',  ( 0.000000000000000000, -1.000000000000000000, 0.000000000000000000 ) ) ;
#75602 = CARTESIAN_POINT ( 'NONE',  ( -114.1191699866896130, -285.4621353624736457, -272.8535896670638294 ) ) ;
#75603 = CARTESIAN_POINT ( 'NONE',  ( 33.11320743190675842, -292.2213349698519664, -239.8828271342735263 ) ) ;
#75604 = CARTESIAN_POINT ( 'NONE',  ( -4.025973531531053418, -282.0842764504088223, -201.8157177411264342 ) ) ;
#75605 = ADVANCED_FACE ( 'NONE', ( #90397 ), #83181, .T. ) ;
#75606 = CARTESIAN_POINT ( 'NONE',  ( -2.628955654622771476, -281.8166113933995689, -202.1678702321460150 ) ) ;
#75607 = CARTESIAN_POINT ( 'NONE',  ( -86.93039352514583129, -283.5985774135995143, -324.0022979817832720 ) ) ;
#75608 = CARTESIAN_POINT ( 'NONE',  ( -109.4375384162540428, -296.2084115790212309, -297.5520761096885849 ) ) ;
#75609 = CARTESIAN_POINT ( 'NONE',  ( -87.68321915755521445, -274.6467622389861276, -216.7472846845810466 ) ) ;
#75610 = CARTESIAN_POINT ( 'NONE',  ( 35.56157207631360251, -291.3646958269602578, -254.2719629792056253 ) ) ;
#75611 = CARTESIAN_POINT ( 'NONE',  ( -60.60099853117307589, -296.6636858989128314, -200.7859825983607038 ) ) ;
#75612 = ORIENTED_EDGE ( 'NONE', *, *, #88205, .F. ) ;
#75613 = LINE ( 'NONE', #3175, #10793 ) ;
#75614 = CARTESIAN_POINT ( 'NONE',  ( -94.37381194975721144, -287.1384832664475084, -222.5212557131695235 ) ) ;
#75615 = CARTESIAN_POINT ( 'NONE',  ( 22.93727962674821796, -295.2686063970570558, -317.7946071113971698 ) ) ;
#75616 = CARTESIAN_POINT ( 'NONE',  ( -101.0842615080306501, -285.6937978764972854, -234.4693920906954929 ) ) ;
#75617 = CARTESIAN_POINT ( 'NONE',  ( 37.67317811608269551, -274.8161146696110109, -286.7193684492440866 ) ) ;
#75618 = CARTESIAN_POINT ( 'NONE',  ( 27.96140394629875914, -293.6705370729663400, -229.6548877418164807 ) ) ;
#75619 = CARTESIAN_POINT ( 'NONE',  ( -4.011029042539628442, -284.6265726013100448, -202.3073330086760393 ) ) ;
#75620 = VECTOR ( 'NONE', #14602, 1000.000000000000000 ) ;
#75621 = CARTESIAN_POINT ( 'NONE',  ( -11.16443524875701954, -292.7173091475025899, -197.9138331013843413 ) ) ;
#75622 = CARTESIAN_POINT ( 'NONE',  ( -71.17878848368118838, -289.8449971651592705, -335.0833499140610456 ) ) ;
#75623 = CARTESIAN_POINT ( 'NONE',  ( 191.4749582765727212, 14.19731191252289015, 13.00000000000000178 ) ) ;
#75624 = DIRECTION ( 'NONE',  ( -0.000000000000000000, 0.000000000000000000, -1.000000000000000000 ) ) ;
#75625 = CARTESIAN_POINT ( 'NONE',  ( -105.1350182532626718, -260.3806308838838959, -315.5284000272559410 ) ) ;
#75626 = CARTESIAN_POINT ( 'NONE',  ( -102.3174723830525750, -285.5445516917910709, -310.3718261940808816 ) ) ;
#75627 = CARTESIAN_POINT ( 'NONE',  ( -115.3430155898818299, -275.8380690714489560, -288.1317622949166548 ) ) ;
#75628 = VERTEX_POINT ( 'NONE', #11819 ) ;
#75629 = CARTESIAN_POINT ( 'NONE',  ( -91.90427036224906487, -282.7745485682152093, -319.3407302205261544 ) ) ;
#75630 = CARTESIAN_POINT ( 'NONE',  ( -111.7095002220548707, -278.4684188084473249, -250.4312396981229085 ) ) ;
#75631 = CARTESIAN_POINT ( 'NONE',  ( -71.80817234150255501, -281.5957443637915389, -203.9231040330332689 ) ) ;
#75632 = CARTESIAN_POINT ( 'NONE',  ( 162.8546122839350403, 218.1056854647095236, -203.8705316301375774 ) ) ;
#75633 = CARTESIAN_POINT ( 'NONE',  ( 21.14719141989809614, -280.7940828509410949, -319.5307820050714440 ) ) ;
#75634 = CARTESIAN_POINT ( 'NONE',  ( 33.40741838781508477, -285.2630762879289819, -246.5617685939234889 ) ) ;
#75635 = CARTESIAN_POINT ( 'NONE',  ( -51.63231078431872589, -299.6320545980326528, -195.6767165542249245 ) ) ;
#75636 = CARTESIAN_POINT ( 'NONE',  ( -86.52678036557627195, -296.2502273313650107, -324.3871887590011056 ) ) ;
#75637 = ORIENTED_EDGE ( 'NONE', *, *, #46981, .F. ) ;
#75638 = CARTESIAN_POINT ( 'NONE',  ( 34.13126325227502633, -292.0120806445708013, -253.1941790877583287 ) ) ;
#75639 = CARTESIAN_POINT ( 'NONE',  ( -22.94983159419836127, -277.5242185744853600, -345.9545391471402809 ) ) ;
#75640 = CARTESIAN_POINT ( 'NONE',  ( -48.87543607973791637, -273.9012764497288686, -198.2268470693725533 ) ) ;
#75641 = CARTESIAN_POINT ( 'NONE',  ( 25.89749349388204891, -273.8973568763689741, -226.9523902113789688 ) ) ;
#75642 = DIRECTION ( 'NONE',  ( -1.000000000000000000, 0.000000000000000000, 0.000000000000000000 ) ) ;
#75643 = CARTESIAN_POINT ( 'NONE',  ( -60.77366303512233259, -271.7480946324538991, -199.0618446551372074 ) ) ;
#75644 = CARTESIAN_POINT ( 'NONE',  ( -61.38878195573088448, -296.7836181382269842, -342.9446551372978433 ) ) ;
#75645 = DIRECTION ( 'NONE',  ( -0.000000000000000000, -1.000000000000000000, -0.000000000000000000 ) ) ;
#75646 = LINE ( 'NONE', #25002, #70017 ) ;
#75647 = CARTESIAN_POINT ( 'NONE',  ( -105.4962559509446578, -285.2704820234149565, -297.5026165127687818 ) ) ;
#75648 = CARTESIAN_POINT ( 'NONE',  ( 37.87148765206244150, -283.4493427249642536, -281.1754786946539753 ) ) ;
#75649 = CARTESIAN_POINT ( 'NONE',  ( -110.4109664734769325, -283.9295207002436428, -268.1759443989990359 ) ) ;
#75650 = CARTESIAN_POINT ( 'NONE',  ( -18.83580362120691021, -275.2097468847273376, -341.8032078706576158 ) ) ;
#75651 = CARTESIAN_POINT ( 'NONE',  ( -1.817076402661904622, -284.4367422749386378, -335.5589818411642682 ) ) ;
#75652 = CARTESIAN_POINT ( 'NONE',  ( -76.74272308500547979, -276.0695467329869075, -332.6968766596721139 ) ) ;
#75653 = CARTESIAN_POINT ( 'NONE',  ( 0.7614402486004525628, -275.6530691849285404, -207.7322367299512393 ) ) ;
#75654 = DIRECTION ( 'NONE',  ( 0.000000000000000000, 0.000000000000000000, -1.000000000000000000 ) ) ;
#75655 = CARTESIAN_POINT ( 'NONE',  ( -108.3672986922079531, -279.7283784804499192, -241.0434924193680502 ) ) ;
#75656 = VERTEX_POINT ( 'NONE', #17997 ) ;
#75657 = DIRECTION ( 'NONE',  ( -1.000000000000000000, -0.000000000000000000, -0.000000000000000000 ) ) ;
#75658 = CARTESIAN_POINT ( 'NONE',  ( -111.9168309691474690, -286.2389262482744243, -284.0223615257261258 ) ) ;
#75659 = CARTESIAN_POINT ( 'NONE',  ( 17.19412622853532824, -293.4456276253310421, -319.1493105483372688 ) ) ;
#75660 = CARTESIAN_POINT ( 'NONE',  ( -104.5168979631347526, -290.3865997928229490, -232.9337806188935076 ) ) ;
#75661 = CARTESIAN_POINT ( 'NONE',  ( 31.41839514244654907, -286.1550643673737113, -297.8857912562353931 ) ) ;
#75663 = CARTESIAN_POINT ( 'NONE',  ( -110.7014682631587306, -288.9246336265083528, -260.1676451368796847 ) ) ;
#75662 = CARTESIAN_POINT ( 'NONE',  ( 35.15101999619818685, -285.9574891468421356, -257.4170380447608295 ) ) ;
#75664 = CARTESIAN_POINT ( 'NONE',  ( -83.02996685808358279, -284.8983164834764921, -327.8694507334673744 ) ) ;
#75665 = CARTESIAN_POINT ( 'NONE',  ( 37.63225285613200555, -273.5266078951023587, -268.3844997456997703 ) ) ;
#75666 = CARTESIAN_POINT ( 'NONE',  ( 38.54884860006462333, -286.0387249353732386, -277.2215135863347655 ) ) ;
#75667 = CARTESIAN_POINT ( 'NONE',  ( 30.88186307268721364, -289.1419799849931564, -239.0826013017536411 ) ) ;
#75668 = CARTESIAN_POINT ( 'NONE',  ( 34.62262094288523429, -285.8316026612118321, -292.1121043758279257 ) ) ;
#75669 = CARTESIAN_POINT ( 'NONE',  ( -61.60139569022783235, -284.3163507508396606, -339.5149967977421852 ) ) ;
#75670 = CARTESIAN_POINT ( 'NONE',  ( -12.79770663512714712, -290.7341651381075849, -341.4622770843610624 ) ) ;
#75671 = CARTESIAN_POINT ( 'NONE',  ( 161.2244399300530233, -11.64849832608277325, 13.00000000000000178 ) ) ;
#75672 = CARTESIAN_POINT ( 'NONE',  ( 140.6539576904058606, 275.0000000000000568, 11.50000000000000000 ) ) ;
#75673 = CARTESIAN_POINT ( 'NONE',  ( -100.3624193321353602, -299.0313208375330873, -228.6517799104587709 ) ) ;
#75674 = CARTESIAN_POINT ( 'NONE',  ( -2.189757884915854547, -278.5172269357741470, -204.0944431433552211 ) ) ;
#75675 = CARTESIAN_POINT ( 'NONE',  ( 22.09087532058367742, -292.0939666494101630, -221.6586765984672809 ) ) ;
#75676 = CARTESIAN_POINT ( 'NONE',  ( -72.02312609100363261, -295.9854514089758482, -205.2035463487816003 ) ) ;
#75677 = CARTESIAN_POINT ( 'NONE',  ( 35.84508245194749776, -280.1420811450055908, -263.1192938982639475 ) ) ;
#75678 = CARTESIAN_POINT ( 'NONE',  ( -4.654090668539102360, -272.5659843010729446, -203.4677660792073368 ) ) ;
#75679 = CARTESIAN_POINT ( 'NONE',  ( -66.23167315409401112, -296.7536390291173802, -337.9378368839156224 ) ) ;
#75680 = SURFACE_SIDE_STYLE ('',( #59641 ) ) ;
#75681 = CARTESIAN_POINT ( 'NONE',  ( -48.84617149401242386, -296.3881850962467297, -194.8734951278480878 ) ) ;
#75682 = CARTESIAN_POINT ( 'NONE',  ( -11.42418782859369664, -292.9590987485843812, -341.8470178889565432 ) ) ;
#75683 = CARTESIAN_POINT ( 'NONE',  ( 18.91540504087728181, -294.3087952890889483, -222.9215455076601415 ) ) ;
#75684 = FACE_OUTER_BOUND ( 'NONE', #9721, .T. ) ;
#75685 = CARTESIAN_POINT ( 'NONE',  ( -14.80635326471109359, -293.1545935799424569, -200.7568087163612915 ) ) ;
#75686 = CIRCLE ( 'NONE', #10655, 5.568361562975243650 ) ;
#75687 = CARTESIAN_POINT ( 'NONE',  ( 160.5350683151633291, 249.5000000000000568, 20.22542485937379908 ) ) ;
#75689 = CARTESIAN_POINT ( 'NONE',  ( -80.15477576422820505, -295.6502543090251152, -329.4884429226718225 ) ) ;
#75688 = CARTESIAN_POINT ( 'NONE',  ( -78.28759442156885484, -281.6201749803213943, -333.6212202725016596 ) ) ;
#75690 = CARTESIAN_POINT ( 'NONE',  ( -1.634139488952519592, -282.5921031205814984, -338.5811305390154757 ) ) ;
#75691 = TOROIDAL_SURFACE ( 'NONE', #62110, 4.500000000000002665, 0.5000000000000000000 ) ;
#75692 = CARTESIAN_POINT ( 'NONE',  ( -29.46088157494614990, -285.8161137574834925, -193.7867293762930387 ) ) ;
#75693 = CARTESIAN_POINT ( 'NONE',  ( -110.4593650553174626, -288.3462594590014874, -286.3529994562124443 ) ) ;
#75694 = DIRECTION ( 'NONE',  ( 0.9531768234071980039, -0.3024135303179465994, -1.750957418710600124E-16 ) ) ;
#75695 = CARTESIAN_POINT ( 'NONE',  ( 17.31601092809237841, -280.7694483825137013, -323.6835921970004506 ) ) ;
#75696 = CARTESIAN_POINT ( 'NONE',  ( 31.40421023157099967, -286.9124344535072737, -304.4733753652319024 ) ) ;
#75697 = CARTESIAN_POINT ( 'NONE',  ( 199.6150009768959990, 249.5000000000000568, -2.367926910627510484 ) ) ;
#75698 = CARTESIAN_POINT ( 'NONE',  ( 20.33158342059506296, -295.7958307762324921, -316.4272565429639599 ) ) ;
#75699 = CARTESIAN_POINT ( 'NONE',  ( -45.56800190211330204, -278.5795949427916867, -346.3804354287603360 ) ) ;
#75701 = EDGE_CURVE ( 'NONE', #24951, #59134, #39302, .T. ) ;
#75700 = CARTESIAN_POINT ( 'NONE',  ( -94.80486466489504949, -278.8541698223959884, -225.2846716162187874 ) ) ;
#75702 = CARTESIAN_POINT ( 'NONE',  ( -30.69938480181331641, -292.3004721418380996, -193.5953904363667277 ) ) ;
#75703 = CARTESIAN_POINT ( 'NONE',  ( -109.3213795032796583, -282.3370553878491478, -293.3873016353512071 ) ) ;
#75704 = CARTESIAN_POINT ( 'NONE',  ( -101.8716609544143097, -280.0399051702174802, -308.6844275771397292 ) ) ;
#75705 = EDGE_CURVE ( 'NONE', #73562, #21018, #62095, .T. ) ;
#75706 = CARTESIAN_POINT ( 'NONE',  ( -3.516960721587788719, -291.5689516074891685, -205.4050139368606267 ) ) ;
#75707 = CARTESIAN_POINT ( 'NONE',  ( -111.7864220875513155, -294.6689553751812696, -261.2515614402256006 ) ) ;
#75708 = VERTEX_POINT ( 'NONE', #46850 ) ;
#75709 = CARTESIAN_POINT ( 'NONE',  ( 152.4536156746142410, 250.5000000000000568, -14.50000000000000000 ) ) ;
#75710 = CARTESIAN_POINT ( 'NONE',  ( 22.98025734727558245, -293.6339754671553237, -311.6715371890010147 ) ) ;
#75711 = DIRECTION ( 'NONE',  ( 0.000000000000000000, 0.000000000000000000, 1.000000000000000000 ) ) ;
#75712 = CARTESIAN_POINT ( 'NONE',  ( 17.40634833298269157, -284.4094976428775112, -226.7417163044926838 ) ) ;
#75713 = CARTESIAN_POINT ( 'NONE',  ( -29.07902934490101288, -297.2119807634421704, -193.5976933739872266 ) ) ;
#75714 = CARTESIAN_POINT ( 'NONE',  ( -67.01335932154566422, -286.9864365401885493, -199.8423905823315749 ) ) ;
#75715 = CARTESIAN_POINT ( 'NONE',  ( -3.368263168884978676, -288.4240865118439388, -335.0298367176197871 ) ) ;
#75716 = CARTESIAN_POINT ( 'NONE',  ( -68.31133957715724137, -278.9866277862275297, -337.2449364066092130 ) ) ;
#75717 = CARTESIAN_POINT ( 'NONE',  ( -103.9356322629459868, -274.5777690077635498, -238.5540650569657259 ) ) ;
#75718 = CARTESIAN_POINT ( 'NONE',  ( -110.7477913952213981, -277.3796275827028239, -267.8796118560917989 ) ) ;
#75719 = VERTEX_POINT ( 'NONE', #4717 ) ;
#75720 = CARTESIAN_POINT ( 'NONE',  ( -111.8177335754042190, -272.6325626290558830, -250.6040595744685220 ) ) ;
#75721 = CARTESIAN_POINT ( 'NONE',  ( -96.07186635792241702, -291.8400784423621985, -316.1209830334568096 ) ) ;
#75722 = CARTESIAN_POINT ( 'NONE',  ( 20.68783691572517469, -294.4792001358006246, -220.9548238103238589 ) ) ;
#75723 = CARTESIAN_POINT ( 'NONE',  ( 199.2296996224750103, 66.10105075020101140, -4.735552035431046215E-14 ) ) ;
#75724 = EDGE_CURVE ( 'NONE', #79261, #41691, #51393, .T. ) ;
#75725 = CARTESIAN_POINT ( 'NONE',  ( -80.46095081314754793, -290.3051638082676504, -329.4547972157160984 ) ) ;
#75726 = CARTESIAN_POINT ( 'NONE',  ( -43.53359176515032658, -248.9304517128276473, -457.6964974781342335 ) ) ;
#75727 = CARTESIAN_POINT ( 'NONE',  ( 23.00598319888725030, -291.0711452265879302, -224.5307811190980942 ) ) ;
#75728 = CARTESIAN_POINT ( 'NONE',  ( -30.49118043164711622, -298.4690047432176243, -193.3818862655401176 ) ) ;
#75729 = CARTESIAN_POINT ( 'NONE',  ( -34.47463164901564880, -297.7557351676047119, -197.3401415332614306 ) ) ;
#75730 = CARTESIAN_POINT ( 'NONE',  ( 199.4392256788250677, 65.82574266882504332, -7.741079165001071516 ) ) ;
#75731 = CARTESIAN_POINT ( 'NONE',  ( 196.0953433360011786, 25.50289778183998379, 14.17534932438595341 ) ) ;
#75732 = CARTESIAN_POINT ( 'NONE',  ( -91.09624402796100640, -291.3187812030578243, -324.5940544420357128 ) ) ;
#75733 = CARTESIAN_POINT ( 'NONE',  ( 44.71564893372296723, -290.0519495502701943, -270.3284710469131937 ) ) ;
#75734 = CARTESIAN_POINT ( 'NONE',  ( -80.38408174780046522, -287.4680793534180907, -209.0816246668871088 ) ) ;
#75735 = CARTESIAN_POINT ( 'NONE',  ( -38.07540656457012318, -272.0427788424437949, -195.5313771995554362 ) ) ;
#75736 = CARTESIAN_POINT ( 'NONE',  ( 30.47603271662454461, -277.8779679084992154, -301.0542655364614575 ) ) ;
#75737 = CARTESIAN_POINT ( 'NONE',  ( -69.62032026370162896, -289.7038170951251459, -203.2694408428101269 ) ) ;
#75738 = CARTESIAN_POINT ( 'NONE',  ( -42.69486696654973912, -278.9794353856195812, -345.9365709135371389 ) ) ;
#75739 = ORIENTED_EDGE ( 'NONE', *, *, #7520, .F. ) ;
#75740 = EDGE_CURVE ( 'NONE', #56465, #18301, #92241, .T. ) ;
#75741 = CARTESIAN_POINT ( 'NONE',  ( 7.850475887748682879, -281.7648971298428364, -327.8849627059589693 ) ) ;
#75742 = CARTESIAN_POINT ( 'NONE',  ( -108.2321823212805469, -280.0051727290456256, -241.1030927006030140 ) ) ;
#75743 = CARTESIAN_POINT ( 'NONE',  ( 10.58658974830555799, -279.4920924973067713, -210.5362127420374350 ) ) ;
#75744 = CARTESIAN_POINT ( 'NONE',  ( 43.64731658108150469, 12.32667446486203389, -329.2959963054772174 ) ) ;
#75745 = CARTESIAN_POINT ( 'NONE',  ( 37.40305196647869224, -276.2732887545182052, -252.8099132522576440 ) ) ;
#75746 = DIRECTION ( 'NONE',  ( 1.000000000000000000, 0.000000000000000000, 0.000000000000000000 ) ) ;
#75747 = CARTESIAN_POINT ( 'NONE',  ( -31.33413024532110569, -275.6468135919130873, -194.2781405821475573 ) ) ;
#75748 = CARTESIAN_POINT ( 'NONE',  ( 35.78497577281001440, -296.2662352645559167, -287.0191576251351080 ) ) ;
#75749 = VERTEX_POINT ( 'NONE', #68661 ) ;
#75750 = ADVANCED_BREP_SHAPE_REPRESENTATION ( '', ( #91220, #18940 ), #91438 ) ;
#75751 = ORIENTED_EDGE ( 'NONE', *, *, #67229, .F. ) ;
#75752 = CARTESIAN_POINT ( 'NONE',  ( 196.8803347170859865, 73.40565171261609123, 12.49999999999999289 ) ) ;
#75753 = AXIS2_PLACEMENT_3D ( 'NONE', #73054, #8185, #22850 ) ;
#75754 = CARTESIAN_POINT ( 'NONE',  ( -97.59516461942406806, -291.0521959831235677, -312.1413524450476871 ) ) ;
#75755 = CARTESIAN_POINT ( 'NONE',  ( 36.72677589446506374, -289.0966188602227476, -253.3377499361083096 ) ) ;
#75756 = CARTESIAN_POINT ( 'NONE',  ( -88.73862094798492706, -289.1459851605791300, -322.3442806248777970 ) ) ;
#75757 = CARTESIAN_POINT ( 'NONE',  ( -12.71746630148235901, -285.8715566567333326, -197.4695957623152935 ) ) ;
#75758 = DIRECTION ( 'NONE',  ( -0.000000000000000000, 1.000000000000000000, -0.000000000000000000 ) ) ;
#75759 = CARTESIAN_POINT ( 'NONE',  ( 36.15100354033334895, -279.8571726824498000, -263.0925968060599303 ) ) ;
#75760 = CARTESIAN_POINT ( 'NONE',  ( 25.29303056442937958, -289.9543190067377623, -310.2077739355467543 ) ) ;
#75761 = CARTESIAN_POINT ( 'NONE',  ( -0.9260744269094322023, -281.0391104580084516, -334.4283479660504099 ) ) ;
#75762 = CARTESIAN_POINT ( 'NONE',  ( -43.81107896392224177, -281.2840033397203570, -197.1026857099741960 ) ) ;
#75763 = TOROIDAL_SURFACE ( 'NONE', #34950, 1.000000000000000000, 0.5000000000000000000 ) ;
#75764 = CARTESIAN_POINT ( 'NONE',  ( 12.27290671139417277, -289.3220892131961364, -328.9376576589830847 ) ) ;
#75765 = CARTESIAN_POINT ( 'NONE',  ( -67.33728138209211522, -280.1402030517718913, -203.7272808318804778 ) ) ;
#75766 = CARTESIAN_POINT ( 'NONE',  ( -104.2556355560847976, -289.8330264165567201, -233.0712539019202154 ) ) ;
#75767 = CARTESIAN_POINT ( 'NONE',  ( -89.78352293075727175, -286.1376822277202905, -214.1281323630736324 ) ) ;
#75768 = CARTESIAN_POINT ( 'NONE',  ( -23.80290198384606271, -286.7128994303685658, -194.5690561745006448 ) ) ;
#75769 = CARTESIAN_POINT ( 'NONE',  ( -42.93079811054101924, -283.2911959243219258, -343.1969311162948202 ) ) ;
#75770 = ORIENTED_EDGE ( 'NONE', *, *, #12869, .F. ) ;
#75771 = CARTESIAN_POINT ( 'NONE',  ( 183.0442525570908288, 291.1800221208779931, -7.499999999999996447 ) ) ;
#75772 = CARTESIAN_POINT ( 'NONE',  ( 10.32302065142151370, -294.5618394109116025, -211.4006844012274655 ) ) ;
#75773 = CARTESIAN_POINT ( 'NONE',  ( 39.11345194492690069, -292.2723757330883814, -273.1732333752716499 ) ) ;
#75774 = CARTESIAN_POINT ( 'NONE',  ( -27.24592100949325513, -273.2422152010747709, -197.7739693503697254 ) ) ;
#75775 = CARTESIAN_POINT ( 'NONE',  ( -90.64740119244436301, -295.1321861965166704, -325.8583941265673616 ) ) ;
#75776 = CARTESIAN_POINT ( 'NONE',  ( -84.25567128901064962, -289.8728945075252454, -213.5299024365953073 ) ) ;
#75777 = CARTESIAN_POINT ( 'NONE',  ( -28.80099573426833359, -293.1823856232198295, -343.9317502568304121 ) ) ;
#75778 = CARTESIAN_POINT ( 'NONE',  ( -19.99311056139763565, -293.4850652424813688, -198.9912691879978865 ) ) ;
#75779 = LINE ( 'NONE', #24656, #9664 ) ;
#75780 = CARTESIAN_POINT ( 'NONE',  ( 36.99949668997525976, -291.6943164936869834, -281.4703430961965864 ) ) ;
#75781 = CARTESIAN_POINT ( 'NONE',  ( -93.27285309890446285, -297.8560243752332894, -320.4036446848157880 ) ) ;
#75782 = CARTESIAN_POINT ( 'NONE',  ( 35.86575157290489813, -288.5380873212598658, -273.7588309075588882 ) ) ;
#75783 = CARTESIAN_POINT ( 'NONE',  ( -67.03673063214209549, -279.4193505957185835, -339.6186949564010433 ) ) ;
#75784 = CARTESIAN_POINT ( 'NONE',  ( -73.92081615026943098, -276.3218025514231044, -337.6811477355925604 ) ) ;
#75785 = CARTESIAN_POINT ( 'NONE',  ( -82.86666355484838675, -296.6445946763698203, -208.3948012186001790 ) ) ;
#75786 = CARTESIAN_POINT ( 'NONE',  ( -3.422769643851260035, -274.8377665466923645, -336.1447038572201791 ) ) ;
#75787 = CARTESIAN_POINT ( 'NONE',  ( -99.17639361337023729, -277.1976287871859199, -228.8234626275265668 ) ) ;
#75788 = CARTESIAN_POINT ( 'NONE',  ( -48.39825944296693194, -275.5903687602177570, -345.8080408774952161 ) ) ;
#75789 = DIRECTION ( 'NONE',  ( -1.000000000000000000, 0.000000000000000000, 0.000000000000000000 ) ) ;
#75790 = CARTESIAN_POINT ( 'NONE',  ( -96.36858252565410510, -273.8075911203138730, -227.1525361581299478 ) ) ;
#75791 = CARTESIAN_POINT ( 'NONE',  ( 208.6610849207568208, 0.04196010845019451652, 7.500000000000014211 ) ) ;
#75793 = CARTESIAN_POINT ( 'NONE',  ( 29.08692807571887329, -274.9758998337271692, -239.9694148806571548 ) ) ;
#75792 = CARTESIAN_POINT ( 'NONE',  ( -41.69136755116043247, -287.1267744003523603, -345.6036209785452229 ) ) ;
#75794 = CARTESIAN_POINT ( 'NONE',  ( 37.71963002168703127, -287.3367626469164975, -253.1329553641232337 ) ) ;
#75795 = CARTESIAN_POINT ( 'NONE',  ( -103.9953226774428856, -275.0127505325787070, -235.5019950587779078 ) ) ;
#75796 = CARTESIAN_POINT ( 'NONE',  ( -111.1758283853003633, -294.3951485875724643, -282.5492241632111927 ) ) ;
#75797 = CARTESIAN_POINT ( 'NONE',  ( 8.458505545426366012, -279.8583330375108744, -208.5981323667115532 ) ) ;
#75798 = DIRECTION ( 'NONE',  ( 0.000000000000000000, 0.000000000000000000, 1.000000000000000000 ) ) ;
#75799 = CARTESIAN_POINT ( 'NONE',  ( 16.98403680409870731, -278.8256595112727609, -218.5790221729846223 ) ) ;
#75800 = DIRECTION ( 'NONE',  ( 0.000000000000000000, 9.656854691831248164E-17, 1.000000000000000000 ) ) ;
#75801 = CARTESIAN_POINT ( 'NONE',  ( -103.9100376976680167, -289.7621435623385651, -239.4453139845581120 ) ) ;
#75802 = DIRECTION ( 'NONE',  ( 0.000000000000000000, 0.000000000000000000, -1.000000000000000000 ) ) ;
#75803 = LINE ( 'NONE', #75345, #80549 ) ;
#75804 = CARTESIAN_POINT ( 'NONE',  ( -60.86267007755495939, -289.7468991524940520, -199.0903094513208771 ) ) ;
#75805 = CARTESIAN_POINT ( 'NONE',  ( -38.10881773538898187, -275.5624914613856049, -196.6717748918384814 ) ) ;
#75806 = CARTESIAN_POINT ( 'NONE',  ( -16.28664212961364655, -284.2105810520420164, -343.8686284336190511 ) ) ;
#75808 = CARTESIAN_POINT ( 'NONE',  ( -36.19353185144915841, -283.0373591625779000, -343.3520880378246716 ) ) ;
#75807 = CARTESIAN_POINT ( 'NONE',  ( -69.99304725725514231, -295.6443029165662324, -202.4472288391835946 ) ) ;
#75809 = CARTESIAN_POINT ( 'NONE',  ( -0.2649537176555840645, -275.9808626576804045, -206.7799908900141475 ) ) ;
#75810 = CARTESIAN_POINT ( 'NONE',  ( 21.60523184260414808, -275.7491595865183172, -227.0268251121202923 ) ) ;
#75811 = CARTESIAN_POINT ( 'NONE',  ( -22.10670906802912583, -284.8571383159976449, -343.7974556709527292 ) ) ;
#75812 = ADVANCED_FACE ( 'NONE', ( #3797 ), #66578, .F. ) ;
#75813 = CARTESIAN_POINT ( 'NONE',  ( -64.67130915957531556, -272.6070668355445719, -202.3231856295250282 ) ) ;
#75814 = ORIENTED_EDGE ( 'NONE', *, *, #22374, .F. ) ;
#75815 = CARTESIAN_POINT ( 'NONE',  ( 204.1962367404059364, 292.3752467799872079, -53.99999999998791367 ) ) ;
#75816 = CARTESIAN_POINT ( 'NONE',  ( 38.81623229397770558, -293.5275010491633338, -281.7175845855642251 ) ) ;
#75818 = CARTESIAN_POINT ( 'NONE',  ( -98.87423496814145096, -285.9556975047948413, -312.7074508390106189 ) ) ;
#75817 = CIRCLE ( 'NONE', #24386, 5.603083949679982467 ) ;
#75819 = DIRECTION ( 'NONE',  ( -0.000000000000000000, -1.000000000000000000, -0.000000000000000000 ) ) ;
#75820 = CARTESIAN_POINT ( 'NONE',  ( -19.05039376806006857, -277.7666405000204577, -190.3683826091709363 ) ) ;
#75821 = CARTESIAN_POINT ( 'NONE',  ( -28.62952085060375396, -276.1416396567680067, -346.7576007529440858 ) ) ;
#75822 = CARTESIAN_POINT ( 'NONE',  ( -86.87997863990480596, -288.1275797692470633, -328.3303482179778143 ) ) ;
#75823 = CARTESIAN_POINT ( 'NONE',  ( -81.02167324588612018, -285.1773066873630000, -329.7775032489919909 ) ) ;
#75824 = CARTESIAN_POINT ( 'NONE',  ( -98.47333328313547440, -279.7397192771551317, -312.0851810841267593 ) ) ;
#75825 = CARTESIAN_POINT ( 'NONE',  ( -35.18320931151639286, -287.5039888866168667, -193.9677946916732196 ) ) ;
#75826 = CARTESIAN_POINT ( 'NONE',  ( -19.07134504114123885, -282.2873266987438683, -197.5668012903721547 ) ) ;
#75827 = CARTESIAN_POINT ( 'NONE',  ( -68.84600606113829713, -273.8159883789961668, -200.0866435368874363 ) ) ;
#75828 = CARTESIAN_POINT ( 'NONE',  ( -100.4667217371038390, -277.8025989422488919, -314.4545602543184373 ) ) ;
#75829 = CARTESIAN_POINT ( 'NONE',  ( -58.80042892690541123, -297.2520488593347636, -341.6411092421834041 ) ) ;
#75830 = CARTESIAN_POINT ( 'NONE',  ( 165.0685442354929080, 2.974099043298211065, 8.999832278985701706 ) ) ;
#75831 = EDGE_CURVE ( 'NONE', #53167, #1315, #90728, .T. ) ;
#75832 = CARTESIAN_POINT ( 'NONE',  ( -69.85430415644619018, -279.9805209788416391, -337.9475929042657754 ) ) ;
#75833 = CARTESIAN_POINT ( 'NONE',  ( -105.9189446312957159, -271.2171927607785165, -237.6329107657502107 ) ) ;
#75834 = CARTESIAN_POINT ( 'NONE',  ( -35.12204278231480004, -276.5311816074056424, -343.3889316092275408 ) ) ;
#75835 = CARTESIAN_POINT ( 'NONE',  ( -36.95721522690917737, -275.2619672315118464, -193.7461694587377110 ) ) ;
#75836 = CARTESIAN_POINT ( 'NONE',  ( 33.23318227448275053, -289.0202663177749969, -248.0216449871566624 ) ) ;
#75837 = CARTESIAN_POINT ( 'NONE',  ( -47.51976205650161944, -296.6994137995394567, -345.9859472841586694 ) ) ;
#75838 = CARTESIAN_POINT ( 'NONE',  ( -36.26455936323313978, -296.2440359874659634, -346.9695094656361789 ) ) ;
#75839 = CARTESIAN_POINT ( 'NONE',  ( 23.27516244509033427, -294.9531667750142105, -226.4574000748131084 ) ) ;
#75840 = CARTESIAN_POINT ( 'NONE',  ( -60.27176484683163693, -277.7541595737312150, -199.0727770410573214 ) ) ;
#75841 = CARTESIAN_POINT ( 'NONE',  ( 36.57259670622160996, -283.5920027569522972, -279.6134232125132826 ) ) ;
#75842 = CARTESIAN_POINT ( 'NONE',  ( 53.90367334667526222, -297.2827687489743766, -195.9512618600769258 ) ) ;
#75843 = CARTESIAN_POINT ( 'NONE',  ( -73.66267137309992563, -285.3889649012892278, -336.9109440597525804 ) ) ;
#75844 = CARTESIAN_POINT ( 'NONE',  ( -10.62456063845134047, -285.3293322166863391, -202.0802608954608104 ) ) ;
#75845 = CARTESIAN_POINT ( 'NONE',  ( 155.4712121400794445, 205.7503459434753381, -216.8500784743320651 ) ) ;
#75846 = VERTEX_POINT ( 'NONE', #93232 ) ;
#75847 = CARTESIAN_POINT ( 'NONE',  ( 11.15126855355469715, -286.4122628849373200, -215.6990439395227668 ) ) ;
#75848 = ORIENTED_EDGE ( 'NONE', *, *, #73101, .F. ) ;
#75849 = CARTESIAN_POINT ( 'NONE',  ( -70.32466304100830712, -284.5563150361788871, -339.6114698006052208 ) ) ;
#75850 = CARTESIAN_POINT ( 'NONE',  ( -19.27049385354924738, -274.6242924230606377, -199.5589839046129157 ) ) ;
#75851 = CARTESIAN_POINT ( 'NONE',  ( 4.973188554968406727, -285.4048384834632657, -206.4429475523315602 ) ) ;
#75852 = ADVANCED_FACE ( 'NONE', ( #50624 ), #52904, .F. ) ;
#75853 = CARTESIAN_POINT ( 'NONE',  ( 23.55331173194532468, -281.8677609407910154, -223.5997537293674213 ) ) ;
#75854 = CARTESIAN_POINT ( 'NONE',  ( 208.4306832106270804, -147.7221692137691775, 8.500000000000007105 ) ) ;
#75855 = CARTESIAN_POINT ( 'NONE',  ( -113.0319554170100815, -280.1995096954249789, -260.2788413600054582 ) ) ;
#75856 = CARTESIAN_POINT ( 'NONE',  ( 39.25751857461231253, -281.9873993123113678, -278.5120697616152370 ) ) ;
#75857 = CARTESIAN_POINT ( 'NONE',  ( 30.91033621190086578, -284.8380690714489560, -254.8156830097664738 ) ) ;
#75858 = CARTESIAN_POINT ( 'NONE',  ( 198.2431558926663229, 284.9595988177349000, -111.8567102798726012 ) ) ;
#75859 = ORIENTED_EDGE ( 'NONE', *, *, #32453, .T. ) ;
#75860 = CARTESIAN_POINT ( 'NONE',  ( 22.31345166405351677, -278.1716316210400350, -315.5417697541061557 ) ) ;
#75861 = CARTESIAN_POINT ( 'NONE',  ( -90.79526613475253782, -229.9289224406445840, -347.4232527532336121 ) ) ;
#75862 = CARTESIAN_POINT ( 'NONE',  ( 34.32058505444159380, -279.3020140620238294, -249.4717980706167850 ) ) ;
#75863 = CARTESIAN_POINT ( 'NONE',  ( -1.168557828331867388, -296.3391519785228638, -337.2000398857312007 ) ) ;
#75864 = CARTESIAN_POINT ( 'NONE',  ( -67.34462063162695245, -294.8049035803488778, -337.0360578957497069 ) ) ;
#75865 = CARTESIAN_POINT ( 'NONE',  ( -110.3705018036671390, -290.3667222628482705, -245.9803694960368148 ) ) ;
#75866 = CARTESIAN_POINT ( 'NONE',  ( 61.37083282337847123, -250.8548725835408391, -21.49999999999999289 ) ) ;
#75868 = CARTESIAN_POINT ( 'NONE',  ( 30.14849459084241445, -286.3510009143491857, -300.3460609336086691 ) ) ;
#75867 = CARTESIAN_POINT ( 'NONE',  ( -103.3317076770338474, -295.6331975501249758, -231.7351363714927857 ) ) ;
#75869 = CARTESIAN_POINT ( 'NONE',  ( 34.98414719972961962, -295.6302278905439493, -287.1455366750598728 ) ) ;
#75870 = CARTESIAN_POINT ( 'NONE',  ( -49.51962599725477787, -287.2089537410172966, -197.8320898875983005 ) ) ;
#75871 = ORIENTED_EDGE ( 'NONE', *, *, #72204, .T. ) ;
#75872 = CARTESIAN_POINT ( 'NONE',  ( 24.61743161434209526, -293.8898464370694228, -225.0412966328639470 ) ) ;
#75873 = CARTESIAN_POINT ( 'NONE',  ( -108.9905448076058292, -285.2329558788666759, -256.0631636561234359 ) ) ;
#75874 = CARTESIAN_POINT ( 'NONE',  ( -93.40936182729932113, -294.6317368279528068, -322.5764761156448799 ) ) ;
#75875 = CARTESIAN_POINT ( 'NONE',  ( -98.89363678004025360, -290.7415144173950239, -316.3776322426410843 ) ) ;
#75876 = CARTESIAN_POINT ( 'NONE',  ( -105.9520754209847837, -291.4944093431425358, -235.4277811038375603 ) ) ;
#75877 = CARTESIAN_POINT ( 'NONE',  ( -53.40646254242511759, -289.4306940981847447, -341.5715344471017829 ) ) ;
#75878 = ORIENTED_EDGE ( 'NONE', *, *, #15862, .T. ) ;
#75879 = DIRECTION ( 'NONE',  ( 0.000000000000000000, 0.000000000000000000, 1.000000000000000000 ) ) ;
#75880 = CARTESIAN_POINT ( 'NONE',  ( -29.24840802400338902, -300.0128539397579175, -194.5937777933623352 ) ) ;
#75881 = CARTESIAN_POINT ( 'NONE',  ( -38.33678194534609673, -272.8348684149425480, -193.7646524478022911 ) ) ;
#75882 = CARTESIAN_POINT ( 'NONE',  ( 30.54817846180591090, -280.9775272945856841, -297.8269664604659965 ) ) ;
#75883 = CARTESIAN_POINT ( 'NONE',  ( 4.834672031142612347, -274.1127332149424092, -205.9497839883548806 ) ) ;
#75884 = CARTESIAN_POINT ( 'NONE',  ( -106.6457790048175838, -294.6996640615237197, -295.5642672307021144 ) ) ;
#75885 = CARTESIAN_POINT ( 'NONE',  ( -39.16474588313371896, -278.9356897418955441, -344.5739335008564694 ) ) ;
#75886 = CARTESIAN_POINT ( 'NONE',  ( 5.915415384517144659, -272.7848397515077181, -209.9677474299022606 ) ) ;
#75887 = AXIS2_PLACEMENT_3D ( 'NONE', #70899, #63352, #27338 ) ;
#75888 = CARTESIAN_POINT ( 'NONE',  ( -60.65649446351395113, -298.9480649679464364, -200.7117299812641988 ) ) ;
#75889 = CARTESIAN_POINT ( 'NONE',  ( -47.32840777196063442, -299.0020854215782720, -197.6839933183894686 ) ) ;
#75890 = DIRECTION ( 'NONE',  ( -0.5941640067486292365, -0.8043439146810368312, 0.000000000000000000 ) ) ;
#75891 = CARTESIAN_POINT ( 'NONE',  ( -111.5222636508694194, -297.9313295527707055, -287.8440360214779048 ) ) ;
#75892 = AXIS2_PLACEMENT_3D ( 'NONE', #58817, #23284, #22352 ) ;
#75893 = CARTESIAN_POINT ( 'NONE',  ( -111.9128010852481196, -270.7153572753629760, -259.1636285309245977 ) ) ;
#75894 = CARTESIAN_POINT ( 'NONE',  ( 23.02184643186814483, -294.7775512982865962, -311.6823437035922666 ) ) ;
#75895 = CARTESIAN_POINT ( 'NONE',  ( 29.27961634384813294, -291.7066269868030304, -238.9841901662230157 ) ) ;
#75896 = DIRECTION ( 'NONE',  ( -0.000000000000000000, -0.000000000000000000, 1.000000000000000000 ) ) ;
#75897 = CARTESIAN_POINT ( 'NONE',  ( 31.19263554894574852, -275.5938141829099663, -235.3958246709615594 ) ) ;
#75898 = CARTESIAN_POINT ( 'NONE',  ( -41.87389327199311140, -298.3267503824546338, -197.4807590913360400 ) ) ;
#75899 = CIRCLE ( 'NONE', #15414, 3.038598599789554822 ) ;
#75900 = CARTESIAN_POINT ( 'NONE',  ( 18.58020151246639529, -284.2335064384474208, -320.9463776469651179 ) ) ;
#75901 = CARTESIAN_POINT ( 'NONE',  ( -8.242070812320026363, -281.3639406251772925, -341.1739835726905881 ) ) ;
#75902 = CARTESIAN_POINT ( 'NONE',  ( -96.07671006737689368, -277.2309684685920956, -320.0152173543373237 ) ) ;
#75903 = FACE_OUTER_BOUND ( 'NONE', #57241, .T. ) ;
#75904 = CARTESIAN_POINT ( 'NONE',  ( -109.1399280731205579, -283.5642832097281030, -284.4187205999521666 ) ) ;
#75905 = CARTESIAN_POINT ( 'NONE',  ( -108.9470334338677304, -282.2570618757212060, -293.2663453970592400 ) ) ;
#75906 = EDGE_CURVE ( 'NONE', #82379, #3784, #36290, .T. ) ;
#75907 = CARTESIAN_POINT ( 'NONE',  ( 28.55007982230936392, -274.5689972873958595, -303.2425081282113410 ) ) ;
#75908 = CARTESIAN_POINT ( 'NONE',  ( -40.28239662771523655, -282.0154786147389814, -195.3686349565388127 ) ) ;
#75909 = DIRECTION ( 'NONE',  ( -0.000000000000000000, -1.000000000000000000, -0.000000000000000000 ) ) ;
#75910 = CYLINDRICAL_SURFACE ( 'NONE', #92728, 1.999999999999988454 ) ;
#75911 = CARTESIAN_POINT ( 'NONE',  ( -43.95282829196552399, -272.3699124249708348, -194.3956945121152557 ) ) ;
#75912 = CARTESIAN_POINT ( 'NONE',  ( -110.3124494798008044, -280.7840555670961180, -252.2722113796381791 ) ) ;
#75913 = FACE_OUTER_BOUND ( 'NONE', #78258, .T. ) ;
#75914 = CARTESIAN_POINT ( 'NONE',  ( -92.36582407080817347, -285.7517920350217651, -322.1648260558247330 ) ) ;
#75915 = CARTESIAN_POINT ( 'NONE',  ( 201.5895683924992170, 64.65149228633973166, 9.583120145149372604 ) ) ;
#75916 = CARTESIAN_POINT ( 'NONE',  ( 36.37296566227340122, -285.3710372959798178, -256.2661782117832558 ) ) ;
#75917 = DIRECTION ( 'NONE',  ( -0.000000000000000000, -1.000000000000000000, -0.000000000000000000 ) ) ;
#75918 = CARTESIAN_POINT ( 'NONE',  ( -92.49916027236018579, -294.6596093640908407, -318.7840990553311258 ) ) ;
#75919 = CARTESIAN_POINT ( 'NONE',  ( -102.7423858827700229, -288.2194860516099766, -305.5930369968697278 ) ) ;
#75920 = CARTESIAN_POINT ( 'NONE',  ( 155.8109286537086859, 19.19772955881914456, -9.232252220101429430 ) ) ;
#75921 = CARTESIAN_POINT ( 'NONE',  ( -57.55348217747368267, -284.2758537244203012, -196.7250779611132998 ) ) ;
#75922 = CARTESIAN_POINT ( 'NONE',  ( 7.613689295216106601, -282.2770863868498168, -211.7690998939867768 ) ) ;
#75923 = CARTESIAN_POINT ( 'NONE',  ( -11.07365303351870622, -280.9544067110335845, -341.7189313804644257 ) ) ;
#75924 = CARTESIAN_POINT ( 'NONE',  ( -105.1130437040779100, -290.1874182480229933, -297.6269346142469772 ) ) ;
#75925 =( BOUNDED_CURVE ( )  B_SPLINE_CURVE ( 3, ( #82428, #73926, #38858, #67764 ),
 .UNSPECIFIED., .F., .F. ) 
 B_SPLINE_CURVE_WITH_KNOTS ( ( 4, 4 ),
 ( 5.134959379131569968, 6.283185307179586232 ),
 .UNSPECIFIED. ) 
 CURVE ( )  GEOMETRIC_REPRESENTATION_ITEM ( )  RATIONAL_B_SPLINE_CURVE ( ( 1.000000000000000000, 0.8931162488198151062, 0.8931162488198151062, 1.000000000000000000 ) ) 
 REPRESENTATION_ITEM ( '' )  );
#75926 = CARTESIAN_POINT ( 'NONE',  ( -92.66329760138118843, -280.6646627437276038, -221.8146746845749249 ) ) ;
#75927 = CARTESIAN_POINT ( 'NONE',  ( -69.82116545691290810, -280.4159591185044178, -204.7905015080229418 ) ) ;
#75928 = CARTESIAN_POINT ( 'NONE',  ( 29.94161605740303855, -289.0858619572676957, -236.4293900149949366 ) ) ;
#75929 = ORIENTED_EDGE ( 'NONE', *, *, #45139, .T. ) ;
#75930 = CARTESIAN_POINT ( 'NONE',  ( -111.8182810546301198, -272.7992156270640862, -250.6061241805279565 ) ) ;
#75931 = CARTESIAN_POINT ( 'NONE',  ( -110.3239333518953487, -292.7341566906680441, -254.6945791088535032 ) ) ;
#75932 = CARTESIAN_POINT ( 'NONE',  ( -36.09237171215954021, -122.5496321078137356, -21.50000000000000000 ) ) ;
#75933 = CARTESIAN_POINT ( 'NONE',  ( -112.3417001280813849, -275.0519495502701943, -270.3929463913696054 ) ) ;
#75934 = ORIENTED_EDGE ( 'NONE', *, *, #79929, .F. ) ;
#75935 = CARTESIAN_POINT ( 'NONE',  ( 37.72509889357520052, -273.4907655340558676, -265.5823357582788162 ) ) ;
#75936 = DIRECTION ( 'NONE',  ( 0.8457827187922973833, 0.5335274993777826547, 0.000000000000000000 ) ) ;
#75937 = CARTESIAN_POINT ( 'NONE',  ( -94.06977653310389087, -294.2543601270296563, -321.2565487766985370 ) ) ;
#75938 = CARTESIAN_POINT ( 'NONE',  ( -91.19201809853579732, -272.6094591775613480, -220.9053986992230705 ) ) ;
#75939 = CARTESIAN_POINT ( 'NONE',  ( -100.8921440408006447, -291.5635754280635865, -307.7717521966957861 ) ) ;
#75940 = CARTESIAN_POINT ( 'NONE',  ( -26.57349754528888752, -284.6735780046901709, -343.6389456451801721 ) ) ;
#75941 = CARTESIAN_POINT ( 'NONE',  ( -112.5948973674062330, -292.1444072122308171, -257.1111142486288372 ) ) ;
#75942 = CARTESIAN_POINT ( 'NONE',  ( -3.554328762074253856, -293.8039260857265162, -201.7047652829031108 ) ) ;
#75943 = CARTESIAN_POINT ( 'NONE',  ( 1.568037845835212662, -294.3498214268451534, -332.1869322365337212 ) ) ;
#75944 = CARTESIAN_POINT ( 'NONE',  ( 5.857096093094018130, -288.6375055843107589, -208.9879991021803960 ) ) ;
#75945 = CARTESIAN_POINT ( 'NONE',  ( 37.86598658131583051, -281.9261579276773091, -286.9387915925918833 ) ) ;
#75946 = CARTESIAN_POINT ( 'NONE',  ( -111.2028154621348364, -294.4289458745433876, -286.2937839141118843 ) ) ;
#75947 = CARTESIAN_POINT ( 'NONE',  ( -79.16150573856964456, -283.4330949595740776, -335.0148407152518075 ) ) ;
#75948 = CARTESIAN_POINT ( 'NONE',  ( 30.66289900026975346, -277.9376964185632914, -301.1380784731194353 ) ) ;
#75949 = CARTESIAN_POINT ( 'NONE',  ( -92.05005921254146983, -292.4090924074130839, -314.0302885647153062 ) ) ;
#75950 = CARTESIAN_POINT ( 'NONE',  ( -111.5880219779992757, -276.4990930026191904, -285.5180161879386560 ) ) ;
#75952 = AXIS2_PLACEMENT_3D ( 'NONE', #73682, #31525, #17324 ) ;
#75951 = FACE_OUTER_BOUND ( 'NONE', #23934, .T. ) ;
#75953 = CARTESIAN_POINT ( 'NONE',  ( -10.95939484926375052, -282.2064867201630136, -338.5466899743207705 ) ) ;
#75954 = AXIS2_PLACEMENT_3D ( 'NONE', #78514, #13651, #86056 ) ;
#75955 = CARTESIAN_POINT ( 'NONE',  ( -108.1514886672800060, -280.1305568707308566, -241.1381379045861308 ) ) ;
#75956 = CARTESIAN_POINT ( 'NONE',  ( 0.1792849999216633017, -285.5978368967813594, -203.3760033283395501 ) ) ;
#75957 = CARTESIAN_POINT ( 'NONE',  ( 33.59391552437426043, -295.0345133766168715, -249.0633222129276874 ) ) ;
#75958 = CARTESIAN_POINT ( 'NONE',  ( 38.90709530625224488, -277.1621598068036292, -271.1428842655080302 ) ) ;
#75959 = AXIS2_PLACEMENT_3D ( 'NONE', #11165, #63264, #92095 ) ;
#75960 = CARTESIAN_POINT ( 'NONE',  ( 38.25117004177573676, -277.0199203808313086, -282.4845915570071497 ) ) ;
#75961 = CARTESIAN_POINT ( 'NONE',  ( -39.15989041254362490, -276.9089216448539332, -343.3384719262245994 ) ) ;
#75962 = CARTESIAN_POINT ( 'NONE',  ( -33.72611932015692560, -300.0976701652980978, -195.5265398058162702 ) ) ;
#75963 = CARTESIAN_POINT ( 'NONE',  ( -107.2692529344595869, -282.8990944411660848, -243.7121821111891222 ) ) ;
#75964 = AXIS2_PLACEMENT_3D ( 'NONE', #39550, #40032, #17814 ) ;
#75965 = CARTESIAN_POINT ( 'NONE',  ( -53.38076770319752029, -291.5187051769832465, -195.0172433845634714 ) ) ;
#75966 = CARTESIAN_POINT ( 'NONE',  ( -96.65439090270751876, -291.5040083434977305, -318.2193847732332870 ) ) ;
#75967 = EDGE_CURVE ( 'NONE', #28861, #56456, #42089, .T. ) ;
#75968 = CARTESIAN_POINT ( 'NONE',  ( 2.419655016270580994, -291.5187664587163567, -208.7115247410452241 ) ) ;
#75969 = EDGE_LOOP ( 'NONE', ( #63206, #4899, #5850, #56096, #85160, #18468 ) ) ;
#75970 = CARTESIAN_POINT ( 'NONE',  ( -56.02699608372067530, -290.3909448486285214, -196.2156633963072068 ) ) ;
#75971 = CARTESIAN_POINT ( 'NONE',  ( 33.32973783826315639, -292.9763526627592114, -251.9862617214188560 ) ) ;
#75972 = ORIENTED_EDGE ( 'NONE', *, *, #55295, .T. ) ;
#75973 = CARTESIAN_POINT ( 'NONE',  ( -104.8772340428890004, -291.1600957520788029, -306.6990343754949322 ) ) ;
#75974 = CARTESIAN_POINT ( 'NONE',  ( -76.88395952052188420, -280.1589448643318860, -208.8166071297662256 ) ) ;
#75975 = EDGE_CURVE ( 'NONE', #7049, #91480, #71004, .T. ) ;
#75976 = CARTESIAN_POINT ( 'NONE',  ( -113.3481868144358060, -295.3392275439289278, -280.9734097568272091 ) ) ;
#75977 = CARTESIAN_POINT ( 'NONE',  ( 0.2267371477746556729, -287.1902449482997781, -203.2497028568727160 ) ) ;
#75978 = CARTESIAN_POINT ( 'NONE',  ( 36.76521087307970959, -288.1470900618989504, -291.2399758316909129 ) ) ;
#75979 = CARTESIAN_POINT ( 'NONE',  ( -84.87232902196633688, -284.0625601656288381, -325.7951039806498557 ) ) ;
#75980 = CARTESIAN_POINT ( 'NONE',  ( -90.36657093633624527, -230.3778195935935003, -347.8114039112169849 ) ) ;
#75981 = CARTESIAN_POINT ( 'NONE',  ( -85.04316653643064683, -218.3528564987888103, -351.0001102442844285 ) ) ;
#75982 = CARTESIAN_POINT ( 'NONE',  ( 138.1549688690315918, 178.5493954107672039, -238.2378617337843139 ) ) ;
#75983 = CARTESIAN_POINT ( 'NONE',  ( 33.66837277626137137, -274.5174278050423027, -252.7494379492692929 ) ) ;
#75984 = CARTESIAN_POINT ( 'NONE',  ( 35.66058051292321096, -274.5604895844408020, -277.0613488986852531 ) ) ;
#75985 = CARTESIAN_POINT ( 'NONE',  ( -110.7525165698548051, -296.3514061935542827, -247.1546002169693566 ) ) ;
#75986 = CARTESIAN_POINT ( 'NONE',  ( 174.8086493686545566, 240.3597952296187827, -177.5534806918111883 ) ) ;
#75987 = CARTESIAN_POINT ( 'NONE',  ( 35.58745166541468308, -274.5294829806975940, -293.4833387096866204 ) ) ;
#75988 = CARTESIAN_POINT ( 'NONE',  ( -72.40733836790208500, -275.3419526731543101, -205.1244447376594735 ) ) ;
#75989 = CARTESIAN_POINT ( 'NONE',  ( -20.58583114906167566, -299.1983710257756570, -193.5938057002267385 ) ) ;
#75990 = CARTESIAN_POINT ( 'NONE',  ( -75.89589603595813116, -290.0746458086439361, -332.4220752706754638 ) ) ;
#75991 = CARTESIAN_POINT ( 'NONE',  ( -107.0156433830699996, -296.9394437326857314, -302.7601990080789278 ) ) ;
#75992 = CARTESIAN_POINT ( 'NONE',  ( -111.5643769034880819, -297.3006958774917052, -249.9028719166121846 ) ) ;
#75993 = CARTESIAN_POINT ( 'NONE',  ( -34.29907000615826007, -295.1795156242868075, -343.2976822453702539 ) ) ;
#75994 = ORIENTED_EDGE ( 'NONE', *, *, #4077, .F. ) ;
#75995 = CARTESIAN_POINT ( 'NONE',  ( 7.408287121446841539, -278.3678564565182114, -331.3090201194807491 ) ) ;
#75996 = VERTEX_POINT ( 'NONE', #49217 ) ;
#75997 = CARTESIAN_POINT ( 'NONE',  ( -17.00222038531473245, -279.8156233805706279, -196.1598210473968891 ) ) ;
#75998 = CARTESIAN_POINT ( 'NONE',  ( -83.14460891177755286, -278.6381134529114547, -327.5709484809809169 ) ) ;
#75999 = CARTESIAN_POINT ( 'NONE',  ( -53.88846030834669421, -279.0217260709594029, -344.5782259279454252 ) ) ;
#76000 = CARTESIAN_POINT ( 'NONE',  ( -38.54454208212246158, -275.0872776358256147, -345.7067215570374401 ) ) ;
#76001 = CARTESIAN_POINT ( 'NONE',  ( -74.30992935990809656, -274.0390524495335853, -207.2839531359876446 ) ) ;
#76002 = EDGE_CURVE ( 'NONE', #14370, #39273, #35006, .T. ) ;
#76003 = CARTESIAN_POINT ( 'NONE',  ( -84.43812335347153919, -295.9640594180127664, -213.7499117009384406 ) ) ;
#76004 = CARTESIAN_POINT ( 'NONE',  ( 152.6002739434380260, 20.65727164547434569, -10.65122728699565080 ) ) ;
#76005 = CARTESIAN_POINT ( 'NONE',  ( -108.1715647033971806, -278.4850744267726554, -288.0798524474452051 ) ) ;
#76006 = CARTESIAN_POINT ( 'NONE',  ( -24.19730974589690575, -275.0185951405136962, -194.6011629654353783 ) ) ;
#76007 = CARTESIAN_POINT ( 'NONE',  ( -57.17928305227649588, -287.9875900632906678, -344.3061206459876757 ) ) ;
#76008 = CARTESIAN_POINT ( 'NONE',  ( -43.89409087027367207, -275.9696206021974945, -195.5959630775169558 ) ) ;
#76009 = DIRECTION ( 'NONE',  ( 0.000000000000000000, 0.000000000000000000, 1.000000000000000000 ) ) ;
#76010 = CARTESIAN_POINT ( 'NONE',  ( -63.88900274588976913, -288.6044308017839626, -338.5905129820301340 ) ) ;
#76011 = CARTESIAN_POINT ( 'NONE',  ( -80.87366006422885789, -284.8271148757268634, -206.9069346341300957 ) ) ;
#76012 = CARTESIAN_POINT ( 'NONE',  ( 20.12483232928461163, -280.4431770220854787, -317.0241118479720512 ) ) ;
#76014 = CARTESIAN_POINT ( 'NONE',  ( -30.37258982855084000, -284.2206814078384696, -196.1962563974661862 ) ) ;
#76013 = CARTESIAN_POINT ( 'NONE',  ( 18.93331755614955725, -280.7953119192370082, -317.7989952549624491 ) ) ;
#76015 = CARTESIAN_POINT ( 'NONE',  ( -0.9407073142919682995, -290.5694564146256766, -335.9927982852373702 ) ) ;
#76016 = CARTESIAN_POINT ( 'NONE',  ( -104.8130807538472027, -280.1432436811634261, -241.4691935017444564 ) ) ;
#76017 = CARTESIAN_POINT ( 'NONE',  ( 154.0376014794581465, 19.37029994958559698, -11.97447443758434993 ) ) ;
#76018 = AXIS2_PLACEMENT_3D ( 'NONE', #5359, #33748, #12933 ) ;
#76019 = CARTESIAN_POINT ( 'NONE',  ( -40.57244151061917847, -294.0117071832756324, -195.4178909076942432 ) ) ;
#76020 = CARTESIAN_POINT ( 'NONE',  ( -111.9963532124225623, -276.9724159568884261, -256.1262997992009787 ) ) ;
#76021 = CIRCLE ( 'NONE', #77586, 1.000000000000000888 ) ;
#76022 = CARTESIAN_POINT ( 'NONE',  ( -11.20986616441890504, -277.3537986155270687, -338.6327806393072706 ) ) ;
#76023 = CARTESIAN_POINT ( 'NONE',  ( -101.3434009962186479, -286.0245128532798162, -309.7795237229511258 ) ) ;
#76024 = EDGE_CURVE ( 'NONE', #53167, #69774, #37829, .T. ) ;
#76025 = VECTOR ( 'NONE', #51232, 1000.000000000000000 ) ;
#76026 = EDGE_CURVE ( 'NONE', #82136, #42552, #81626, .T. ) ;
#76027 = DIRECTION ( 'NONE',  ( 0.000000000000000000, 0.000000000000000000, 1.000000000000000000 ) ) ;
#76028 = CARTESIAN_POINT ( 'NONE',  ( -67.45705456184020932, -291.3642470151970656, -339.6603216404498085 ) ) ;
#76029 = CIRCLE ( 'NONE', #50283, 1.000000000000000888 ) ;
#76030 = CARTESIAN_POINT ( 'NONE',  ( -110.3465916710653545, -294.3307108219991051, -287.5999104957114128 ) ) ;
#76031 = CARTESIAN_POINT ( 'NONE',  ( 38.51389189407272085, -286.9069115583802159, -282.9353773197545365 ) ) ;
#76032 = CARTESIAN_POINT ( 'NONE',  ( -75.37460983632033162, -289.9361834806989577, -207.0564003974298544 ) ) ;
#76033 = CARTESIAN_POINT ( 'NONE',  ( 208.4306832106270804, -198.2391364535880598, 0.000000000000000000 ) ) ;
#76034 = CARTESIAN_POINT ( 'NONE',  ( 19.55279810706876020, -274.8914941718879277, -316.9025458673040703 ) ) ;
#76035 = CARTESIAN_POINT ( 'NONE',  ( -71.52023349363894056, -293.6481243479290129, -336.2744556876218667 ) ) ;
#76036 = LINE ( 'NONE', #62796, #60837 ) ;
#76037 = DIRECTION ( 'NONE',  ( 0.000000000000000000, 0.000000000000000000, 1.000000000000000000 ) ) ;
#76038 = CARTESIAN_POINT ( 'NONE',  ( -113.5597172241179038, -288.9856254112971214, -274.0382936655008166 ) ) ;
#76039 = CARTESIAN_POINT ( 'NONE',  ( -69.13787289579103401, -287.2269187639383858, -203.7480474070543153 ) ) ;
#76040 = CARTESIAN_POINT ( 'NONE',  ( -9.949808324987175823, -286.9391682151593841, -341.2388879613669133 ) ) ;
#76041 = CARTESIAN_POINT ( 'NONE',  ( -108.9948986926918622, -285.7573339169599080, -287.1849568370683983 ) ) ;
#76042 = CARTESIAN_POINT ( 'NONE',  ( 160.6539576904058606, 293.9636489450775230, 0.000000000000000000 ) ) ;
#76043 = CARTESIAN_POINT ( 'NONE',  ( -42.69612697970789839, -286.7857398359332137, -197.3831861166171677 ) ) ;
#76044 = CARTESIAN_POINT ( 'NONE',  ( 37.96410137081927871, -295.5669115517113141, -273.0893152886368398 ) ) ;
#76045 = CARTESIAN_POINT ( 'NONE',  ( -69.70683069490866046, -275.5546957679982256, -338.6527543176570703 ) ) ;
#76046 = CARTESIAN_POINT ( 'NONE',  ( -106.3245471169879579, -278.4448854882502360, -304.6440419186031932 ) ) ;
#76047 = CARTESIAN_POINT ( 'NONE',  ( 34.91718699693180383, -291.3493499639941433, -248.2711331495324885 ) ) ;
#76048 = CARTESIAN_POINT ( 'NONE',  ( -35.11085582536794192, -300.0601007652616659, -195.7155521100123963 ) ) ;
#76049 = CARTESIAN_POINT ( 'NONE',  ( -43.27349326848973732, -275.1676604347916282, -506.7546311057413959 ) ) ;
#76050 = CARTESIAN_POINT ( 'NONE',  ( -110.9470825032862820, -282.3671488964955074, -284.7572402772948976 ) ) ;
#76051 = DIRECTION ( 'NONE',  ( 0.000000000000000000, 0.000000000000000000, 1.000000000000000000 ) ) ;
#76052 = CARTESIAN_POINT ( 'NONE',  ( -105.5681333782994074, -277.0782454512280992, -241.1033107563759756 ) ) ;
#76053 = CARTESIAN_POINT ( 'NONE',  ( 30.57030059763306795, -279.9718200200854312, -302.3104308716163473 ) ) ;
#76054 = DIRECTION ( 'NONE',  ( -1.000000000000000000, 0.000000000000000000, 0.000000000000000000 ) ) ;
#76055 = CARTESIAN_POINT ( 'NONE',  ( 14.39871299181071862, -274.8205415338319426, -326.5189986597804364 ) ) ;
#76056 = CARTESIAN_POINT ( 'NONE',  ( -105.5968602864647323, -297.7035912348071065, -298.1449417418108965 ) ) ;
#76057 = CIRCLE ( 'NONE', #69982, 1.000000000000000888 ) ;
#76058 = CARTESIAN_POINT ( 'NONE',  ( -35.91877279613662211, -281.9550661235056737, -347.0518701350185324 ) ) ;
#76059 = CARTESIAN_POINT ( 'NONE',  ( -72.97180650640677868, -298.5088205713158800, -206.3774953287440326 ) ) ;
#76060 = CARTESIAN_POINT ( 'NONE',  ( -91.29966478901761207, -298.6191288769531411, -216.1224203418156549 ) ) ;
#76061 = CARTESIAN_POINT ( 'NONE',  ( -67.06222564507206130, -273.3182351341887397, -203.6482622081232705 ) ) ;
#76062 = CARTESIAN_POINT ( 'NONE',  ( 37.70948608006271741, -295.5572517172814173, -270.7454272195612930 ) ) ;
#76063 = CARTESIAN_POINT ( 'NONE',  ( 35.07319506592877900, -288.0511312081731603, -296.6903482713996709 ) ) ;
#76064 = CARTESIAN_POINT ( 'NONE',  ( 30.73485323614489317, -274.1270672462239872, -303.7354388363376643 ) ) ;
#76065 = CARTESIAN_POINT ( 'NONE',  ( 16.68444365934453799, -288.1427482256304415, -325.3003286409004318 ) ) ;
#76066 = CARTESIAN_POINT ( 'NONE',  ( 14.24063675421330899, -287.3639591154873187, -322.3483372739083848 ) ) ;
#76067 = CARTESIAN_POINT ( 'NONE',  ( -112.1206062431190702, -288.4698658283209056, -276.7570070170708618 ) ) ;
#76068 = ORIENTED_EDGE ( 'NONE', *, *, #46451, .F. ) ;
#76069 = CARTESIAN_POINT ( 'NONE',  ( 168.1488725781630649, 234.1813984995739588, -193.4213935641190858 ) ) ;
#76070 = CARTESIAN_POINT ( 'NONE',  ( 24.28689484107245278, -287.6019351796898036, -309.6027377726563259 ) ) ;
#76071 = CARTESIAN_POINT ( 'NONE',  ( 194.7510731661265595, -164.3527196417747689, -21.50000000000000000 ) ) ;
#76072 = CARTESIAN_POINT ( 'NONE',  ( -106.4724330804543371, -285.9228948723415442, -236.9880453978409776 ) ) ;
#76073 = CARTESIAN_POINT ( 'NONE',  ( -4.693298396127183025, -291.5305477319059264, -200.8852079244021240 ) ) ;
#76074 = CARTESIAN_POINT ( 'NONE',  ( 10.30672033035423141, -282.2968452250051996, -210.8286512880796408 ) ) ;
#76075 = CARTESIAN_POINT ( 'NONE',  ( -6.444976512106915578, -281.7646787273274640, -200.3562913039808961 ) ) ;
#76076 = CARTESIAN_POINT ( 'NONE',  ( -56.32094479663410169, -283.1369305463718433, -340.8507503854584684 ) ) ;
#76077 = CARTESIAN_POINT ( 'NONE',  ( 15.14878992875681796, -278.3119622101590949, -324.0035116118828000 ) ) ;
#76078 = CARTESIAN_POINT ( 'NONE',  ( -110.7997946007286316, -296.2615738536190406, -293.4900583394814930 ) ) ;
#76079 = CARTESIAN_POINT ( 'NONE',  ( -108.4213384445573780, -274.1146472706962527, -251.4861789237028518 ) ) ;
#76080 = CARTESIAN_POINT ( 'NONE',  ( -70.93895424918967763, -289.6266879276687405, -203.7047505313932447 ) ) ;
#76081 = CARTESIAN_POINT ( 'NONE',  ( -110.2786492092206885, -271.4547307310580777, -262.1555123849296933 ) ) ;
#76082 = ORIENTED_EDGE ( 'NONE', *, *, #4626, .F. ) ;
#76083 = CARTESIAN_POINT ( 'NONE',  ( 139.6925840978351516, 15.36528803885690664, -22.50000000000000000 ) ) ;
#76084 = CARTESIAN_POINT ( 'NONE',  ( -110.6147194032072605, -286.6430841782876655, -257.1599668740173001 ) ) ;
#76085 = AXIS2_PLACEMENT_3D ( 'NONE', #35400, #58120, #72768 ) ;
#76086 = CARTESIAN_POINT ( 'NONE',  ( -61.48117441133690164, -296.4380729176240266, -343.2093368443427721 ) ) ;
#76087 = CARTESIAN_POINT ( 'NONE',  ( -107.0806176643818191, -284.9134692792322312, -292.2786007098782761 ) ) ;
#76088 = CARTESIAN_POINT ( 'NONE',  ( 39.39597081608347651, -274.5853459679027537, -268.3239458345869366 ) ) ;
#76089 = CARTESIAN_POINT ( 'NONE',  ( -70.86078524371089316, -292.2728980964574248, -201.1528546015402696 ) ) ;
#76090 = CARTESIAN_POINT ( 'NONE',  ( -107.8698363859662095, -283.0499521734768678, -242.5402707553669472 ) ) ;
#76091 = CARTESIAN_POINT ( 'NONE',  ( -2.069309449261933942, -292.8394817343975660, -201.9241060530037544 ) ) ;
#76093 = CARTESIAN_POINT ( 'NONE',  ( -34.57294953326663034, -289.3498277015729627, -343.3793475435304003 ) ) ;
#76092 = VECTOR ( 'NONE', #67885, 1000.000000000000114 ) ;
#76094 = CARTESIAN_POINT ( 'NONE',  ( 185.2519943799831879, 3.000000000000000000, 9.000000000000001776 ) ) ;
#76095 = AXIS2_PLACEMENT_3D ( 'NONE', #28969, #86708, #21873 ) ;
#76096 = LINE ( 'NONE', #81780, #35724 ) ;
#76097 = CARTESIAN_POINT ( 'NONE',  ( 6.451691864244251562, -59.65713888448967595, -351.0909003801652375 ) ) ;
#76098 = CARTESIAN_POINT ( 'NONE',  ( -113.2124118153363810, -285.9694803670265060, -278.5062306186741239 ) ) ;
#76099 = CARTESIAN_POINT ( 'NONE',  ( -95.99890600148557951, -293.4094976428775681, -317.0979686699210447 ) ) ;
#76100 = ORIENTED_EDGE ( 'NONE', *, *, #40423, .T. ) ;
#76101 = CARTESIAN_POINT ( 'NONE',  ( 17.30236139984067378, -279.7762853634818612, -221.4913664608390036 ) ) ;
#76102 = CARTESIAN_POINT ( 'NONE',  ( 5.855908976923163145, -276.1504848360327173, -334.0769783241346431 ) ) ;
#76103 = CARTESIAN_POINT ( 'NONE',  ( -106.1372464149112886, -280.9382004354164337, -240.9128373064592381 ) ) ;
#76104 = CARTESIAN_POINT ( 'NONE',  ( 27.36103610868812908, -24.54272754578916249, -343.3512226634238687 ) ) ;
#76105 = CARTESIAN_POINT ( 'NONE',  ( -44.38313441369549395, -281.7141632033985843, -346.4997068946032073 ) ) ;
#76107 = TOROIDAL_SURFACE ( 'NONE', #42777, 1.000000000000000000, 0.5000000000000000000 ) ;
#76106 = CARTESIAN_POINT ( 'NONE',  ( -110.5984609935359089, -282.3874139172017408, -284.6891950701244127 ) ) ;
#76108 = CARTESIAN_POINT ( 'NONE',  ( -98.58286273371544439, -275.0152257852059847, -225.6666292473326223 ) ) ;
#76109 = CARTESIAN_POINT ( 'NONE',  ( -68.53792374930726794, -295.9657901631740060, -336.4413729006775498 ) ) ;
#76110 = EDGE_LOOP ( 'NONE', ( #57947, #24218, #5158, #28110 ) ) ;
#76111 = CARTESIAN_POINT ( 'NONE',  ( 35.91466781810470366, -292.3142112879884280, -276.2558641556560133 ) ) ;
#76112 = CARTESIAN_POINT ( 'NONE',  ( 38.08401046024775383, -276.3911036465935354, -285.3369307880264500 ) ) ;
#76113 = CARTESIAN_POINT ( 'NONE',  ( -29.98986665155448250, -274.1477929672778941, -197.7322632171610053 ) ) ;
#76114 = CARTESIAN_POINT ( 'NONE',  ( 22.52571284700371379, -273.8276629161189248, -222.4092399869006442 ) ) ;
#76115 = CARTESIAN_POINT ( 'NONE',  ( 159.4851178187871312, 15.00000000000000000, -6.999999999999999112 ) ) ;
#76116 = CARTESIAN_POINT ( 'NONE',  ( -4.249203765795510179, -272.4881347513623950, -203.0426458878170308 ) ) ;
#76117 = DIRECTION ( 'NONE',  ( -0.3024135303179478207, -0.9531768234071973378, 4.625929269271478222E-15 ) ) ;
#76118 = CARTESIAN_POINT ( 'NONE',  ( -43.41266492080073647, -261.7876796617941295, -500.4428755130637683 ) ) ;
#76119 = AXIS2_PLACEMENT_3D ( 'NONE', #69506, #4178, #26889 ) ;
#76120 = CARTESIAN_POINT ( 'NONE',  ( 12.13539671357389693, -283.4238804594296539, -324.4558770727243200 ) ) ;
#76121 = CARTESIAN_POINT ( 'NONE',  ( -3.326083706890943681, -284.3694042368343844, -338.3234414275487438 ) ) ;
#76122 = CARTESIAN_POINT ( 'NONE',  ( -110.0950005561461751, -284.0012465296653090, -262.7311777370776440 ) ) ;
#76123 = CARTESIAN_POINT ( 'NONE',  ( -32.38698326070905864, -275.3886508705768392, -344.0451246684216926 ) ) ;
#76124 = CARTESIAN_POINT ( 'NONE',  ( 30.45199406605279080, -283.8145644404988843, -300.7344161441818073 ) ) ;
#76125 = CARTESIAN_POINT ( 'NONE',  ( -54.13052162131204881, -275.7513924861306123, -342.1691973884592244 ) ) ;
#76126 = CARTESIAN_POINT ( 'NONE',  ( -1.583818916418291423, -275.6176602082504132, -206.3498702297087846 ) ) ;
#76127 = DIRECTION ( 'NONE',  ( -0.000000000000000000, -0.000000000000000000, 1.000000000000000000 ) ) ;
#76128 = CARTESIAN_POINT ( 'NONE',  ( -56.52624197746927592, -280.6139448484572654, -195.9011761911354199 ) ) ;
#76129 = CIRCLE ( 'NONE', #44342, 25.00000000000000355 ) ;
#76130 = VERTEX_POINT ( 'NONE', #71955 ) ;
#76131 = CARTESIAN_POINT ( 'NONE',  ( 196.0143093133015384, 19.33012701892219454, 12.49999999999999289 ) ) ;
#76132 = CARTESIAN_POINT ( 'NONE',  ( -109.0478871218274719, -286.0992788355792982, -294.8259545129931212 ) ) ;
#76133 = CARTESIAN_POINT ( 'NONE',  ( -7.932760715127213480, -293.8538909085236241, -337.3651416634506290 ) ) ;
#76134 = CARTESIAN_POINT ( 'NONE',  ( -114.0115551577167992, -289.8183958810299146, -276.9366082656763979 ) ) ;
#76135 = CARTESIAN_POINT ( 'NONE',  ( 26.55978144643145100, -286.2987876544191863, -307.8063924156029429 ) ) ;
#76137 = CARTESIAN_POINT ( 'NONE',  ( -66.94913751108470024, -289.8985505982098516, -202.5276921000277923 ) ) ;
#76136 = CARTESIAN_POINT ( 'NONE',  ( -6.755171173920111016, -285.0364444681046052, -203.4156778648855379 ) ) ;
#76138 = CARTESIAN_POINT ( 'NONE',  ( -93.71725922283104637, -285.0939094030924252, -317.3603397071559584 ) ) ;
#76139 = CARTESIAN_POINT ( 'NONE',  ( -8.673318798625839321, -274.6768893177790005, -339.6796075054556923 ) ) ;
#76140 = CARTESIAN_POINT ( 'NONE',  ( 30.71651624715849138, -285.5064175604962315, -236.0898530914087985 ) ) ;
#76141 = CARTESIAN_POINT ( 'NONE',  ( -32.11032877462433532, -300.1177950843049302, -195.3593257338152114 ) ) ;
#76142 = CARTESIAN_POINT ( 'NONE',  ( 13.03747359438205322, -284.7533051515300713, -214.5062549990608147 ) ) ;
#76143 = CARTESIAN_POINT ( 'NONE',  ( 11.45370304120203464, -281.6901796690403899, -215.7496075011398773 ) ) ;
#76144 = CARTESIAN_POINT ( 'NONE',  ( -79.49100149355670908, -291.6197162158988476, -332.6611486431770572 ) ) ;
#76145 = DIRECTION ( 'NONE',  ( -0.000000000000000000, -1.000000000000000000, -0.000000000000000000 ) ) ;
#76146 = EDGE_CURVE ( 'NONE', #75053, #85558, #56333, .T. ) ;
#76147 = CARTESIAN_POINT ( 'NONE',  ( 222.4306832106270804, 15.36528803885690664, 22.50000000000000000 ) ) ;
#76148 = CARTESIAN_POINT ( 'NONE',  ( -39.05030000327838025, -296.9935862307967795, -345.9018016420998265 ) ) ;
#76149 = CARTESIAN_POINT ( 'NONE',  ( -0.9745784581178658090, -278.5348183059059579, -204.7681830609684255 ) ) ;
#76150 = CARTESIAN_POINT ( 'NONE',  ( -5.943545222788352511, -291.6516268500353704, -200.2161613024450162 ) ) ;
#76151 = CARTESIAN_POINT ( 'NONE',  ( -111.1848895209751049, -294.9377440495641167, -271.4548583908583623 ) ) ;
#76152 = CARTESIAN_POINT ( 'NONE',  ( 22.98003335751389997, -280.8182271328700494, -312.3436375328074632 ) ) ;
#76153 = CARTESIAN_POINT ( 'NONE',  ( 10.42751909942468913, -272.7969640136547014, -213.2023037157763667 ) ) ;
#76154 = CARTESIAN_POINT ( 'NONE',  ( 35.32816335982330713, -295.0154124352441158, -281.6623330039305984 ) ) ;
#76155 = CARTESIAN_POINT ( 'NONE',  ( -4.829096099716510437, -294.9805209788416391, -202.7746430608542312 ) ) ;
#76156 = CARTESIAN_POINT ( 'NONE',  ( -111.8645635446429054, -271.3396278418827592, -253.4806818537858533 ) ) ;
#76157 = CARTESIAN_POINT ( 'NONE',  ( -19.54662964627135935, -293.0663389252223965, -344.2888823901656110 ) ) ;
#76158 = TOROIDAL_SURFACE ( 'NONE', #24710, 1.000000000000000000, 0.5000000000000000000 ) ;
#76159 = CARTESIAN_POINT ( 'NONE',  ( 9.207639428972127504, -294.1309697270799575, -213.2991249091605255 ) ) ;
#76160 = DIRECTION ( 'NONE',  ( -0.000000000000000000, -1.000000000000000000, -0.000000000000000000 ) ) ;
#76161 = CARTESIAN_POINT ( 'NONE',  ( 33.60514948766985555, -294.5902378573332498, -288.2257830242676846 ) ) ;
#76162 = CARTESIAN_POINT ( 'NONE',  ( 140.6539576904058606, 250.5000000000000568, -10.49999999999999822 ) ) ;
#76164 = CARTESIAN_POINT ( 'NONE',  ( -15.59282841151147458, -294.7628665931050023, -340.0991984537363351 ) ) ;
#76163 = CARTESIAN_POINT ( 'NONE',  ( -55.33440940062592972, -281.3026256464106041, -343.5367232947555749 ) ) ;
#76165 = VECTOR ( 'NONE', #72754, 1000.000000000000000 ) ;
#76166 = CARTESIAN_POINT ( 'NONE',  ( 36.47868067795234026, -281.8289688222096743, -292.4432063663202257 ) ) ;
#76167 = CARTESIAN_POINT ( 'NONE',  ( -110.6667003585914415, -283.9236722787348981, -293.8393690874095796 ) ) ;
#76168 = CARTESIAN_POINT ( 'NONE',  ( -53.83681850528533630, -287.2642022859209305, -343.3538538751236047 ) ) ;
#76169 = PLANE ( 'NONE',  #59346 ) ;
#76170 = CARTESIAN_POINT ( 'NONE',  ( -10.96007420478843741, -281.1943872675498710, -342.0183486038312708 ) ) ;
#76171 = CIRCLE ( 'NONE', #70103, 0.5000000000000004441 ) ;
#76172 = CARTESIAN_POINT ( 'NONE',  ( 7.741645972113681218, -287.3732558840783327, -332.4667810086199893 ) ) ;
#76173 = CARTESIAN_POINT ( 'NONE',  ( 169.9462594094670180, 249.5000000000000568, -23.92352941176469017 ) ) ;
#76174 = CARTESIAN_POINT ( 'NONE',  ( -2.750946930590558726, -296.1869150250240637, -335.5525300693781219 ) ) ;
#76175 = CARTESIAN_POINT ( 'NONE',  ( -12.04400716799281490, -278.1546641365202390, -342.5181689210476748 ) ) ;
#76176 = CARTESIAN_POINT ( 'NONE',  ( -108.3092153509391835, -278.4456849880803020, -253.1652094586677038 ) ) ;
#76177 = CARTESIAN_POINT ( 'NONE',  ( -13.86847411476865943, -292.5150805279670294, -196.9702428282546123 ) ) ;
#76178 = TOROIDAL_SURFACE ( 'NONE', #29357, 3.342139515347628986, 0.5000000000000000000 ) ;
#76179 = CARTESIAN_POINT ( 'NONE',  ( -13.89247716168959101, -280.8300564381304412, -342.1904165909267590 ) ) ;
#76180 = AXIS2_PLACEMENT_3D ( 'NONE', #19267, #41002, #25426 ) ;
#76181 = CARTESIAN_POINT ( 'NONE',  ( 34.18218954774205542, -292.4031678975247814, -254.5632775188253447 ) ) ;
#76182 = CARTESIAN_POINT ( 'NONE',  ( -108.8994442186181857, -294.2617360929501160, -292.8650043882645377 ) ) ;
#76183 = ORIENTED_EDGE ( 'NONE', *, *, #2076, .T. ) ;
#76184 = DIRECTION ( 'NONE',  ( -0.5831039236546632365, 0.7661730729848328370, -0.2701270746362063324 ) ) ;
#76185 = VECTOR ( 'NONE', #32253, 1000.000000000000114 ) ;
#76186 = CARTESIAN_POINT ( 'NONE',  ( 33.17444996187899875, -293.3126895032967809, -289.5257052011448877 ) ) ;
#76187 = LINE ( 'NONE', #41091, #39791 ) ;
#76188 = CARTESIAN_POINT ( 'NONE',  ( 17.36665895637873192, -291.6952119285918457, -314.0302885647153062 ) ) ;
#76189 = CARTESIAN_POINT ( 'NONE',  ( -31.91811639151086766, -297.1772509278766847, -193.5972525813361074 ) ) ;
#76190 = CARTESIAN_POINT ( 'NONE',  ( 30.91907146842683218, -279.2617524575707648, -237.3652354966351083 ) ) ;
#76191 = CARTESIAN_POINT ( 'NONE',  ( 33.39702184604652047, -288.4930101215028913, -241.0794989330513260 ) ) ;
#76192 = CARTESIAN_POINT ( 'NONE',  ( -5.794353780739670334, -288.4587008117282494, -336.1924550719858189 ) ) ;
#76193 = CARTESIAN_POINT ( 'NONE',  ( -73.16224152467334818, -279.0562693167220800, -334.7774711732768083 ) ) ;
#76194 = CARTESIAN_POINT ( 'NONE',  ( -40.58449608220404770, -299.7709930978458033, -196.4061319642943602 ) ) ;
#76195 = CIRCLE ( 'NONE', #36863, 4.025000000000000355 ) ;
#76196 = CARTESIAN_POINT ( 'NONE',  ( -78.86923746328997709, -276.4203335142410083, -330.9423841821011933 ) ) ;
#76197 = ORIENTED_EDGE ( 'NONE', *, *, #22273, .F. ) ;
#76198 = CARTESIAN_POINT ( 'NONE',  ( -80.60962900258410002, -297.1499246020748046, -206.6289016264463498 ) ) ;
#76199 = CARTESIAN_POINT ( 'NONE',  ( -74.23786127341048768, -291.4667465931088941, -335.0286341508721080 ) ) ;
#76200 = CARTESIAN_POINT ( 'NONE',  ( 38.85525595660539722, -295.1154479318924473, -267.4466598667569883 ) ) ;
#76201 = CARTESIAN_POINT ( 'NONE',  ( 196.5385635023627344, 69.63708600452028463, -11.34458575904874067 ) ) ;
#76202 = CARTESIAN_POINT ( 'NONE',  ( -86.79223756958316471, -290.4129738191232946, -324.2678437636218973 ) ) ;
#76203 = CARTESIAN_POINT ( 'NONE',  ( -48.18343439339133027, -254.4948186591712158, -445.8861037206912670 ) ) ;
#76204 = CARTESIAN_POINT ( 'NONE',  ( -110.7183655319142019, -297.4949820912572136, -247.1806778513567053 ) ) ;
#76205 = CARTESIAN_POINT ( 'NONE',  ( -105.4143060338692663, -288.2562895974788830, -303.7434260337585670 ) ) ;
#76206 = CARTESIAN_POINT ( 'NONE',  ( -75.77303195036481043, -297.8874081006112533, -203.6007872815017947 ) ) ;
#76207 = FACE_OUTER_BOUND ( 'NONE', #68408, .T. ) ;
#76208 = DIRECTION ( 'NONE',  ( -1.000000000000000000, -0.000000000000000000, -0.000000000000000000 ) ) ;
#76209 = CARTESIAN_POINT ( 'NONE',  ( -99.47782662320248903, -292.6642216147709519, -226.0687988101013559 ) ) ;
#76210 = CARTESIAN_POINT ( 'NONE',  ( 36.60358173371528068, -296.4805209788416391, -305.9350535429201159 ) ) ;
#76211 = CARTESIAN_POINT ( 'NONE',  ( -72.05061536490396179, -287.5921755817422536, -204.0639111605298694 ) ) ;
#76212 = CARTESIAN_POINT ( 'NONE',  ( -21.52224098468846236, -272.2552977652755999, -197.2189746191602921 ) ) ;
#76213 = CARTESIAN_POINT ( 'NONE',  ( -54.56804387304662640, -275.7492352321035014, -197.9417333119921807 ) ) ;
#76214 = CARTESIAN_POINT ( 'NONE',  ( -109.8241076460055439, -288.8521103906546728, -253.3463959635021752 ) ) ;
#76215 = CARTESIAN_POINT ( 'NONE',  ( -67.19966758303387167, -279.2998936537179588, -339.9944954805196176 ) ) ;
#76217 = CARTESIAN_POINT ( 'NONE',  ( -61.57632958888007124, -282.7239422256514558, -339.3823613209391965 ) ) ;
#76216 = CARTESIAN_POINT ( 'NONE',  ( -43.75108986543212808, -279.9690414437212667, -197.5928001481529463 ) ) ;
#76218 = CARTESIAN_POINT ( 'NONE',  ( -42.77051135094828282, -278.1988168739889034, -346.8596180892677125 ) ) ;
#76219 = CARTESIAN_POINT ( 'NONE',  ( 32.81546619092550543, -279.9528151303060781, -239.6043182205529263 ) ) ;
#76220 = CARTESIAN_POINT ( 'NONE',  ( 151.9403889390961240, 205.9175150728080439, -214.8626715079458904 ) ) ;
#76221 = CARTESIAN_POINT ( 'NONE',  ( 1.067278298569687367, -275.4929940158611998, -203.8810736652323783 ) ) ;
#76222 = SHAPE_DEFINITION_REPRESENTATION ( #70105, #61554 ) ;
#76223 = CARTESIAN_POINT ( 'NONE',  ( -91.68896306329104107, -274.8146490932733741, -216.7972984447000329 ) ) ;
#76224 = CARTESIAN_POINT ( 'NONE',  ( 7.399455738971494334, -277.1948066931273047, -214.2051214447836571 ) ) ;
#76225 = ORIENTED_EDGE ( 'NONE', *, *, #89855, .F. ) ;
#76226 = CIRCLE ( 'NONE', #35420, 2.842139515347646750 ) ;
#76227 = CARTESIAN_POINT ( 'NONE',  ( 175.2296996224750103, 154.6894116713782807, 0.000000000000000000 ) ) ;
#76228 = CARTESIAN_POINT ( 'NONE',  ( 22.22083613111720979, -289.2267314906696924, -313.0990443304157225 ) ) ;
#76229 = CARTESIAN_POINT ( 'NONE',  ( 6.935038215161405617, -288.4053908461635842, -208.5424231130983799 ) ) ;
#76230 = CARTESIAN_POINT ( 'NONE',  ( -80.47432844673046759, -289.0025470480873082, -329.4450335138739092 ) ) ;
#76231 = CARTESIAN_POINT ( 'NONE',  ( 22.04667438303508575, -286.4021073552116832, -221.4474401773227328 ) ) ;
#76232 = CARTESIAN_POINT ( 'NONE',  ( 223.4306832106270804, -135.2391364535880882, -22.50000000000000000 ) ) ;
#76233 = CARTESIAN_POINT ( 'NONE',  ( 12.44149653315743542, -280.7445121722610111, -324.8411486703859055 ) ) ;
#76234 = CARTESIAN_POINT ( 'NONE',  ( 29.34762096092801187, -289.8469195111678687, -302.9709313845942802 ) ) ;
#76235 = CARTESIAN_POINT ( 'NONE',  ( -68.09115084047047617, -281.9433191321730874, -337.3325972496724034 ) ) ;
#76236 = CARTESIAN_POINT ( 'NONE',  ( -110.1125250017011581, -280.0066481343555438, -259.7287960100724717 ) ) ;
#76237 = CIRCLE ( 'NONE', #6707, 2.000000000000001776 ) ;
#76238 = CARTESIAN_POINT ( 'NONE',  ( -24.31247500908635573, -277.3737919798914504, -342.3029996870943137 ) ) ;
#76239 = CARTESIAN_POINT ( 'NONE',  ( -100.3627047681104187, -288.7690257045032922, -313.9083531752284557 ) ) ;
#76240 = CARTESIAN_POINT ( 'NONE',  ( -87.65195034795991091, -286.1735348565533172, -212.2128125754102825 ) ) ;
#76241 = CARTESIAN_POINT ( 'NONE',  ( 22.93975552307198029, -287.4039946583444589, -222.5314088620413600 ) ) ;
#76242 = CARTESIAN_POINT ( 'NONE',  ( -40.23223348366850161, -283.2561758089654518, -343.3038682833472990 ) ) ;
#76243 = ORIENTED_EDGE ( 'NONE', *, *, #7662, .F. ) ;
#76244 = CARTESIAN_POINT ( 'NONE',  ( 175.2296996224750103, 275.0000000000000568, 0.000000000000000000 ) ) ;
#76245 = CARTESIAN_POINT ( 'NONE',  ( -81.23438751810218150, -293.3229321674481298, -208.6056528654344504 ) ) ;
#76246 = AXIS2_PLACEMENT_3D ( 'NONE', #35987, #50668, #92805 ) ;
#76247 = CARTESIAN_POINT ( 'NONE',  ( 10.87445188436011279, -293.0863395316068818, -329.8305635953509523 ) ) ;
#76248 = AXIS2_PLACEMENT_3D ( 'NONE', #18571, #69703, #83901 ) ;
#76249 = CARTESIAN_POINT ( 'NONE',  ( 0.7450351216454592640, -273.6324716830128523, -207.8086676223443874 ) ) ;
#76250 = EDGE_CURVE ( 'NONE', #44141, #46969, #46845, .T. ) ;
#76251 = CARTESIAN_POINT ( 'NONE',  ( -19.31923069674204285, -294.1748885325274045, -345.1722228434732642 ) ) ;
#76252 = CARTESIAN_POINT ( 'NONE',  ( -77.61805655244667435, -289.9804857328609842, -208.6478871105687176 ) ) ;
#76253 = CARTESIAN_POINT ( 'NONE',  ( -63.95399614429018698, -293.6437524977787916, -339.4788744237098967 ) ) ;
#76254 = CARTESIAN_POINT ( 'NONE',  ( -71.34314728681985684, -290.7166507677868026, -335.4217002395019449 ) ) ;
#76255 = DIRECTION ( 'NONE',  ( -0.000000000000000000, -1.000000000000000000, -0.000000000000000000 ) ) ;
#76256 = TOROIDAL_SURFACE ( 'NONE', #92873, 5.654241149514405151, 1.000000000000000000 ) ;
#76257 = CARTESIAN_POINT ( 'NONE',  ( -4.108406303805257842, -290.4891287321794948, -202.9260320208372832 ) ) ;
#76258 = CARTESIAN_POINT ( 'NONE',  ( 28.48397989213211545, -295.0734138936728641, -234.3103449144501553 ) ) ;
#76259 = CARTESIAN_POINT ( 'NONE',  ( 22.95040097869604523, -289.0707723354784093, -311.9557063478078476 ) ) ;
#76260 = CARTESIAN_POINT ( 'NONE',  ( 34.99957049443172963, -277.2595651719407783, -249.0804711168652830 ) ) ;
#76261 = CARTESIAN_POINT ( 'NONE',  ( -28.66135202697728346, -275.7394613280545741, -346.5239443744176810 ) ) ;
#76262 = CIRCLE ( 'NONE', #62710, 0.5000000000000017764 ) ;
#76263 = CARTESIAN_POINT ( 'NONE',  ( -98.09998604057219040, -296.3788532233318733, -223.3017163505457177 ) ) ;
#76264 = CARTESIAN_POINT ( 'NONE',  ( -51.49632924560014402, -275.4755077687397034, -343.0083511409750940 ) ) ;
#76265 = CARTESIAN_POINT ( 'NONE',  ( -82.13526567517490662, -277.5161543465504224, -210.8417975660866261 ) ) ;
#76266 = CARTESIAN_POINT ( 'NONE',  ( -46.24206423374222652, -275.1418048189901242, -197.5056856308715680 ) ) ;
#76267 = CARTESIAN_POINT ( 'NONE',  ( -6.913075853365770129, -275.0593360712501294, -340.2360802745932347 ) ) ;
#76268 = EDGE_CURVE ( 'NONE', #5915, #70302, #14652, .T. ) ;
#76269 = CARTESIAN_POINT ( 'NONE',  ( 201.0776230153480526, -147.7221692137691775, -8.778910157967986905 ) ) ;
#76270 = CARTESIAN_POINT ( 'NONE',  ( -71.96331869518968460, -274.2334037994623941, -205.9212037993105184 ) ) ;
#76271 = CARTESIAN_POINT ( 'NONE',  ( 150.6539576904058606, 293.9636489450775230, -9.103929867429224387 ) ) ;
#76273 = CARTESIAN_POINT ( 'NONE',  ( -5.306140316738417795, -274.3191742623328082, -204.7521496480252665 ) ) ;
#76272 = CARTESIAN_POINT ( 'NONE',  ( 18.39041245825583815, -286.2768332729150416, -321.0985561820101566 ) ) ;
#76274 = CARTESIAN_POINT ( 'NONE',  ( 35.94775315317257025, -287.8491195265457350, -293.9758599403900803 ) ) ;
#76275 = CARTESIAN_POINT ( 'NONE',  ( -91.58664357536616762, -289.4656767271319495, -325.0550633259551319 ) ) ;
#76276 = CARTESIAN_POINT ( 'NONE',  ( -36.24039811181739168, -300.0457602125951553, -195.0055400566417632 ) ) ;
#76277 = CARTESIAN_POINT ( 'NONE',  ( -111.5509562621303274, -294.6811226260339822, -260.3262643196953832 ) ) ;
#76278 = CARTESIAN_POINT ( 'NONE',  ( 38.09810183088004720, -280.5664172417576196, -255.7667662894656075 ) ) ;
#76279 = CARTESIAN_POINT ( 'NONE',  ( 175.2296996224750103, 150.9142415853029036, 22.83127060016886034 ) ) ;
#76280 = CARTESIAN_POINT ( 'NONE',  ( -18.32587242272214212, -278.2968769681713184, -197.7587295238090519 ) ) ;
#76281 = CARTESIAN_POINT ( 'NONE',  ( 203.4326848949253019, 287.6892256648253010, -4.962899367210394708 ) ) ;
#76282 = CARTESIAN_POINT ( 'NONE',  ( -76.09132718529086503, -288.3774965233114926, -332.6956742695442131 ) ) ;
#76283 = CARTESIAN_POINT ( 'NONE',  ( 196.2226484203252426, 42.37842866446141699, 11.63914608143143603 ) ) ;
#76284 = CARTESIAN_POINT ( 'NONE',  ( 29.33919985515026596, -212.1443419142231051, 54.50000000000000711 ) ) ;
#76285 = CARTESIAN_POINT ( 'NONE',  ( -111.9602290560184770, -288.6489923944097882, -262.8062660380241482 ) ) ;
#76286 = CARTESIAN_POINT ( 'NONE',  ( 0.9564155159336718004, -276.0934487225012504, -207.4011140887274678 ) ) ;
#76287 = CARTESIAN_POINT ( 'NONE',  ( -0.6423713710800299515, -283.9997005014303681, -337.3965796941538429 ) ) ;
#76289 = CARTESIAN_POINT ( 'NONE',  ( -80.62613582809001400, -283.6574293504984894, -329.2071500834630911 ) ) ;
#76288 = CARTESIAN_POINT ( 'NONE',  ( -34.10905316332367221, -296.1125408323349006, -195.0069938773381466 ) ) ;
#76290 = CARTESIAN_POINT ( 'NONE',  ( -43.54978340593097386, -275.3976124971742365, -196.9830950715867175 ) ) ;
#76291 = CARTESIAN_POINT ( 'NONE',  ( -0.4737124017632046158, -275.3585233762697158, -207.1535120387808320 ) ) ;
#76292 = CARTESIAN_POINT ( 'NONE',  ( 24.65590105461573245, -286.2147374318741413, -313.6436417353257298 ) ) ;
#76293 = CARTESIAN_POINT ( 'NONE',  ( 34.56857836002976114, -283.8288064457119049, -291.8452136433186297 ) ) ;
#76294 = CARTESIAN_POINT ( 'NONE',  ( 94.95646885087283806, -298.8069592322501649, -197.1477396936165860 ) ) ;
#76295 = ORIENTED_EDGE ( 'NONE', *, *, #1367, .F. ) ;
#76296 = CARTESIAN_POINT ( 'NONE',  ( 204.5638081195592122, 295.1839629088547099, -54.00000000004283862 ) ) ;
#76297 = CARTESIAN_POINT ( 'NONE',  ( -27.74993937775823127, -294.7670012271443056, -346.8146598934874305 ) ) ;
#76298 = CARTESIAN_POINT ( 'NONE',  ( -106.7338867245362479, -286.1705578667221630, -298.0075384234560829 ) ) ;
#76299 = CARTESIAN_POINT ( 'NONE',  ( -117.3417001280813423, -270.0523547857346784, -270.3292895737509980 ) ) ;
#76300 = CARTESIAN_POINT ( 'NONE',  ( -112.3290637397061573, -277.5392181542181902, -287.1257867821586842 ) ) ;
#76301 = EDGE_CURVE ( 'NONE', #37641, #55239, #48370, .T. ) ;
#76302 = CARTESIAN_POINT ( 'NONE',  ( -111.2139367995613952, -289.1889487258644067, -251.6181641222729013 ) ) ;
#76303 = CARTESIAN_POINT ( 'NONE',  ( -10.70728668976124887, -284.2186311998029851, -339.1270456137751239 ) ) ;
#76304 = CARTESIAN_POINT ( 'NONE',  ( -56.84591985023792660, -279.0671290778715274, -341.8115344093550334 ) ) ;
#76305 = CARTESIAN_POINT ( 'NONE',  ( -63.02063161816173675, -287.1494456575954359, -198.3944675826213029 ) ) ;
#76306 = CARTESIAN_POINT ( 'NONE',  ( -54.98739407203545682, -281.8255670572203826, -197.4128350223410848 ) ) ;
#76307 = CARTESIAN_POINT ( 'NONE',  ( -5.116197397439956163, -274.6314201264449935, -200.4288866561637121 ) ) ;
#76308 = CARTESIAN_POINT ( 'NONE',  ( -110.6673202174979735, -278.0880351509414936, -294.0350054765586378 ) ) ;
#76309 = CARTESIAN_POINT ( 'NONE',  ( -67.86371400210332183, -297.3760549497756642, -338.2700171700143983 ) ) ;
#76310 = TOROIDAL_SURFACE ( 'NONE', #35509, 5.343514653206205445, 1.000000000000000000 ) ;
#76311 = FACE_OUTER_BOUND ( 'NONE', #19035, .T. ) ;
#76312 = FACE_BOUND ( 'NONE', #17529, .T. ) ;
#76313 = CARTESIAN_POINT ( 'NONE',  ( -88.75247875321427671, -295.4795912069792507, -214.6372420201819295 ) ) ;
#76314 = CARTESIAN_POINT ( 'NONE',  ( 5.427738460538985343, -275.9635083976758665, -329.6584063297124771 ) ) ;
#76315 = CARTESIAN_POINT ( 'NONE',  ( -108.8017662732843434, -274.1102221589346755, -242.6203269128297393 ) ) ;
#76316 = CARTESIAN_POINT ( 'NONE',  ( 22.80210275257455876, -288.7165801202618809, -227.1389479497133550 ) ) ;
#76317 = CARTESIAN_POINT ( 'NONE',  ( -37.66642236224352303, -296.5762281189958571, -346.6800571558220554 ) ) ;
#76318 = CARTESIAN_POINT ( 'NONE',  ( -111.9156952345667833, -297.5363409015791376, -287.9314576665448158 ) ) ;
#76319 = CARTESIAN_POINT ( 'NONE',  ( -89.21944715022024752, -293.3208142715086524, -216.3568575459673866 ) ) ;
#76320 = CARTESIAN_POINT ( 'NONE',  ( 12.54651379812971967, -278.7492407441729938, -214.5830350544112832 ) ) ;
#76321 = CARTESIAN_POINT ( 'NONE',  ( -108.6127496141198918, -280.7512964059710043, -248.8727093911112718 ) ) ;
#76322 = CARTESIAN_POINT ( 'NONE',  ( -36.43754930487137500, -296.1434028850160303, -195.9214085030576200 ) ) ;
#76323 = CARTESIAN_POINT ( 'NONE',  ( -76.10523290413317454, -285.4242658231326004, -335.5195081237679915 ) ) ;
#76324 = AXIS2_PLACEMENT_3D ( 'NONE', #38798, #52087, #38334 ) ;
#76325 = CARTESIAN_POINT ( 'NONE',  ( 33.99873784092385165, -286.6941633905929052, -287.2361879103874571 ) ) ;
#76326 = CARTESIAN_POINT ( 'NONE',  ( -11.30266990606949484, -92.55646609309191319, -359.6964084294213535 ) ) ;
#76327 = ORIENTED_EDGE ( 'NONE', *, *, #5345, .F. ) ;
#76328 = CARTESIAN_POINT ( 'NONE',  ( 0.1831703079714151194, -286.2330785186373419, -207.6605550212403557 ) ) ;
#76329 = ORIENTED_EDGE ( 'NONE', *, *, #93158, .T. ) ;
#76330 = CARTESIAN_POINT ( 'NONE',  ( -88.10658806933011533, -284.8224532882052813, -327.9160872133641647 ) ) ;
#76331 = CARTESIAN_POINT ( 'NONE',  ( -109.6043162646397207, -273.0284359234773319, -259.5177243449915636 ) ) ;
#76332 = CARTESIAN_POINT ( 'NONE',  ( -32.31705935647455163, -284.9090872642121326, -193.9100598209185478 ) ) ;
#76333 = CARTESIAN_POINT ( 'NONE',  ( 39.17621167823674000, -282.4162451864140166, -264.2105582314514436 ) ) ;
#76334 = CARTESIAN_POINT ( 'NONE',  ( 195.1541288595761330, 21.00000000164155622, -15.11439585901458749 ) ) ;
#76335 = CARTESIAN_POINT ( 'NONE',  ( -45.22120558338460938, -281.4743272175518882, -194.4098485349325642 ) ) ;
#76336 = CARTESIAN_POINT ( 'NONE',  ( 1.359669952900150802, -280.8873203759857802, -203.7576009053198618 ) ) ;
#76337 = CARTESIAN_POINT ( 'NONE',  ( -21.39648532958014826, -286.3380690714489560, -340.3683826091709079 ) ) ;
#76338 = CARTESIAN_POINT ( 'NONE',  ( 103.6515131172030095, 116.2435397068051088, -283.0600850077821633 ) ) ;
#76339 = EDGE_LOOP ( 'NONE', ( #92653, #13893, #21710, #40117 ) ) ;
#76340 = CARTESIAN_POINT ( 'NONE',  ( -38.12651595029868190, -276.0424522960996683, -195.5318957835380900 ) ) ;
#76341 = CARTESIAN_POINT ( 'NONE',  ( -90.58576820265814433, -230.1752324110255472, -347.6622623265371885 ) ) ;
#76342 = CARTESIAN_POINT ( 'NONE',  ( 25.07136067719763872, -279.0160458490407791, -229.3233031774037158 ) ) ;
#76343 = CARTESIAN_POINT ( 'NONE',  ( 21.41130435408585697, -294.6565257008296044, -222.1733759581961465 ) ) ;
#76344 = CARTESIAN_POINT ( 'NONE',  ( -104.0330092696299715, -295.4965785094855164, -300.4208520403024067 ) ) ;
#76345 = CARTESIAN_POINT ( 'NONE',  ( -111.9333636849018205, -290.2965507470121338, -251.4504278974752367 ) ) ;
#76346 = DIRECTION ( 'NONE',  ( -1.000000000000000000, 6.661338147750933184E-13, 0.000000000000000000 ) ) ;
#76348 = CARTESIAN_POINT ( 'NONE',  ( 36.35281526907292005, -285.8892989160941056, -265.5546851710813598 ) ) ;
#76347 = CARTESIAN_POINT ( 'NONE',  ( -104.7253641013063543, -295.5973557171842003, -234.2204901812115736 ) ) ;
#76349 = CARTESIAN_POINT ( 'NONE',  ( 6.816391997564002381, -296.3050230892768013, -330.0987091538603408 ) ) ;
#76350 = CARTESIAN_POINT ( 'NONE',  ( 33.14768931099136040, -285.9631147065874757, -249.5203077237698608 ) ) ;
#76351 = CARTESIAN_POINT ( 'NONE',  ( -81.79005048671535860, -286.7472863968405932, -211.8325982079589380 ) ) ;
#76352 = ORIENTED_EDGE ( 'NONE', *, *, #10009, .F. ) ;
#76353 = CARTESIAN_POINT ( 'NONE',  ( 36.87217313967585852, -294.7398331294729701, -289.9856237895505160 ) ) ;
#76354 = CARTESIAN_POINT ( 'NONE',  ( -3.587381373274681096, -283.0864185947573333, -335.1720057463320472 ) ) ;
#76355 = CARTESIAN_POINT ( 'NONE',  ( -109.0711666125227310, -295.0035299454532378, -297.3975126226923749 ) ) ;
#76356 = CARTESIAN_POINT ( 'NONE',  ( -104.4738742647615624, -291.8406114335153347, -232.9789027493299614 ) ) ;
#76357 = CARTESIAN_POINT ( 'NONE',  ( -42.05645968822665992, -292.4865624559037656, -193.5672513942529633 ) ) ;
#76358 = CARTESIAN_POINT ( 'NONE',  ( -15.84962372812422515, -288.9330830353967485, -340.1784809887006986 ) ) ;
#76359 = ORIENTED_EDGE ( 'NONE', *, *, #35747, .F. ) ;
#76360 = DIRECTION ( 'NONE',  ( -0.000000000000000000, -0.000000000000000000, 1.000000000000000000 ) ) ;
#76361 = CARTESIAN_POINT ( 'NONE',  ( -95.54703591679596286, -297.7492986057359872, -318.8832864868103911 ) ) ;
#76362 = CARTESIAN_POINT ( 'NONE',  ( -71.21334725666983445, -272.4098462454447827, -201.6536202754759586 ) ) ;
#76363 = CARTESIAN_POINT ( 'NONE',  ( -30.22763583838307966, -279.2029606267645363, -197.4216538472745128 ) ) ;
#76364 = EDGE_CURVE ( 'NONE', #85520, #89916, #12090, .T. ) ;
#76365 = CARTESIAN_POINT ( 'NONE',  ( 31.19832021748437256, -274.6092782823770904, -235.4069692432904617 ) ) ;
#76366 = CARTESIAN_POINT ( 'NONE',  ( -108.8429906471895237, -295.2658498109277616, -252.4692990984672178 ) ) ;
#76367 = CARTESIAN_POINT ( 'NONE',  ( -96.23879224412233668, -279.7873534551964099, -315.5495902241452768 ) ) ;
#76368 = CARTESIAN_POINT ( 'NONE',  ( -29.84191081088734165, -272.2876770118209606, -196.5057279291170005 ) ) ;
#76369 = CARTESIAN_POINT ( 'NONE',  ( -0.5456646725608630399, -295.7569151606389823, -333.9264713786313905 ) ) ;
#76370 = CARTESIAN_POINT ( 'NONE',  ( -104.0053867017158780, -298.0428562477958394, -239.7400475757917775 ) ) ;
#76371 = CARTESIAN_POINT ( 'NONE',  ( 0.000000000000000000, 0.000000000000000000, 12.50000000000000000 ) ) ;
#76372 = CARTESIAN_POINT ( 'NONE',  ( -109.5807499514425132, -297.8437234547807293, -294.6090064566498086 ) ) ;
#76373 = CARTESIAN_POINT ( 'NONE',  ( -36.19303743876654522, -296.0663432834716104, -195.1948331483942525 ) ) ;
#76374 = CARTESIAN_POINT ( 'NONE',  ( 27.25202138763718551, -294.6704687749886489, -304.6971313117701925 ) ) ;
#76375 = CARTESIAN_POINT ( 'NONE',  ( -91.17797276996677169, -289.8427043991016490, -220.1724744300341285 ) ) ;
#76376 = CARTESIAN_POINT ( 'NONE',  ( -22.78264641048746597, -118.9815703160634541, 21.50000000000000000 ) ) ;
#76377 = CARTESIAN_POINT ( 'NONE',  ( 36.00586127399329683, -276.3367125618950126, -293.5917473238491198 ) ) ;
#76378 = CARTESIAN_POINT ( 'NONE',  ( -97.84438154634071338, -273.2876506464223212, -229.4245687950308934 ) ) ;
#76379 = CARTESIAN_POINT ( 'NONE',  ( 35.95453964602150876, -283.7562678607716862, -287.9110375050311745 ) ) ;
#76380 = CARTESIAN_POINT ( 'NONE',  ( 11.16690718817122452, -281.0815913538260133, -329.5922613597094823 ) ) ;
#76381 = CARTESIAN_POINT ( 'NONE',  ( -65.06607605476824574, -276.7534824689196284, -342.1436997471198538 ) ) ;
#76382 = DIRECTION ( 'NONE',  ( -0.9953184226294283787, 0.000000000000000000, 0.09665007798479254009 ) ) ;
#76383 = CARTESIAN_POINT ( 'NONE',  ( -107.1429753769598534, -283.4594581442398180, -292.2787752632311253 ) ) ;
#76384 = VECTOR ( 'NONE', #12726, 1000.000000000000000 ) ;
#76385 = CARTESIAN_POINT ( 'NONE',  ( 34.71374241495128388, -279.8291311979189686, -291.9418742854047082 ) ) ;
#76386 = EDGE_CURVE ( 'NONE', #19742, #4433, #39660, .T. ) ;
#76387 = ADVANCED_FACE ( 'NONE', ( #78164 ), #6190, .T. ) ;
#76388 = CARTESIAN_POINT ( 'NONE',  ( 34.41232581654214329, -273.9124918188405786, -253.9727021139765952 ) ) ;
#76389 = CARTESIAN_POINT ( 'NONE',  ( -69.83462975212601975, -279.4801687198992113, -337.9710042952777940 ) ) ;
#76390 = CARTESIAN_POINT ( 'NONE',  ( 184.7149167944524493, -12.49482340714361506, -3.999999999999998224 ) ) ;
#76391 = FACE_BOUND ( 'NONE', #54158, .T. ) ;
#76392 = CARTESIAN_POINT ( 'NONE',  ( -112.2777488463876097, -271.1302532820440661, -256.2584822934489921 ) ) ;
#76393 =( GEOMETRIC_REPRESENTATION_CONTEXT ( 3 ) GLOBAL_UNCERTAINTY_ASSIGNED_CONTEXT ( ( #4042 ) ) GLOBAL_UNIT_ASSIGNED_CONTEXT ( ( #53027, #89001, #60162 ) ) REPRESENTATION_CONTEXT ( 'NONE', 'WORKASPACE' ) );
#76394 = CARTESIAN_POINT ( 'NONE',  ( -56.43319225364551528, -279.2976468172718683, -343.1165968422513970 ) ) ;
#76395 = LINE ( 'NONE', #18156, #2965 ) ;
#76396 = CARTESIAN_POINT ( 'NONE',  ( -101.3125932882769860, -287.0088790233717759, -230.1486942156624309 ) ) ;
#76397 = ORIENTED_EDGE ( 'NONE', *, *, #5821, .F. ) ;
#76398 = CARTESIAN_POINT ( 'NONE',  ( 156.4851178187871312, 0.000000000000000000, 10.00000000000000000 ) ) ;
#76399 = CARTESIAN_POINT ( 'NONE',  ( 1.411003838963230450, -286.5346415187040634, -334.6332205906015247 ) ) ;
#76400 = VECTOR ( 'NONE', #4696, 1000.000000000000000 ) ;
#76401 = DIRECTION ( 'NONE',  ( 0.000000000000000000, 0.000000000000000000, -1.000000000000000000 ) ) ;
#76402 = CARTESIAN_POINT ( 'NONE',  ( -104.3051457716638595, -294.9430050771975971, -300.5358294888583828 ) ) ;
#76403 = CARTESIAN_POINT ( 'NONE',  ( -18.17709084290268962, -286.9422461581812058, -342.1333677983686812 ) ) ;
#76404 = CARTESIAN_POINT ( 'NONE',  ( 154.2759627658477086, 20.32662787347679512, -12.20915505293937642 ) ) ;
#76405 = CARTESIAN_POINT ( 'NONE',  ( -110.4202099340763965, -294.7685807957072939, -253.4930398996894780 ) ) ;
#76406 = CARTESIAN_POINT ( 'NONE',  ( -95.27734773123958689, -283.7089301923844005, -220.6213565429787025 ) ) ;
#76407 = CARTESIAN_POINT ( 'NONE',  ( 17.64542445061449882, -282.4556523320346741, -221.1385972562944744 ) ) ;
#76408 = CARTESIAN_POINT ( 'NONE',  ( -34.53908727042879434, -281.2572425680131118, -346.2960860593905181 ) ) ;
#76409 = CARTESIAN_POINT ( 'NONE',  ( -75.86873968945332081, -289.5823779850818482, -332.3664985767994153 ) ) ;
#76410 = CARTESIAN_POINT ( 'NONE',  ( -107.7964547180532264, -280.2564945246516572, -249.1125304233597433 ) ) ;
#76411 = CARTESIAN_POINT ( 'NONE',  ( -35.66933598710514275, -280.8764673557497531, -197.2063269233823632 ) ) ;
#76412 = CARTESIAN_POINT ( 'NONE',  ( 37.05530737712214773, -289.6891870490071597, -282.6578220402601573 ) ) ;
#76413 = VERTEX_POINT ( 'NONE', #57329 ) ;
#76414 = CARTESIAN_POINT ( 'NONE',  ( -95.08647638581383887, -273.2418569663221319, -219.4244826898316774 ) ) ;
#76415 = CARTESIAN_POINT ( 'NONE',  ( -97.87809587863021932, -291.9347183658455265, -314.0325227466998399 ) ) ;
#76416 = CARTESIAN_POINT ( 'NONE',  ( 201.0592549708491958, 40.73798607845790798, 10.50000000000000000 ) ) ;
#76417 = CARTESIAN_POINT ( 'NONE',  ( -72.02372285203398405, -291.9805209788416391, -342.4524372437778652 ) ) ;
#76418 = VERTEX_POINT ( 'NONE', #42140 ) ;
#76419 = CARTESIAN_POINT ( 'NONE',  ( 4.821355287580785465, -274.4838739899860798, -332.5889669121688712 ) ) ;
#76420 = DIRECTION ( 'NONE',  ( 0.000000000000000000, 0.000000000000000000, 1.000000000000000000 ) ) ;
#76421 = CARTESIAN_POINT ( 'NONE',  ( -44.73846493661697821, -293.5440239110451444, -346.2541200324676538 ) ) ;
#76422 = CARTESIAN_POINT ( 'NONE',  ( -94.49554268541129431, -296.7020004505471320, -224.8481887995275486 ) ) ;
#76423 = CARTESIAN_POINT ( 'NONE',  ( -13.04115754993245524, -290.2507078279832626, -339.9326019558486109 ) ) ;
#76424 = CARTESIAN_POINT ( 'NONE',  ( -56.56073321752538163, -285.0634416755692087, -341.8356083843844999 ) ) ;
#76425 = CARTESIAN_POINT ( 'NONE',  ( -94.28441374687812981, -292.6738594858829856, -219.4088495424886958 ) ) ;
#76426 = CARTESIAN_POINT ( 'NONE',  ( -34.99244343458124717, -293.3962140497518476, -193.8772780442982366 ) ) ;
#76427 = CARTESIAN_POINT ( 'NONE',  ( -66.56212616720715403, -291.4917541943732431, -203.4644311691167786 ) ) ;
#76428 = CARTESIAN_POINT ( 'NONE',  ( -38.68560912950633224, -288.0354893388805522, -195.3603318999358294 ) ) ;
#76429 = CARTESIAN_POINT ( 'NONE',  ( -72.50870513971767650, -279.7663670681044437, -201.8462346356486705 ) ) ;
#76430 = CARTESIAN_POINT ( 'NONE',  ( -83.32854787231035232, -293.7561426886059053, -330.3814523584369454 ) ) ;
#76431 = CARTESIAN_POINT ( 'NONE',  ( 15.75199781910635899, -282.1583273761293640, -326.1290231143227061 ) ) ;
#76432 = CARTESIAN_POINT ( 'NONE',  ( 23.27598800998567796, -276.8240812207150157, -227.4863352907541412 ) ) ;
#76433 = CARTESIAN_POINT ( 'NONE',  ( -105.5937364680635966, -275.2662352645559167, -254.8156830097664738 ) ) ;
#76434 = CARTESIAN_POINT ( 'NONE',  ( -64.67198163286256829, -275.5446747933210645, -341.0802284867209551 ) ) ;
#76435 = CARTESIAN_POINT ( 'NONE',  ( 154.5564663305860904, 20.34868851667230061, -12.19273113389447083 ) ) ;
#76436 = CARTESIAN_POINT ( 'NONE',  ( 3.419358850103377367, -281.9956956474497360, -331.0566624037581960 ) ) ;
#76437 = CARTESIAN_POINT ( 'NONE',  ( -112.4014579835181138, -279.5640888472843812, -285.7242941006983870 ) ) ;
#76438 = CARTESIAN_POINT ( 'NONE',  ( -107.7056409591531434, -284.0048322855715810, -239.5405368461725288 ) ) ;
#76439 = CARTESIAN_POINT ( 'NONE',  ( -64.46352547408663725, -293.4533958526740776, -201.4824504845877016 ) ) ;
#76440 = CARTESIAN_POINT ( 'NONE',  ( 25.47342839486007549, -276.5767241440461248, -227.2021668403941135 ) ) ;
#76441 = CARTESIAN_POINT ( 'NONE',  ( 6.935854778539218835, -275.9557569601988689, -207.9038340390339386 ) ) ;
#76442 = CARTESIAN_POINT ( 'NONE',  ( -9.990333026611466494, -276.5181379909447514, -338.0570498900360121 ) ) ;
#76443 = CARTESIAN_POINT ( 'NONE',  ( -104.1810135834413984, -298.9992136855112221, -236.5925114287485087 ) ) ;
#76444 = CARTESIAN_POINT ( 'NONE',  ( -102.5773445585654713, -283.0426510456817937, -233.5897554845238346 ) ) ;
#76445 = CARTESIAN_POINT ( 'NONE',  ( 20.36565442307731288, -292.5286107965130213, -219.3941163929616209 ) ) ;
#76446 = CARTESIAN_POINT ( 'NONE',  ( 38.55250176099807646, -289.2384661410605986, -277.1809811570702777 ) ) ;
#76447 = CARTESIAN_POINT ( 'NONE',  ( 35.21563908366541540, -292.3349182322745037, -259.8893177433520236 ) ) ;
#76448 = ORIENTED_EDGE ( 'NONE', *, *, #6509, .T. ) ;
#76449 = CARTESIAN_POINT ( 'NONE',  ( -27.90373146379274871, -290.7443363928971394, -194.4821909894145335 ) ) ;
#76450 = CARTESIAN_POINT ( 'NONE',  ( 22.60771860761217056, -292.6376985038773455, -228.6479026957655094 ) ) ;
#76451 = ORIENTED_EDGE ( 'NONE', *, *, #69493, .T. ) ;
#76452 = CARTESIAN_POINT ( 'NONE',  ( -34.66379058456840312, -290.0989053819855599, -347.0052391598403574 ) ) ;
#76453 = CARTESIAN_POINT ( 'NONE',  ( -109.9245484245452786, -278.7741910939839158, -278.7964727294116756 ) ) ;
#76454 = ADVANCED_FACE ( 'NONE', ( #56870 ), #63508, .F. ) ;
#76455 = CARTESIAN_POINT ( 'NONE',  ( -108.0952018556565690, -295.0930993413451802, -300.0863635499195539 ) ) ;
#76456 = CARTESIAN_POINT ( 'NONE',  ( -95.74458746593975889, -285.8801130297811142, -220.2570947718829473 ) ) ;
#76457 = CARTESIAN_POINT ( 'NONE',  ( 37.80523059895784144, -288.0950207990633771, -287.1151143867770656 ) ) ;
#76458 = CARTESIAN_POINT ( 'NONE',  ( -70.22064498324230897, -283.8310730745346291, -335.5752726161098280 ) ) ;
#76459 = CARTESIAN_POINT ( 'NONE',  ( 202.0776253717283737, 293.7063013533117442, -83.21832582370875286 ) ) ;
#76460 = CARTESIAN_POINT ( 'NONE',  ( -57.39736010472714156, -168.6502712723204240, -363.1223024648248838 ) ) ;
#76461 = CARTESIAN_POINT ( 'NONE',  ( -70.73824396572096873, -195.6031298962179790, -356.6742706091125683 ) ) ;
#76462 = CARTESIAN_POINT ( 'NONE',  ( 22.59225271492110210, -275.3342239518406132, -312.4066643714056681 ) ) ;
#76463 = CARTESIAN_POINT ( 'NONE',  ( 29.43017786110765499, -274.8786252294602832, -300.6223536225385828 ) ) ;
#76464 = CARTESIAN_POINT ( 'NONE',  ( -89.56193029040233000, -296.8474396712807106, -213.7860823365475653 ) ) ;
#76465 = CARTESIAN_POINT ( 'NONE',  ( 66.02812564630266934, 45.92910118373598749, -315.8466591048211285 ) ) ;
#76466 = CARTESIAN_POINT ( 'NONE',  ( 36.81141119533734951, -273.9998289900178747, -251.5299110285778568 ) ) ;
#76467 = CARTESIAN_POINT ( 'NONE',  ( -111.3550334602798699, -274.3120101394163157, -270.3834770935375218 ) ) ;
#76468 = ORIENTED_EDGE ( 'NONE', *, *, #66484, .F. ) ;
#76469 = CARTESIAN_POINT ( 'NONE',  ( -103.9678297180685149, -274.1282815347021256, -232.2748936603652226 ) ) ;
#76470 = VECTOR ( 'NONE', #14534, 1000.000000000000000 ) ;
#76471 = CARTESIAN_POINT ( 'NONE',  ( 23.56425921944132540, -288.6042495599207882, -310.7380619729346449 ) ) ;
#76472 = CARTESIAN_POINT ( 'NONE',  ( -65.53471439865862180, -296.2143623095975045, -341.8547662142683521 ) ) ;
#76473 = CARTESIAN_POINT ( 'NONE',  ( -65.52530806583628475, -298.1858490065776550, -198.7135921590706289 ) ) ;
#76474 = CARTESIAN_POINT ( 'NONE',  ( -10.48802672819066828, -294.8584447510136215, -338.2424867772592165 ) ) ;
#76475 = VERTEX_POINT ( 'NONE', #77689 ) ;
#76476 = CARTESIAN_POINT ( 'NONE',  ( 18.94648717451537223, -276.7748672446655860, -219.8763795095855755 ) ) ;
#76477 = ORIENTED_EDGE ( 'NONE', *, *, #16173, .F. ) ;
#76478 = CARTESIAN_POINT ( 'NONE',  ( -53.74124167373921068, -279.3549166971457680, -195.1362407033382453 ) ) ;
#76479 = CARTESIAN_POINT ( 'NONE',  ( -72.94594343254587443, -278.4774928210591725, -334.3735629527138826 ) ) ;
#76480 = CARTESIAN_POINT ( 'NONE',  ( -20.33085777978403996, -278.5968313288817058, -344.4732414441789956 ) ) ;
#76481 = CARTESIAN_POINT ( 'NONE',  ( -90.19379001330752033, -275.8146220283531989, -324.1470010600972955 ) ) ;
#76482 = CARTESIAN_POINT ( 'NONE',  ( -93.82995333313432695, -273.7005150137832743, -224.0051138216794868 ) ) ;
#76483 = CARTESIAN_POINT ( 'NONE',  ( -97.35281674859676571, -295.7168740479199869, -227.7695601353353538 ) ) ;
#76484 = DIRECTION ( 'NONE',  ( -0.7957555401921984073, -0.6056179655966479336, 0.000000000000000000 ) ) ;
#76485 = CARTESIAN_POINT ( 'NONE',  ( -94.45170733341134905, -278.0764875778563692, -315.8502725316577084 ) ) ;
#76486 = CARTESIAN_POINT ( 'NONE',  ( -38.92685501898818501, -287.7564819854090956, -346.8515458700260865 ) ) ;
#76487 = CARTESIAN_POINT ( 'NONE',  ( -16.36188926982008596, -276.3233417246316890, -198.3013326868602064 ) ) ;
#76488 = DIRECTION ( 'NONE',  ( 0.000000000000000000, 0.000000000000000000, 1.000000000000000000 ) ) ;
#76489 = CARTESIAN_POINT ( 'NONE',  ( -88.78185020040575637, -288.9945901950816278, -322.3852728273838011 ) ) ;
#76490 = CARTESIAN_POINT ( 'NONE',  ( -95.26342772700883188, -283.2157722314795478, -320.9416108504484555 ) ) ;
#76491 = CARTESIAN_POINT ( 'NONE',  ( 1.615889759993562658, -280.7638497990469091, -333.3517107786541374 ) ) ;
#76493 = CARTESIAN_POINT ( 'NONE',  ( -63.03743404493653202, -283.7949028775299212, -200.4416891151780931 ) ) ;
#76492 = CARTESIAN_POINT ( 'NONE',  ( 25.64998266121680714, -279.6062374946538398, -232.2173182046038278 ) ) ;
#76494 = CARTESIAN_POINT ( 'NONE',  ( -63.17603437508145703, -287.7159632494962125, -199.8964818378199766 ) ) ;
#76495 = CARTESIAN_POINT ( 'NONE',  ( -81.53915246214216950, -280.6408812515650197, -211.6993741935708044 ) ) ;
#76496 = CARTESIAN_POINT ( 'NONE',  ( 14.04872217819529112, -294.7731795276428102, -215.6636020820816952 ) ) ;
#76497 = CARTESIAN_POINT ( 'NONE',  ( -47.95478125794594604, -278.1589320212169696, -195.0661304319107785 ) ) ;
#76498 = CARTESIAN_POINT ( 'NONE',  ( 22.55411767426107517, -276.7882349552257324, -312.3572672008701829 ) ) ;
#76499 = CARTESIAN_POINT ( 'NONE',  ( -52.52185957043352715, -285.2461834177107107, -344.0321814315896063 ) ) ;
#76500 = CARTESIAN_POINT ( 'NONE',  ( 198.3171862047178422, 65.26485410360638184, 9.727777467356141017 ) ) ;
#76501 = CARTESIAN_POINT ( 'NONE',  ( -102.5432373721015864, -291.9646349741823883, -308.6492832714856718 ) ) ;
#76502 = CARTESIAN_POINT ( 'NONE',  ( -111.4864994332881167, -294.7012415681579682, -258.7371390073324164 ) ) ;
#76503 = EDGE_CURVE ( 'NONE', #4269, #85072, #19, .T. ) ;
#76504 = CARTESIAN_POINT ( 'NONE',  ( 39.18570460005456368, -286.8358922961920712, -277.2687330363582987 ) ) ;
#76505 = CARTESIAN_POINT ( 'NONE',  ( -82.19932917432734598, -289.8288252163771404, -211.6941314157282363 ) ) ;
#76506 = CARTESIAN_POINT ( 'NONE',  ( 199.2296996224750103, 68.12454877777268791, 0.000000000000000000 ) ) ;
#76507 = CARTESIAN_POINT ( 'NONE',  ( 14.06438449782166522, -274.9971618522870358, -322.9549043105789110 ) ) ;
#76508 = CARTESIAN_POINT ( 'NONE',  ( 28.23833922142655695, -292.1590438555282390, -305.2577342872530721 ) ) ;
#76509 =( LENGTH_UNIT ( ) NAMED_UNIT ( * ) SI_UNIT ( .MILLI., .METRE. ) );
#76510 = CARTESIAN_POINT ( 'NONE',  ( 209.8616357346614905, 36.89613957940296274, 12.09245862095555601 ) ) ;
#76511 = CARTESIAN_POINT ( 'NONE',  ( -33.55424171836384062, -290.5788983845924349, -194.1485014912937856 ) ) ;
#76512 = CARTESIAN_POINT ( 'NONE',  ( -52.27045588907994045, -287.4579419282569006, -198.0868302691719123 ) ) ;
#76513 = CARTESIAN_POINT ( 'NONE',  ( -36.12583683735016393, -287.2770035012818539, -346.3509979411987274 ) ) ;
#76514 = CARTESIAN_POINT ( 'NONE',  ( -97.06356115614984503, -286.5740936262721448, -227.3434023554003147 ) ) ;
#76515 = ADVANCED_FACE ( 'NONE', ( #71535 ), #49269, .F. ) ;
#76516 = CARTESIAN_POINT ( 'NONE',  ( -30.52640065874925668, -286.9432289559196647, -197.4668589413124380 ) ) ;
#76517 = CARTESIAN_POINT ( 'NONE',  ( 38.06566468328554720, -295.5310859627203968, -270.2858865059675395 ) ) ;
#76518 = CARTESIAN_POINT ( 'NONE',  ( -95.95319992546896515, -275.9797408285566576, -318.0679287200999852 ) ) ;
#76519 = CARTESIAN_POINT ( 'NONE',  ( 37.88592085992544867, -276.0904415627179560, -286.7490583984293266 ) ) ;
#76520 = CARTESIAN_POINT ( 'NONE',  ( -47.52466074643158578, -290.0036669445614166, -195.4376326333212717 ) ) ;
#76521 = CARTESIAN_POINT ( 'NONE',  ( -106.1755779162270699, -278.9973941920438847, -235.7329874477496503 ) ) ;
#76522 = CARTESIAN_POINT ( 'NONE',  ( -95.20184817669124300, -297.8789533473575943, -317.5410344465990420 ) ) ;
#76523 = CARTESIAN_POINT ( 'NONE',  ( -43.52490746412112088, -249.8961441073384151, -483.9573757348985055 ) ) ;
#76524 = CARTESIAN_POINT ( 'NONE',  ( 156.1449889021179160, 249.5000000000000568, 16.91223866672558529 ) ) ;
#76525 = CARTESIAN_POINT ( 'NONE',  ( -46.77166153146829686, -284.6148853284377083, -197.4243411303504558 ) ) ;
#76526 = CARTESIAN_POINT ( 'NONE',  ( -109.0189822456722055, -276.4407982536561690, -289.6803496066063985 ) ) ;
#76527 = CARTESIAN_POINT ( 'NONE',  ( 3.436350252227038382, -280.5041807352507135, -333.3681085133127340 ) ) ;
#76528 = DIRECTION ( 'NONE',  ( -0.8195702660915945570, 0.000000000000000000, 0.5729786897769871823 ) ) ;
#76529 = CARTESIAN_POINT ( 'NONE',  ( -15.95297372255607904, -272.8036259670304275, -197.0585413385411471 ) ) ;
#76530 = CIRCLE ( 'NONE', #56892, 5.000000000000004441 ) ;
#76531 = CARTESIAN_POINT ( 'NONE',  ( 36.11709217213325473, -295.1490506209334512, -276.2359443631333988 ) ) ;
#76532 = CARTESIAN_POINT ( 'NONE',  ( 38.11894000997226328, -280.6451961972731510, -284.1155205264357164 ) ) ;
#76533 = CARTESIAN_POINT ( 'NONE',  ( -35.63314603846480111, -295.9714821568629191, -343.5890166210859888 ) ) ;
#76534 = CARTESIAN_POINT ( 'NONE',  ( -112.1195825992270727, -297.6637503386282333, -286.5341377351184633 ) ) ;
#76535 = CARTESIAN_POINT ( 'NONE',  ( 8.930710037563439840, -298.4806182316301602, -197.3624746187491610 ) ) ;
#76536 = CARTESIAN_POINT ( 'NONE',  ( -94.08592463948411933, -293.2324258640568360, -221.3193639787115217 ) ) ;
#76537 = CARTESIAN_POINT ( 'NONE',  ( -12.70571787137886233, -286.5304776923700274, -197.4086102618328482 ) ) ;
#76538 = CARTESIAN_POINT ( 'NONE',  ( 37.01121162820782473, -273.5066983485751280, -255.8026154350708339 ) ) ;
#76539 = CARTESIAN_POINT ( 'NONE',  ( 0.7174463734385814195, -288.3928920754133856, -337.3579173016635764 ) ) ;
#76540 = CARTESIAN_POINT ( 'NONE',  ( 35.91606645810338705, -286.5840264297027602, -268.3178157173430236 ) ) ;
#76541 = CARTESIAN_POINT ( 'NONE',  ( -73.68679976405829279, -289.5694842327730498, -204.7559780725573830 ) ) ;
#76542 = ORIENTED_EDGE ( 'NONE', *, *, #32342, .F. ) ;
#76543 = CARTESIAN_POINT ( 'NONE',  ( -108.4555765497910471, -262.4588243622614527, -317.8183916042563055 ) ) ;
#76544 = CARTESIAN_POINT ( 'NONE',  ( -42.67465990898582362, -288.6287547114201857, -343.2784098232261272 ) ) ;
#76545 = DIRECTION ( 'NONE',  ( 0.000000000000000000, 1.000000000000000000, 0.000000000000000000 ) ) ;
#76546 = CARTESIAN_POINT ( 'NONE',  ( -109.7592728075075712, -285.8156345934768297, -244.8951528555565176 ) ) ;
#76547 = CARTESIAN_POINT ( 'NONE',  ( 1.591137889000544980, -291.6176674398516298, -204.1410555231681769 ) ) ;
#76548 = CARTESIAN_POINT ( 'NONE',  ( 8.053437036477692601, -282.2609072772607988, -209.0932365007826661 ) ) ;
#76549 = CARTESIAN_POINT ( 'NONE',  ( 36.84891077491612066, -282.6320521936957562, -251.6781972200875543 ) ) ;
#76550 = CARTESIAN_POINT ( 'NONE',  ( -34.84866714145898214, -282.8533203320646976, -343.3309722403500359 ) ) ;
#76551 = CARTESIAN_POINT ( 'NONE',  ( 18.76524934551564883, -276.8593582428042055, -220.5146185197979776 ) ) ;
#76552 = CARTESIAN_POINT ( 'NONE',  ( -101.6282676053475029, -295.9937785143127371, -312.8395856388088987 ) ) ;
#76553 = CARTESIAN_POINT ( 'NONE',  ( -106.2110834230515479, -288.9515250770970738, -241.4368797290185569 ) ) ;
#76554 = CARTESIAN_POINT ( 'NONE',  ( -87.59404735942686671, -272.1269183271066368, -216.7954519976267989 ) ) ;
#76555 = ORIENTED_EDGE ( 'NONE', *, *, #80560, .T. ) ;
#76556 = EDGE_LOOP ( 'NONE', ( #33784, #49183 ) ) ;
#76557 = CYLINDRICAL_SURFACE ( 'NONE', #6292, 1.000000000000000888 ) ;
#76558 = CARTESIAN_POINT ( 'NONE',  ( -105.9337740114443989, -286.8545154619316691, -241.3072221966463360 ) ) ;
#76559 = CARTESIAN_POINT ( 'NONE',  ( 34.16824444149040829, -294.9842794391035454, -298.0706891945355892 ) ) ;
#76560 = CARTESIAN_POINT ( 'NONE',  ( -64.08495003180270544, -284.0618858529895192, -338.3956037442119964 ) ) ;
#76561 = CARTESIAN_POINT ( 'NONE',  ( 33.96123670155220964, -274.9744102214193617, -298.9422266537117139 ) ) ;
#76562 = CARTESIAN_POINT ( 'NONE',  ( -95.58914123365204318, -291.8825688328802244, -220.1359251740089462 ) ) ;
#76563 = CARTESIAN_POINT ( 'NONE',  ( -51.91215501165626023, -284.0073354190644750, -195.9570332820456429 ) ) ;
#76564 = CARTESIAN_POINT ( 'NONE',  ( -84.25682486062854082, -291.7602647917484546, -209.2634871296109509 ) ) ;
#76565 = CARTESIAN_POINT ( 'NONE',  ( -108.4490344042040846, -291.1051805550153517, -253.6983097913259542 ) ) ;
#76566 = LINE ( 'NONE', #75164, #92801 ) ;
#76567 = FACE_OUTER_BOUND ( 'NONE', #72404, .T. ) ;
#76568 = CARTESIAN_POINT ( 'NONE',  ( 45.77323534221019941, 10.84377598319223779, -328.4943775524195644 ) ) ;
#76569 = CARTESIAN_POINT ( 'NONE',  ( -97.48588656273726372, -285.4390590387739053, -317.3226404613002956 ) ) ;
#76570 = CARTESIAN_POINT ( 'NONE',  ( -54.49178911615187104, -280.7666405000204009, -345.3538533559490702 ) ) ;
#76571 = ORIENTED_EDGE ( 'NONE', *, *, #56649, .T. ) ;
#76572 = CARTESIAN_POINT ( 'NONE',  ( 32.52172574600692201, -280.7676859438883525, -292.7373300214495657 ) ) ;
#76573 = CARTESIAN_POINT ( 'NONE',  ( -51.31294624711899388, -276.8928262412638901, -346.0615048595248027 ) ) ;
#76574 = CARTESIAN_POINT ( 'NONE',  ( -34.26277092075687136, -282.0910846996497980, -195.5782878711285093 ) ) ;
#76575 = CARTESIAN_POINT ( 'NONE',  ( 162.7603103009924155, 217.9236943496693186, -203.6326850931731371 ) ) ;
#76576 = CARTESIAN_POINT ( 'NONE',  ( 24.12861320391544595, -279.5190817099143601, -224.9738193956834778 ) ) ;
#76577 = CARTESIAN_POINT ( 'NONE',  ( -74.34967771691152905, -283.5776698133333866, -205.5214846736406855 ) ) ;
#76578 = CARTESIAN_POINT ( 'NONE',  ( -29.21748939662639444, -299.9126702956965573, -194.3720490655677224 ) ) ;
#76579 = CARTESIAN_POINT ( 'NONE',  ( -93.12532351689074517, -296.3743056158288027, -317.5628645845365554 ) ) ;
#76580 = ORIENTED_EDGE ( 'NONE', *, *, #46184, .F. ) ;
#76581 = CARTESIAN_POINT ( 'NONE',  ( -107.0336605112414361, -289.5447476143401673, -247.0314344055476568 ) ) ;
#76582 = CARTESIAN_POINT ( 'NONE',  ( 35.10773432549471096, -276.5310751071872346, -296.2939267924919591 ) ) ;
#76583 = CARTESIAN_POINT ( 'NONE',  ( 21.48118147675633338, -274.9464567763436094, -227.1307050802612082 ) ) ;
#76584 = CARTESIAN_POINT ( 'NONE',  ( 38.42816383699886984, -274.6254615369954877, -282.5439436668503390 ) ) ;
#76585 = DIRECTION ( 'NONE',  ( 0.000000000000000000, 1.000000000000000000, 0.000000000000000000 ) ) ;
#76586 = CARTESIAN_POINT ( 'NONE',  ( -75.79491863347708147, -271.5390859265188510, -205.9094166353348498 ) ) ;
#76587 = FACE_OUTER_BOUND ( 'NONE', #36130, .T. ) ;
#76588 = EDGE_CURVE ( 'NONE', #7661, #92724, #34481, .T. ) ;
#76589 = CARTESIAN_POINT ( 'NONE',  ( -43.50899003844633484, -251.6488149788269197, -488.1642653036145703 ) ) ;
#76590 = CARTESIAN_POINT ( 'NONE',  ( 32.53011433091749183, -282.9266804448087669, -292.7111277205769397 ) ) ;
#76591 = CARTESIAN_POINT ( 'NONE',  ( 38.17307873055065670, -283.1993127890175970, -261.4462975323013438 ) ) ;
#76592 = CARTESIAN_POINT ( 'NONE',  ( -89.73012471310292426, -284.6376622228160045, -219.3047079616582096 ) ) ;
#76593 = CARTESIAN_POINT ( 'NONE',  ( 23.10954566211194106, -274.5370568693433029, -312.7818725018061059 ) ) ;
#76594 = CARTESIAN_POINT ( 'NONE',  ( -61.92173439816566827, -285.2353665560385139, -340.4629983659432355 ) ) ;
#76595 = CARTESIAN_POINT ( 'NONE',  ( -41.91880686746605988, -275.5907144707901466, -343.9248900447914821 ) ) ;
#76596 = DIRECTION ( 'NONE',  ( -0.000000000000000000, -0.000000000000000000, -1.000000000000000000 ) ) ;
#76597 = CARTESIAN_POINT ( 'NONE',  ( -24.55598058415324658, -275.2987054726415863, -198.1237777896839702 ) ) ;
#76598 = CARTESIAN_POINT ( 'NONE',  ( 197.3322352251145162, 72.17950364302515709, -11.72475155278582015 ) ) ;
#76599 = CARTESIAN_POINT ( 'NONE',  ( -64.69442686515992591, -280.5068941690625479, -198.4998000430934155 ) ) ;
#76600 = ORIENTED_EDGE ( 'NONE', *, *, #2175, .T. ) ;
#76601 = CARTESIAN_POINT ( 'NONE',  ( 196.7071296363291140, 19.50333209967908843, 12.79999999999999538 ) ) ;
#76602 = CARTESIAN_POINT ( 'NONE',  ( -66.73212955454549444, -287.5315903770040791, -200.5291185837035357 ) ) ;
#76603 = CARTESIAN_POINT ( 'NONE',  ( -45.11803947041191520, -294.3501712361127716, -343.1587358381387958 ) ) ;
#76604 = CARTESIAN_POINT ( 'NONE',  ( -108.2699144452730451, -290.2790998385033845, -240.6541962289265939 ) ) ;
#76605 = CARTESIAN_POINT ( 'NONE',  ( 31.93084578902593407, -285.4472717793988181, -244.1531621404348016 ) ) ;
#76607 = CARTESIAN_POINT ( 'NONE',  ( -111.2562393032154802, -288.8533123169111150, -265.6490732066125133 ) ) ;
#76606 = CARTESIAN_POINT ( 'NONE',  ( -35.90390096878096671, -284.6452615214085426, -196.7859343106696031 ) ) ;
#76608 = CARTESIAN_POINT ( 'NONE',  ( -108.4742786379083270, -285.5197404811117963, -288.4521870626683153 ) ) ;
#76609 = CARTESIAN_POINT ( 'NONE',  ( -7.397242079258217196, -274.6593686441573254, -339.1378552451679980 ) ) ;
#76611 = CARTESIAN_POINT ( 'NONE',  ( 7.094123897701084758, -285.0456621174336647, -208.3937916942269339 ) ) ;
#76610 = B_SPLINE_CURVE_WITH_KNOTS ( 'NONE', 3,
 ( #36921, #65836, #51569, #85703, #57320, #87547 ),
 .UNSPECIFIED., .F., .F.,
 ( 4, 2, 4 ),
 ( 0.000000000000000000, 0.0008512308255186546487, 0.001702461651037309297 ),
 .UNSPECIFIED. ) ;
#76612 = CARTESIAN_POINT ( 'NONE',  ( -37.62631890171964955, -300.0487446769467397, -195.3616536796459116 ) ) ;
#76613 = CARTESIAN_POINT ( 'NONE',  ( 29.79600266233247652, -285.1064498350896201, -236.5593830046665005 ) ) ;
#76614 = CARTESIAN_POINT ( 'NONE',  ( -5.466883223478672171, -281.4233898864263779, -204.4262675901926229 ) ) ;
#76615 = CARTESIAN_POINT ( 'NONE',  ( -72.29812593220761130, -291.5136513980145310, -336.9193165610674896 ) ) ;
#76616 = CARTESIAN_POINT ( 'NONE',  ( 154.7659666677267865, 20.47222690886501439, -12.53936336329526391 ) ) ;
#76617 = CARTESIAN_POINT ( 'NONE',  ( 195.6913163135599234, 40.51256746173211809, 13.63274697749497300 ) ) ;
#76618 = CARTESIAN_POINT ( 'NONE',  ( -30.69284333728993985, -296.8888606969608190, -345.6280224039527411 ) ) ;
#76619 = CARTESIAN_POINT ( 'NONE',  ( -16.33785894445908227, -278.3234877734162183, -198.3622339514360249 ) ) ;
#76620 = CARTESIAN_POINT ( 'NONE',  ( 35.30330697479982405, -292.4312454658624461, -245.1627872002271431 ) ) ;
#76621 = CARTESIAN_POINT ( 'NONE',  ( -106.5490206060877654, -295.2917880932865273, -244.5859655528838630 ) ) ;
#76622 = CARTESIAN_POINT ( 'NONE',  ( 35.05575875174248068, -280.0713080165008364, -257.7178815881530909 ) ) ;
#76623 = CARTESIAN_POINT ( 'NONE',  ( -8.388608893812747880, -272.5138707157639715, -201.7274727217701695 ) ) ;
#76624 = CARTESIAN_POINT ( 'NONE',  ( 9.147930413843498698, -294.0208891608623389, -213.3744949042412884 ) ) ;
#76625 = CARTESIAN_POINT ( 'NONE',  ( -69.85430415644619018, -291.9805209788416391, -337.9475929042657754 ) ) ;
#76626 = CARTESIAN_POINT ( 'NONE',  ( -112.5241843097678043, -294.8635703285478940, -283.7101061273240248 ) ) ;
#76627 = CARTESIAN_POINT ( 'NONE',  ( 38.43227163499855692, -291.7200093274458368, -264.6796379699028989 ) ) ;
#76628 = CARTESIAN_POINT ( 'NONE',  ( -88.35200724408710471, -292.7460186934327453, -217.2499060422842661 ) ) ;
#76629 = DIRECTION ( 'NONE',  ( -0.000000000000000000, -1.000000000000000000, -0.000000000000000000 ) ) ;
#76630 = CARTESIAN_POINT ( 'NONE',  ( -92.68533390788199711, -292.0352914715937231, -222.5104761124463266 ) ) ;
#76632 = CARTESIAN_POINT ( 'NONE',  ( -30.80697332525654275, -292.1370550477507777, -197.6541902135197404 ) ) ;
#76631 = CARTESIAN_POINT ( 'NONE',  ( -35.95529233870315267, -281.0549909850892618, -345.7164044554401698 ) ) ;
#76633 = CARTESIAN_POINT ( 'NONE',  ( 39.41170925864951613, -281.4751448022304885, -264.2036714734219913 ) ) ;
#76634 = CARTESIAN_POINT ( 'NONE',  ( -108.2093362901456715, -283.8346291699731410, -300.5561501315042960 ) ) ;
#76635 = CARTESIAN_POINT ( 'NONE',  ( -28.99326453416362526, -286.9459128857212136, -344.7273203098748127 ) ) ;
#76636 = CARTESIAN_POINT ( 'NONE',  ( 32.54576606641337122, -279.6378196074267066, -239.7269896305699035 ) ) ;
#76637 = CARTESIAN_POINT ( 'NONE',  ( 38.78199126036250988, -286.5947429566154483, -280.0976348922514489 ) ) ;
#76638 = CARTESIAN_POINT ( 'NONE',  ( 195.4695760097934851, 39.54264841588432233, 15.00000000000000000 ) ) ;
#76639 = CARTESIAN_POINT ( 'NONE',  ( 26.92125939201894980, -294.6597212768976419, -233.9702917787960530 ) ) ;
#76640 = CARTESIAN_POINT ( 'NONE',  ( -67.45952374629314363, -278.8648203355996884, -340.5859212533017626 ) ) ;
#76641 = CARTESIAN_POINT ( 'NONE',  ( -102.1727021121564007, -278.6770270542980938, -236.6500620236490704 ) ) ;
#76642 = CARTESIAN_POINT ( 'NONE',  ( 39.65592328351496576, -293.6822302851240352, -267.4344854004200442 ) ) ;
#76643 = CARTESIAN_POINT ( 'NONE',  ( 0.1325363614081735142, -280.6372298423601137, -335.9885296395385126 ) ) ;
#76644 = CARTESIAN_POINT ( 'NONE',  ( 26.44536948771673934, -292.1187500288311298, -234.2767393968833005 ) ) ;
#76645 = CARTESIAN_POINT ( 'NONE',  ( -111.9561552009020744, -294.4544703409337103, -277.9560993184263680 ) ) ;
#76646 = ORIENTED_EDGE ( 'NONE', *, *, #90226, .T. ) ;
#76647 = LINE ( 'NONE', #4211, #12155 ) ;
#76648 = CARTESIAN_POINT ( 'NONE',  ( -10.47319891448835705, -294.1995238890440874, -338.3027994766823099 ) ) ;
#76649 = FACE_OUTER_BOUND ( 'NONE', #11723, .T. ) ;
#76650 = CARTESIAN_POINT ( 'NONE',  ( -21.39648532958014826, -292.3380690714489560, -340.3683826091709079 ) ) ;
#76651 = CARTESIAN_POINT ( 'NONE',  ( 53.25449529029830131, -298.2191232718067226, -193.6104392773155496 ) ) ;
#76652 = CARTESIAN_POINT ( 'NONE',  ( 27.23953207529913101, -280.2189802970960955, -310.0782911197750877 ) ) ;
#76653 = CARTESIAN_POINT ( 'NONE',  ( 28.26696695656664104, -288.3495996160002619, -230.9041700946816604 ) ) ;
#76654 = CARTESIAN_POINT ( 'NONE',  ( 33.08134115626550198, -287.6416882212055270, -289.7735396969575277 ) ) ;
#76655 = CARTESIAN_POINT ( 'NONE',  ( -108.4845937189351446, -279.8207897370473916, -289.5808069834986895 ) ) ;
#76656 = CARTESIAN_POINT ( 'NONE',  ( -81.13979601274394327, -293.6706808318216986, -330.8059159125374435 ) ) ;
#76657 = CARTESIAN_POINT ( 'NONE',  ( -88.84679080605808110, -299.0772781492377135, -217.1369353207897177 ) ) ;
#76658 = CARTESIAN_POINT ( 'NONE',  ( -110.5656749594325987, -277.2718436589311750, -276.0947032256683542 ) ) ;
#76659 = EDGE_LOOP ( 'NONE', ( #1827, #63552, #59773, #5800 ) ) ;
#76660 = CARTESIAN_POINT ( 'NONE',  ( -105.6079596317261320, -272.8462587157188182, -234.6268191249995141 ) ) ;
#76661 = CARTESIAN_POINT ( 'NONE',  ( -81.23730489548655953, -291.5737004659950458, -330.5458750137212292 ) ) ;
#76662 = CARTESIAN_POINT ( 'NONE',  ( 37.00790010273387765, -295.3639497309682724, -287.1107183995169976 ) ) ;
#76663 = CARTESIAN_POINT ( 'NONE',  ( 202.3291156054731346, 292.0658875081724091, -53.99999999997604760 ) ) ;
#76664 = CARTESIAN_POINT ( 'NONE',  ( -109.3786519940150868, -291.3711560438437118, -257.6392874493740237 ) ) ;
#76665 = CARTESIAN_POINT ( 'NONE',  ( -48.18343439338449485, -249.5219462827487860, -456.6705712887342088 ) ) ;
#76666 = ORIENTED_EDGE ( 'NONE', *, *, #28819, .F. ) ;
#76667 = CARTESIAN_POINT ( 'NONE',  ( -80.57457805637038462, -298.1344604248849350, -206.7028221423462924 ) ) ;
#76668 = CARTESIAN_POINT ( 'NONE',  ( -109.2509330367413583, -288.9988741009902355, -246.3356692337193294 ) ) ;
#76669 = CARTESIAN_POINT ( 'NONE',  ( 53.55226604457176620, -299.4943067948125304, -193.3772322354090250 ) ) ;
#76670 = DIRECTION ( 'NONE',  ( 0.000000000000000000, -1.000000000000000000, 0.000000000000000000 ) ) ;
#76671 = FACE_OUTER_BOUND ( 'NONE', #30013, .T. ) ;
#76672 = CARTESIAN_POINT ( 'NONE',  ( -9.795398941516131330, -290.2189021077890629, -341.5222663965483321 ) ) ;
#76673 = CARTESIAN_POINT ( 'NONE',  ( -119.3990491898856732, -281.0519495502701943, -270.3937649182068412 ) ) ;
#76674 = EDGE_CURVE ( 'NONE', #73473, #21018, #6093, .T. ) ;
#76675 = CARTESIAN_POINT ( 'NONE',  ( -111.0020447630474507, -286.7230776743869001, -257.0910900317908272 ) ) ;
#76676 = EDGE_CURVE ( 'NONE', #37419, #20412, #25730, .T. ) ;
#76677 = CARTESIAN_POINT ( 'NONE',  ( 23.40413665144833288, -285.5039181236483046, -223.9872091681073414 ) ) ;
#76678 = CARTESIAN_POINT ( 'NONE',  ( 10.68060858862410001, -272.7169704728086685, -212.9008518456541026 ) ) ;
#76679 = CARTESIAN_POINT ( 'NONE',  ( -70.14716857114906645, -275.5366153623551213, -203.5395986793191412 ) ) ;
#76680 = CARTESIAN_POINT ( 'NONE',  ( -111.5604172484394780, -288.5496116041332471, -276.7292282745677312 ) ) ;
#76681 = CARTESIAN_POINT ( 'NONE',  ( -74.70608869245306494, -279.4043998861710065, -336.2717237171921170 ) ) ;
#76682 = ORIENTED_EDGE ( 'NONE', *, *, #2931, .T. ) ;
#76684 = CARTESIAN_POINT ( 'NONE',  ( -11.69963187783426939, -279.7435149230977345, -201.8504652150937204 ) ) ;
#76683 = CARTESIAN_POINT ( 'NONE',  ( 9.276538532253212566, -280.7132319616817995, -214.1192516020252583 ) ) ;
#76685 = CARTESIAN_POINT ( 'NONE',  ( 23.28217962871956459, -277.2617318547763148, -317.3530255161510922 ) ) ;
#76686 = CARTESIAN_POINT ( 'NONE',  ( 24.28150080872926253, -279.7392426791169555, -224.8573837862583389 ) ) ;
#76687 = CARTESIAN_POINT ( 'NONE',  ( -40.60242197809582620, -139.1959913163171620, -361.5915507396188104 ) ) ;
#76688 = CARTESIAN_POINT ( 'NONE',  ( -3.939357049675801026, -275.4232249478636732, -201.2300602596499743 ) ) ;
#76689 = PRODUCT_CONTEXT ( 'NONE', #54134, 'mechanical' ) ;
#76690 = CARTESIAN_POINT ( 'NONE',  ( -80.87090453512651322, -274.9935689934691254, -207.6239886869931013 ) ) ;
#76691 = CARTESIAN_POINT ( 'NONE',  ( -20.25526795762937127, -294.7662352645559167, -195.3538533559490702 ) ) ;
#76692 = VERTEX_POINT ( 'NONE', #49728 ) ;
#76693 = CARTESIAN_POINT ( 'NONE',  ( 175.2296996224750103, 250.5000000000000568, 0.000000000000000000 ) ) ;
#76694 = CARTESIAN_POINT ( 'NONE',  ( 21.42950459440442401, -289.2442935791040100, -314.2018988088595393 ) ) ;
#76695 = CARTESIAN_POINT ( 'NONE',  ( 26.60432939761541959, -289.8590355010832695, -311.5054610518041613 ) ) ;
#76696 = CARTESIAN_POINT ( 'NONE',  ( -102.9405496951424510, -289.4642245306970381, -302.6207460539445719 ) ) ;
#76697 = CARTESIAN_POINT ( 'NONE',  ( -64.51958215165524280, -285.2143914695812441, -198.3685651946223061 ) ) ;
#76698 = CARTESIAN_POINT ( 'NONE',  ( 196.5998995412811325, 25.70598842973117470, 11.15476524095016941 ) ) ;
#76699 = CARTESIAN_POINT ( 'NONE',  ( 27.54889578111157533, -280.4264633211897149, -305.5129454716814621 ) ) ;
#76700 = CARTESIAN_POINT ( 'NONE',  ( 32.57050280545230692, -289.7394053802656799, -295.3240777454739145 ) ) ;
#76701 = CARTESIAN_POINT ( 'NONE',  ( -3.318327443655574971, -281.0742748396984894, -335.7443440979537286 ) ) ;
#76702 = CARTESIAN_POINT ( 'NONE',  ( -110.8449567856905418, -279.8994717789595370, -267.9084008339096954 ) ) ;
#76703 = CARTESIAN_POINT ( 'NONE',  ( -70.47510922770024422, -277.9936729455083650, -335.4776722777727400 ) ) ;
#76704 = CARTESIAN_POINT ( 'NONE',  ( -107.9949577011233117, -289.7255264533641821, -240.7616938007201099 ) ) ;
#76705 = CARTESIAN_POINT ( 'NONE',  ( -113.6604452798630120, -285.4668030306847868, -261.4387887609575500 ) ) ;
#76706 = CARTESIAN_POINT ( 'NONE',  ( -71.04493448815912870, -286.1115718872038656, -201.1974071419211043 ) ) ;
#76707 = CARTESIAN_POINT ( 'NONE',  ( 32.23196691350072030, -282.0138363489546123, -292.6279110291256416 ) ) ;
#76708 = ORIENTED_EDGE ( 'NONE', *, *, #12553, .F. ) ;
#76709 = CARTESIAN_POINT ( 'NONE',  ( 0.000000000000000000, 3.000000000000000000, 9.000000000000001776 ) ) ;
#76710 = CARTESIAN_POINT ( 'NONE',  ( -102.7203795270322502, -291.9049064666373852, -308.7523481915845878 ) ) ;
#76711 = CARTESIAN_POINT ( 'NONE',  ( 1.464502773491773935, -291.2438057354800662, -204.3659269331617168 ) ) ;
#76712 = CARTESIAN_POINT ( 'NONE',  ( 28.07682607989820767, -274.1655286602704109, -237.4396223276166893 ) ) ;
#76713 = CARTESIAN_POINT ( 'NONE',  ( -86.33675949824396412, -295.0605327958493831, -329.6299710470999003 ) ) ;
#76714 = CARTESIAN_POINT ( 'NONE',  ( -79.91562587690184216, -289.9447944676441580, -210.1473665590815756 ) ) ;
#76716 = ADVANCED_FACE ( 'NONE', ( #85712 ), #27491, .F. ) ;
#76715 = CARTESIAN_POINT ( 'NONE',  ( -17.97665795845529502, -293.0388964498699806, -341.7961874714746955 ) ) ;
#76717 = CARTESIAN_POINT ( 'NONE',  ( -74.90600990107076029, -290.7694777610180381, -333.4318354204780235 ) ) ;
#76718 = CARTESIAN_POINT ( 'NONE',  ( -37.37352853689063892, -300.5519495502701943, -195.3611179825600175 ) ) ;
#76719 = CARTESIAN_POINT ( 'NONE',  ( -54.03111960814487702, -291.2664552906873610, -343.5339230191971751 ) ) ;
#76720 = CARTESIAN_POINT ( 'NONE',  ( -28.04984531623601995, -290.1695408249292427, -195.7185740383867767 ) ) ;
#76721 = CARTESIAN_POINT ( 'NONE',  ( 28.71352174661529588, -296.0250602192240876, -305.9899822279509181 ) ) ;
#76722 = CARTESIAN_POINT ( 'NONE',  ( -11.95161078791422860, -287.3321895460314863, -201.6679464778129045 ) ) ;
#76723 = CARTESIAN_POINT ( 'NONE',  ( -44.59279534605742157, -297.1437322773941787, -345.2293602885483779 ) ) ;
#76724 = CARTESIAN_POINT ( 'NONE',  ( -43.92474550783400389, -275.9493555785821854, -195.2418423320020509 ) ) ;
#76725 = CARTESIAN_POINT ( 'NONE',  ( 16.66434370630601336, -275.0998115301671874, -324.7615546432394353 ) ) ;
#76726 = CARTESIAN_POINT ( 'NONE',  ( 76.10082423805694418, -298.6357017837653984, -193.5375264744100434 ) ) ;
#76727 = CARTESIAN_POINT ( 'NONE',  ( -13.47961245494971472, -274.9780316423373279, -340.4762083061955309 ) ) ;
#76728 = CARTESIAN_POINT ( 'NONE',  ( -21.87173617678286419, -278.3316267423758177, -197.4934392616594607 ) ) ;
#76729 = CARTESIAN_POINT ( 'NONE',  ( -104.7504358689854769, -274.1468479304457446, -241.1944732930645614 ) ) ;
#76730 = CARTESIAN_POINT ( 'NONE',  ( -4.066171927379444107, -273.0570839051138137, -201.5619417268292750 ) ) ;
#76731 = CARTESIAN_POINT ( 'NONE',  ( -109.8595781668697668, -298.1411517136421594, -257.8498317690542194 ) ) ;
#76732 = CARTESIAN_POINT ( 'NONE',  ( 194.7510731661265595, -164.3527196417747689, 21.50000000000000000 ) ) ;
#76733 = CARTESIAN_POINT ( 'NONE',  ( -63.14596986960387426, -298.5102405101060299, -201.8477373004160995 ) ) ;
#76734 = LINE ( 'NONE', #18490, #23184 ) ;
#76736 = CARTESIAN_POINT ( 'NONE',  ( -34.47993613328235796, -298.0889596179500245, -197.3611180422582549 ) ) ;
#76735 = CARTESIAN_POINT ( 'NONE',  ( 11.33375771337099813, -286.4014152028009335, -327.8859526523521595 ) ) ;
#76737 = CARTESIAN_POINT ( 'NONE',  ( 14.60370856817763041, -288.3451503552590225, -327.2723938430602857 ) ) ;
#76738 = CARTESIAN_POINT ( 'NONE',  ( -6.932185464183433510, -288.3306037057610638, -341.0931429864613733 ) ) ;
#76739 = CARTESIAN_POINT ( 'NONE',  ( -105.0467918063214654, -298.9661115425412277, -237.2789874499145526 ) ) ;
#76740 = CARTESIAN_POINT ( 'NONE',  ( 33.26148161316621810, -291.8757249210775626, -295.3197334483541567 ) ) ;
#76741 = CARTESIAN_POINT ( 'NONE',  ( 37.98522367718763348, -280.9393962618596561, -285.5273096958051156 ) ) ;
#76742 = CARTESIAN_POINT ( 'NONE',  ( 169.7306087885279169, 249.5000000000000568, -24.89999999999998792 ) ) ;
#76743 = CARTESIAN_POINT ( 'NONE',  ( -98.79400081414873114, -277.1358528567157578, -227.3435465148481569 ) ) ;
#76744 = DIRECTION ( 'NONE',  ( -0.000000000000000000, -1.000000000000000000, -0.000000000000000000 ) ) ;
#76745 = CARTESIAN_POINT ( 'NONE',  ( -78.40922887016004950, -288.4130594546452926, -331.2547748475975595 ) ) ;
#76746 = CARTESIAN_POINT ( 'NONE',  ( -36.09237171215955442, -55.96374926131388605, -21.50000000000000000 ) ) ;
#76747 = CARTESIAN_POINT ( 'NONE',  ( 206.7809450508160865, 35.77530089738193908, 15.00000000000000000 ) ) ;
#76748 = CARTESIAN_POINT ( 'NONE',  ( -108.8669602638945832, -288.2588691536116698, -293.0971604383435078 ) ) ;
#76749 = CARTESIAN_POINT ( 'NONE',  ( -40.57317446955623552, -299.6110061150338879, -196.6192111055412681 ) ) ;
#76750 = CARTESIAN_POINT ( 'NONE',  ( 36.02881530851531267, -282.7072136894717005, -248.9747617690478876 ) ) ;
#76752 = CARTESIAN_POINT ( 'NONE',  ( -51.01789745730554415, -283.2316833417682460, -342.1201670036364817 ) ) ;
#76751 = CARTESIAN_POINT ( 'NONE',  ( -34.80262803020576712, -296.1038995947365606, -195.0067612199095777 ) ) ;
#76753 = CARTESIAN_POINT ( 'NONE',  ( 13.89399614490957369, -276.2135002198470488, -217.5380326527090915 ) ) ;
#76754 = CARTESIAN_POINT ( 'NONE',  ( 34.53022114635317052, -276.1749785405036732, -256.6852757898665800 ) ) ;
#76755 = CARTESIAN_POINT ( 'NONE',  ( 36.41388865671829222, -285.8419503763049079, -286.8343437386976689 ) ) ;
#76756 = CARTESIAN_POINT ( 'NONE',  ( -27.60581441161320981, -284.9287777069334311, -344.7784973596588998 ) ) ;
#76757 = CARTESIAN_POINT ( 'NONE',  ( -94.00858999500484003, -272.1287512492044698, -223.8324658957658926 ) ) ;
#76758 = ORIENTED_EDGE ( 'NONE', *, *, #47034, .F. ) ;
#76759 = CARTESIAN_POINT ( 'NONE',  ( 204.9737444410070566, 294.0971962920011720, -54.00000000001803357 ) ) ;
#76760 = CARTESIAN_POINT ( 'NONE',  ( 4.225512895823866799, -294.3420781106043478, -335.2403015338224463 ) ) ;
#76761 = CARTESIAN_POINT ( 'NONE',  ( -68.25129945820560806, -287.6240421843597801, -202.4167033829201614 ) ) ;
#76762 = DIRECTION ( 'NONE',  ( 0.000000000000000000, 1.000000000000000000, 0.000000000000000000 ) ) ;
#76763 = CARTESIAN_POINT ( 'NONE',  ( 36.57525178469694538, -273.4809262143061233, -305.9938812882205070 ) ) ;
#76764 = CARTESIAN_POINT ( 'NONE',  ( -96.93565459347829005, -277.0968812586236822, -318.8865642467521297 ) ) ;
#76765 = CARTESIAN_POINT ( 'NONE',  ( -112.5734979646407510, -288.7990036975851922, -282.4696691000957571 ) ) ;
#76766 = CARTESIAN_POINT ( 'NONE',  ( -4.500960683627558190, -284.1313966059612994, -336.3322752199168804 ) ) ;
#76767 = CARTESIAN_POINT ( 'NONE',  ( -48.74211185284015357, -278.9593193771763708, -343.5432709503215847 ) ) ;
#76768 = CARTESIAN_POINT ( 'NONE',  ( -91.99948166029207641, -285.2392658024552929, -323.7571216752605778 ) ) ;
#76769 = CARTESIAN_POINT ( 'NONE',  ( -108.8154649949730697, -283.1274117683187797, -287.1083383910242901 ) ) ;
#76770 = CARTESIAN_POINT ( 'NONE',  ( -34.25585668506585790, -282.0910847014805540, -195.4117360488422435 ) ) ;
#76771 = CARTESIAN_POINT ( 'NONE',  ( -3.828025083772701009, -274.6487784333672835, -201.0224899149199018 ) ) ;
#76772 = CARTESIAN_POINT ( 'NONE',  ( -45.65172708368776000, -276.9878992031458438, -346.9644440313794007 ) ) ;
#76773 = CARTESIAN_POINT ( 'NONE',  ( -110.5540224271688032, -298.2972234404227265, -283.8952634451722474 ) ) ;
#76774 = DIRECTION ( 'NONE',  ( 0.000000000000000000, 0.000000000000000000, -1.000000000000000000 ) ) ;
#76775 = ADVANCED_FACE ( 'NONE', ( #21322 ), #45319, .T. ) ;
#76776 = CARTESIAN_POINT ( 'NONE',  ( 151.6545538274111209, 20.00000000000000000, -4.874605230979886628 ) ) ;
#76777 = CARTESIAN_POINT ( 'NONE',  ( -99.01703812007357897, -294.0983534309256129, -314.4547261793791222 ) ) ;
#76778 = CARTESIAN_POINT ( 'NONE',  ( 25.33184142990839405, -274.5425675952747611, -232.7129368582133964 ) ) ;
#76779 = CARTESIAN_POINT ( 'NONE',  ( -26.27902803094477235, -299.2672730695208543, -193.6682527258752486 ) ) ;
#76780 = CARTESIAN_POINT ( 'NONE',  ( -5.381090812785151556, -288.2386053716709284, -203.5901710489817731 ) ) ;
#76781 = CARTESIAN_POINT ( 'NONE',  ( -83.74806696574948717, -297.1958651192277330, -331.0012908657889739 ) ) ;
#76782 = CARTESIAN_POINT ( 'NONE',  ( 36.71663804834218325, -295.0036142221478599, -289.9409868822082217 ) ) ;
#76783 = ADVANCED_FACE ( 'NONE', ( #43558 ), #72454, .F. ) ;
#76784 = CARTESIAN_POINT ( 'NONE',  ( -100.3725741073241267, -292.0079916845918433, -310.6989085909413575 ) ) ;
#76785 = CARTESIAN_POINT ( 'NONE',  ( -96.21785295733651822, -277.1875605780452361, -224.1493017826633718 ) ) ;
#76786 = CARTESIAN_POINT ( 'NONE',  ( -109.8841469871321834, -280.2555290125474698, -287.1180563634273994 ) ) ;
#76787 = CARTESIAN_POINT ( 'NONE',  ( -108.9954257056843971, -294.3704572154069865, -290.5367917098691350 ) ) ;
#76788 = CARTESIAN_POINT ( 'NONE',  ( -98.77282794680859013, -285.8139437521036825, -314.7942429699178319 ) ) ;
#76789 = CARTESIAN_POINT ( 'NONE',  ( -6.875550828619760857, -285.3819894538563631, -203.6687007221675856 ) ) ;
#76790 = CARTESIAN_POINT ( 'NONE',  ( 201.4006444668590348, 287.9081297433514806, -97.31964668604067015 ) ) ;
#76791 = ORIENTED_EDGE ( 'NONE', *, *, #50265, .T. ) ;
#76792 = CARTESIAN_POINT ( 'NONE',  ( -95.78031251298627069, -284.8332872889211558, -226.5773759157260940 ) ) ;
#76793 = ORIENTED_EDGE ( 'NONE', *, *, #55446, .T. ) ;
#76794 = CARTESIAN_POINT ( 'NONE',  ( 22.62497065170372323, -281.9889408704189009, -222.5334370499905674 ) ) ;
#76795 = CARTESIAN_POINT ( 'NONE',  ( -63.31821001435073981, -274.0374721145117292, -202.1031448226012230 ) ) ;
#76796 = CARTESIAN_POINT ( 'NONE',  ( -54.85882837433268122, -284.6267097088638707, -195.7879395906978175 ) ) ;
#76797 = CARTESIAN_POINT ( 'NONE',  ( 32.95266403754042983, -282.0987973680323080, -239.5143583656991098 ) ) ;
#76798 = CARTESIAN_POINT ( 'NONE',  ( 196.2609727609197421, 20.67721664505789647, -13.53105402382274036 ) ) ;
#76799 = CARTESIAN_POINT ( 'NONE',  ( -25.52224719976205947, -281.7202806909519950, -194.9753880085647495 ) ) ;
#76800 = CARTESIAN_POINT ( 'NONE',  ( 1.315543883392145563, -281.2054010817063840, -203.8254613743454797 ) ) ;
#76801 = CARTESIAN_POINT ( 'NONE',  ( 17.40634833298269157, -290.4094976428775112, -226.7417163044926838 ) ) ;
#76802 = CARTESIAN_POINT ( 'NONE',  ( -21.25639653131470297, -108.7475251564685976, -362.7871151475208649 ) ) ;
#76803 = VERTEX_POINT ( 'NONE', #15152 ) ;
#76804 = CARTESIAN_POINT ( 'NONE',  ( -57.37634452483914771, -275.7932986035743284, -198.2054673961312972 ) ) ;
#76805 = CARTESIAN_POINT ( 'NONE',  ( -108.2462866289636025, -261.9720010280532279, -317.4642910659676431 ) ) ;
#76806 = CARTESIAN_POINT ( 'NONE',  ( 35.54105161292097392, -279.7802643882178586, -286.4841234598790720 ) ) ;
#76808 = AXIS2_PLACEMENT_3D ( 'NONE', #73421, #81424, #30793 ) ;
#76807 = CARTESIAN_POINT ( 'NONE',  ( 34.48727884711513525, -294.9938061797964224, -245.4114250490830784 ) ) ;
#76809 = CARTESIAN_POINT ( 'NONE',  ( -23.50766485369321046, -294.2193438462166455, -342.1937946107894390 ) ) ;
#76810 = CARTESIAN_POINT ( 'NONE',  ( -68.29824766140912118, -291.1639872345078288, -199.9108414600736694 ) ) ;
#76811 = DIRECTION ( 'NONE',  ( -0.000000000000000000, -1.000000000000000000, -0.000000000000000000 ) ) ;
#76813 = CARTESIAN_POINT ( 'NONE',  ( 12.68327238162940951, -286.7408048212066660, -324.6886510975755868 ) ) ;
#76812 = CARTESIAN_POINT ( 'NONE',  ( -113.7198779826033501, -295.1724553898970385, -266.7449246467346029 ) ) ;
#76814 = CARTESIAN_POINT ( 'NONE',  ( 25.88773120472323797, -294.8841451944440450, -231.3675062999054433 ) ) ;
#76815 = CARTESIAN_POINT ( 'NONE',  ( -92.02082268316372904, -285.1690072359671717, -319.4864341692789935 ) ) ;
#76816 = EDGE_LOOP ( 'NONE', ( #18585, #38918, #38490, #56884 ) ) ;
#76817 = CARTESIAN_POINT ( 'NONE',  ( -70.80600167280040580, -292.5626899446709785, -201.2745003467363176 ) ) ;
#76818 = CARTESIAN_POINT ( 'NONE',  ( 7.836929599663928769, -282.9084735145201535, -327.8441974752027477 ) ) ;
#76819 = CARTESIAN_POINT ( 'NONE',  ( -106.8127544581925008, -294.9318585821474130, -302.6377554736166644 ) ) ;
#76820 = CARTESIAN_POINT ( 'NONE',  ( -96.26064320211381187, -290.6895856249560097, -319.7041034888595732 ) ) ;
#76821 = CARTESIAN_POINT ( 'NONE',  ( -36.38543624903908125, -292.5561848099704321, -193.4155772456277020 ) ) ;
#76822 = CARTESIAN_POINT ( 'NONE',  ( 35.45207718627528948, -287.7995411981529514, -276.4792224299424106 ) ) ;
#76823 = ORIENTED_EDGE ( 'NONE', *, *, #91565, .F. ) ;
#76824 = CARTESIAN_POINT ( 'NONE',  ( 180.0056393205866812, 250.0000000000000568, -23.52000000000002800 ) ) ;
#76825 = CARTESIAN_POINT ( 'NONE',  ( -78.78124554001236390, -297.4645748580605300, -333.7887898217801990 ) ) ;
#76826 = CARTESIAN_POINT ( 'NONE',  ( -95.18717095392101157, -295.9184518941388546, -220.2101266073456145 ) ) ;
#76827 = CARTESIAN_POINT ( 'NONE',  ( -66.15125742854300483, -278.7243331120811831, -203.0167755575455999 ) ) ;
#76828 = ORIENTED_EDGE ( 'NONE', *, *, #87492, .T. ) ;
#76829 = CARTESIAN_POINT ( 'NONE',  ( 37.22713366733128026, -274.8225227298822801, -251.4134022930541903 ) ) ;
#76830 = CARTESIAN_POINT ( 'NONE',  ( -109.7230384929604838, -295.2138079905083146, -256.4502442199338930 ) ) ;
#76831 = CARTESIAN_POINT ( 'NONE',  ( -62.18117992897023072, -279.2389104878173498, -340.3719310740302149 ) ) ;
#76832 = CARTESIAN_POINT ( 'NONE',  ( 30.21987882562623895, -273.2824364716808532, -239.4747143198748631 ) ) ;
#76833 = CARTESIAN_POINT ( 'NONE',  ( -53.22040793449946960, -296.4652670279565996, -342.0722775561085314 ) ) ;
#76834 = CARTESIAN_POINT ( 'NONE',  ( -98.71385353567241339, -298.1862380762077009, -230.1732849842972826 ) ) ;
#76835 = LINE ( 'NONE', #27580, #78938 ) ;
#76836 = CARTESIAN_POINT ( 'NONE',  ( -91.08587157039625026, -298.9040373189471325, -216.3425614445917233 ) ) ;
#76837 = CARTESIAN_POINT ( 'NONE',  ( -35.50162904485573989, -296.0749791115317748, -195.1950682159290125 ) ) ;
#76838 = CARTESIAN_POINT ( 'NONE',  ( 4.555284104978047033, -293.2854069631762286, -210.3946854649783518 ) ) ;
#76839 = CARTESIAN_POINT ( 'NONE',  ( -110.3765128903326058, -289.0088883758375573, -279.3772724642715843 ) ) ;
#76840 = CARTESIAN_POINT ( 'NONE',  ( 207.8858603214774519, 30.22477065800575957, 14.36621317371163897 ) ) ;
#76841 = CARTESIAN_POINT ( 'NONE',  ( 1.159191600861030347, -275.0441616628350516, -203.7334727181245171 ) ) ;
#76842 = CARTESIAN_POINT ( 'NONE',  ( -52.64366058546358573, -298.1840897786422033, -198.9093746060461569 ) ) ;
#76843 = CARTESIAN_POINT ( 'NONE',  ( -87.84811519967756510, -281.3301567154842928, -214.4369833275779627 ) ) ;
#76844 = CARTESIAN_POINT ( 'NONE',  ( -74.05416154775977589, -282.2138878511605640, -337.5432072027315371 ) ) ;
#76845 = CARTESIAN_POINT ( 'NONE',  ( -42.80721410208891342, -276.4680116714912970, -347.0647094475549466 ) ) ;
#76846 = CARTESIAN_POINT ( 'NONE',  ( -105.7122109433169470, -284.0962294726536470, -244.3212451426253438 ) ) ;
#76847 = CARTESIAN_POINT ( 'NONE',  ( 35.75931287015413318, -279.7768593501419900, -287.9165212345840246 ) ) ;
#76848 = CARTESIAN_POINT ( 'NONE',  ( -92.44744532713963281, -271.8181609291914924, -221.5888741949748351 ) ) ;
#76849 = CARTESIAN_POINT ( 'NONE',  ( -92.96718084120462322, -279.8506860439898674, -320.6871905074064557 ) ) ;
#76850 = CARTESIAN_POINT ( 'NONE',  ( 0.000000000000000000, 249.5000000000000568, 12.00000000000000000 ) ) ;
#76851 = AXIS2_PLACEMENT_3D ( 'NONE', #83867, #90475, #83385 ) ;
#76852 = CARTESIAN_POINT ( 'NONE',  ( 209.8744251295252354, 28.03846817292548366, 15.00000000000000000 ) ) ;
#76853 = CARTESIAN_POINT ( 'NONE',  ( -48.79482848485816504, -296.1482044836258751, -195.1895873448658563 ) ) ;
#76854 = CARTESIAN_POINT ( 'NONE',  ( 9.406271242195954230, -278.4119172539650435, -329.2889255606859251 ) ) ;
#76855 = CARTESIAN_POINT ( 'NONE',  ( -60.05780265172333543, -271.7577189249084881, -198.8296289754283919 ) ) ;
#76856 = CARTESIAN_POINT ( 'NONE',  ( 138.6539576904058606, 249.5000000000000568, -10.49999999999999822 ) ) ;
#76857 = CARTESIAN_POINT ( 'NONE',  ( -112.1697510040013270, -286.3338913703030926, -281.2215909911712401 ) ) ;
#76858 = VERTEX_POINT ( 'NONE', #16085 ) ;
#76859 = CARTESIAN_POINT ( 'NONE',  ( 159.4572718888394718, 15.48129629386928663, -10.01740370621926068 ) ) ;
#76860 = ADVANCED_FACE ( 'NONE', ( #40040 ), #71805, .T. ) ;
#76861 = CARTESIAN_POINT ( 'NONE',  ( 21.09807492070249779, -286.1990395094103974, -317.3896012640129243 ) ) ;
#76862 = CARTESIAN_POINT ( 'NONE',  ( 206.1364290716512357, 30.05009751731189738, 14.00000000000000000 ) ) ;
#76863 = CARTESIAN_POINT ( 'NONE',  ( -61.15643401280885172, -294.1631289167759178, -339.8411284280082327 ) ) ;
#76864 = CARTESIAN_POINT ( 'NONE',  ( 35.78831485485306985, -285.5224157997286056, -257.3087225269305236 ) ) ;
#76865 = CARTESIAN_POINT ( 'NONE',  ( 24.80950920047307307, -22.49099280560490399, -345.4124233396505019 ) ) ;
#76866 = CARTESIAN_POINT ( 'NONE',  ( -96.86112658669014763, -295.1771302669549186, -224.7064573417206077 ) ) ;
#76867 = CARTESIAN_POINT ( 'NONE',  ( -85.06409488138612573, -283.8868155852132418, -210.8188574452699982 ) ) ;
#76868 = CARTESIAN_POINT ( 'NONE',  ( 24.81511520159434880, -283.6978039692119182, -310.2416662723389891 ) ) ;
#76869 = CARTESIAN_POINT ( 'NONE',  ( 36.69531954020453668, -279.5746205710122467, -253.2014265372545196 ) ) ;
#76870 = CARTESIAN_POINT ( 'NONE',  ( -90.59275651568300702, -289.8329213021414716, -320.3681424121349437 ) ) ;
#76871 = CARTESIAN_POINT ( 'NONE',  ( -9.037352862421002442, -281.8550182730632514, -202.4329291076968218 ) ) ;
#76872 = CARTESIAN_POINT ( 'NONE',  ( 22.23906847704920509, -281.7631645236373288, -227.9025059038118854 ) ) ;
#76873 = CARTESIAN_POINT ( 'NONE',  ( 13.51269787187153248, -290.3247237891447412, -326.0397357310200732 ) ) ;
#76874 = VERTEX_POINT ( 'NONE', #77452 ) ;
#76875 = CARTESIAN_POINT ( 'NONE',  ( -113.5443057820701824, -272.6949299969889466, -258.9447185789064747 ) ) ;
#76876 = CARTESIAN_POINT ( 'NONE',  ( -99.46591255800603903, -291.9699541887025589, -311.7658821380492782 ) ) ;
#76877 = DIRECTION ( 'NONE',  ( 0.000000000000000000, 0.000000000000000000, 1.000000000000000000 ) ) ;
#76878 = CARTESIAN_POINT ( 'NONE',  ( -2.602324593224680793, -291.1233781216987495, -342.4248175857292154 ) ) ;
#76879 = ORIENTED_EDGE ( 'NONE', *, *, #62384, .T. ) ;
#76880 = CARTESIAN_POINT ( 'NONE',  ( -26.07062376046305374, -274.9087881590091911, -344.6779482554795209 ) ) ;
#76881 = CARTESIAN_POINT ( 'NONE',  ( 199.1087447750284980, 64.61450673763175701, 10.46317447812566570 ) ) ;
#76882 = CARTESIAN_POINT ( 'NONE',  ( -81.42565569830419747, -294.0402114871855588, -332.5789765780154426 ) ) ;
#76883 = CARTESIAN_POINT ( 'NONE',  ( -37.14315381731567101, -297.5623635274440630, -197.2967449215204851 ) ) ;
#76884 = CARTESIAN_POINT ( 'NONE',  ( -29.07631924951236257, -290.4656279022099170, -343.5894678942593714 ) ) ;
#76885 = CARTESIAN_POINT ( 'NONE',  ( 6.206154487261058783, -284.2119424452542944, -330.2072404097167464 ) ) ;
#76886 = CARTESIAN_POINT ( 'NONE',  ( -72.92952254726509409, -290.8287756716216563, -338.1017349535645735 ) ) ;
#76887 = CARTESIAN_POINT ( 'NONE',  ( -1.245591803044596935, -288.5307547965683170, -204.5603923112500979 ) ) ;
#76888 = CARTESIAN_POINT ( 'NONE',  ( -42.43217316056491484, -280.1562955310649272, -193.5295678952614935 ) ) ;
#76889 = CARTESIAN_POINT ( 'NONE',  ( -111.4710981498404294, -294.8193518280380658, -255.6609399110392076 ) ) ;
#76890 = CARTESIAN_POINT ( 'NONE',  ( -97.17373675951814960, -283.7352074409558895, -318.8496363182581490 ) ) ;
#76891 = CARTESIAN_POINT ( 'NONE',  ( 24.81499666903957646, -276.8594682637530582, -229.7728127305347527 ) ) ;
#76892 = EDGE_CURVE ( 'NONE', #45087, #60346, #20160, .T. ) ;
#76893 = CARTESIAN_POINT ( 'NONE',  ( 7.450504543161046378, -278.9090924074131408, -326.4764044574609443 ) ) ;
#76894 = CARTESIAN_POINT ( 'NONE',  ( 34.77543551412834688, -273.4847523464841288, -246.2557507969009691 ) ) ;
#76895 = CARTESIAN_POINT ( 'NONE',  ( 222.8344101925596306, 3.000000000000000000, 10.00000000000000000 ) ) ;
#76896 = CARTESIAN_POINT ( 'NONE',  ( -3.114716986823207190, -280.0247965234529488, -205.7984802966873303 ) ) ;
#76897 = CARTESIAN_POINT ( 'NONE',  ( -79.99230248998082971, -278.8200339340047549, -334.0562051560213490 ) ) ;
#76898 = CARTESIAN_POINT ( 'NONE',  ( -30.89164117063817727, -285.1905093387615011, -193.8546159905229729 ) ) ;
#76899 = CARTESIAN_POINT ( 'NONE',  ( 0.4068617851011501196, -294.3226974174677935, -206.6977840534921427 ) ) ;
#76900 = CARTESIAN_POINT ( 'NONE',  ( 35.81202702478421429, -276.8798626843932311, -248.8468140989682809 ) ) ;
#76901 = CARTESIAN_POINT ( 'NONE',  ( -1.547143709048898197, -275.8317809596364327, -202.7441969895050136 ) ) ;
#76902 = DIRECTION ( 'NONE',  ( 0.000000000000000000, 0.000000000000000000, 1.000000000000000000 ) ) ;
#76903 = CARTESIAN_POINT ( 'NONE',  ( 28.02955897725547274, -275.8273870376234527, -302.9650418396694249 ) ) ;
#76904 = CARTESIAN_POINT ( 'NONE',  ( -111.1675064573201439, -298.3948235758292640, -282.5995307722490679 ) ) ;
#76905 = CARTESIAN_POINT ( 'NONE',  ( -30.33487976723781543, -284.1406878903274560, -195.8044598530479163 ) ) ;
#76906 = CARTESIAN_POINT ( 'NONE',  ( 19.40294650657618192, -292.5110035160992084, -218.3439153488016871 ) ) ;
#76907 = CARTESIAN_POINT ( 'NONE',  ( 17.72796013400181181, -274.2794206241090365, -320.7704447901696199 ) ) ;
#76908 = CARTESIAN_POINT ( 'NONE',  ( -3.398592021914435435, -290.2117115917122305, -338.5980691811682277 ) ) ;
#76909 = CARTESIAN_POINT ( 'NONE',  ( -22.66536255689516466, -291.1647678147143097, -198.5361140622206619 ) ) ;
#76910 = ORIENTED_EDGE ( 'NONE', *, *, #72465, .F. ) ;
#76911 = CARTESIAN_POINT ( 'NONE',  ( -11.33658538402526084, -290.9590391734051309, -198.4560753402803925 ) ) ;
#76912 = CARTESIAN_POINT ( 'NONE',  ( -93.45336087039868289, -290.8818502863744584, -223.6129249373564392 ) ) ;
#76913 = EDGE_LOOP ( 'NONE', ( #11834, #4360, #23220, #37944 ) ) ;
#76914 = CARTESIAN_POINT ( 'NONE',  ( 39.26803746374337578, -288.5748367620718113, -265.8229276596409250 ) ) ;
#76915 = CARTESIAN_POINT ( 'NONE',  ( -74.52020881422305365, -279.8764855438762993, -207.4551977821039088 ) ) ;
#76916 = ADVANCED_FACE ( 'NONE', ( #11646, #40493 ), #33417, .F. ) ;
#76917 = CARTESIAN_POINT ( 'NONE',  ( -3.378095802159524652, -293.5346380217991964, -339.1358694524066664 ) ) ;
#76918 = CARTESIAN_POINT ( 'NONE',  ( -109.8838510317794004, -285.5258425320400306, -244.8474132593927095 ) ) ;
#76919 = CARTESIAN_POINT ( 'NONE',  ( 38.00193571307701745, -287.6871997286742157, -254.5150156346946346 ) ) ;
#76921 = CARTESIAN_POINT ( 'NONE',  ( 13.94255196412528619, -282.6418006494040469, -322.4132055708257667 ) ) ;
#76920 = CONICAL_SURFACE ( 'NONE', #30018, 4.025000000000000355, 0.7853981633973095011 ) ;
#76922 = CARTESIAN_POINT ( 'NONE',  ( 64.96643722983849045, 47.89135711549346297, -318.9769533625240570 ) ) ;
#76923 = CARTESIAN_POINT ( 'NONE',  ( 63.56526613329861419, 48.20594201903070797, -317.9086331218617829 ) ) ;
#76924 = CARTESIAN_POINT ( 'NONE',  ( -106.4423271607811898, -259.7000258358197584, -315.5468887844339179 ) ) ;
#76925 = CARTESIAN_POINT ( 'NONE',  ( 35.76273596723413561, -274.8015758187369215, -274.3315634204191724 ) ) ;
#76926 = CARTESIAN_POINT ( 'NONE',  ( 30.55916282461592459, -274.8427078849937288, -298.1312310828664067 ) ) ;
#76927 = CARTESIAN_POINT ( 'NONE',  ( -91.58769398147823892, -296.8118990018231784, -215.8001515871295055 ) ) ;
#76928 = CARTESIAN_POINT ( 'NONE',  ( 203.5338562182570001, 292.0436489450776207, -53.99999999998835420 ) ) ;
#76929 = CARTESIAN_POINT ( 'NONE',  ( 23.25258900297250975, -273.6094030875871681, -223.6318617462921168 ) ) ;
#76930 = CARTESIAN_POINT ( 'NONE',  ( -49.05764131074640488, -275.6611343120919173, -197.2290659742096750 ) ) ;
#76931 = ORIENTED_EDGE ( 'NONE', *, *, #86325, .T. ) ;
#76932 = CARTESIAN_POINT ( 'NONE',  ( -76.28764799197409729, -274.6243320108757189, -204.2338312892161696 ) ) ;
#76933 = CARTESIAN_POINT ( 'NONE',  ( 22.80412073339321211, -288.6219400024127708, -311.8617054626722052 ) ) ;
#76934 = CARTESIAN_POINT ( 'NONE',  ( -97.27504928186945676, -296.7091223177130814, -318.4667847877851159 ) ) ;
#76935 = CARTESIAN_POINT ( 'NONE',  ( -114.2484962686692285, -297.0897662265755343, -266.7444304478437971 ) ) ;
#76936 = CARTESIAN_POINT ( 'NONE',  ( -4.834986371183608966, -292.6592369659877022, -204.9842562496372125 ) ) ;
#76937 = ORIENTED_EDGE ( 'NONE', *, *, #4015, .F. ) ;
#76938 = CARTESIAN_POINT ( 'NONE',  ( 33.85256884787933984, -277.7996115248241722, -295.8273437185206376 ) ) ;
#76939 = ORIENTED_EDGE ( 'NONE', *, *, #42150, .T. ) ;
#76940 = CARTESIAN_POINT ( 'NONE',  ( -25.39895610655716851, -279.7081356066872786, -194.3552118414999939 ) ) ;
#76941 = PRODUCT_DEFINITION_CONTEXT ( 'detailed design', #929, 'design' ) ;
#76942 = CARTESIAN_POINT ( 'NONE',  ( -93.77971946704622042, -278.8336875194699473, -317.0515070767875727 ) ) ;
#76943 = CARTESIAN_POINT ( 'NONE',  ( 0.5612836321380542115, -278.3147380947766010, -336.2792770800451194 ) ) ;
#76944 = CARTESIAN_POINT ( 'NONE',  ( -112.7317043466922399, -276.5929248515249697, -268.7438369969278256 ) ) ;
#76945 = CARTESIAN_POINT ( 'NONE',  ( -35.82122951370943298, -298.7230955458567792, -197.2590104329121345 ) ) ;
#76946 = CARTESIAN_POINT ( 'NONE',  ( -45.17132622571710243, -293.7278318508057282, -343.5835260978550423 ) ) ;
#76947 = CARTESIAN_POINT ( 'NONE',  ( 151.9308040602113579, 19.99432900746804620, -6.268121358087393347 ) ) ;
#76948 = CARTESIAN_POINT ( 'NONE',  ( 21.01532648003455250, -281.3669807022101850, -220.2014386207109169 ) ) ;
#76949 = CARTESIAN_POINT ( 'NONE',  ( -109.6221191285575571, -278.8583394546413388, -259.7857695774932836 ) ) ;
#76950 = CARTESIAN_POINT ( 'NONE',  ( -62.61664176052439501, -288.0590141791712426, -342.6284718934915077 ) ) ;
#76951 = CARTESIAN_POINT ( 'NONE',  ( -105.0489245893652566, -274.9768893035542305, -238.1007335866977996 ) ) ;
#76952 = DIRECTION ( 'NONE',  ( 0.000000000000000000, -0.000000000000000000, 1.000000000000000000 ) ) ;
#76953 = CARTESIAN_POINT ( 'NONE',  ( -34.58213057077002617, -288.2138975673685195, -343.5202244982656907 ) ) ;
#76954 = CARTESIAN_POINT ( 'NONE',  ( -39.71153009679694179, -278.2618745588158617, -196.3730369288573456 ) ) ;
#76956 = CARTESIAN_POINT ( 'NONE',  ( -26.55786663609574916, -280.9938753476183706, -344.0681837657413666 ) ) ;
#76955 = CARTESIAN_POINT ( 'NONE',  ( -66.28486608250479151, -278.2403910190682268, -202.6889043120860094 ) ) ;
#76957 = CARTESIAN_POINT ( 'NONE',  ( -90.85243905842411039, -287.2935666412539604, -217.7371416735708181 ) ) ;
#76958 = CARTESIAN_POINT ( 'NONE',  ( -87.81475920902107646, -280.5331210238073254, -217.0029608360344753 ) ) ;
#76959 = CARTESIAN_POINT ( 'NONE',  ( 197.3748232817348764, 215.0000000000000568, -12.45182892472558933 ) ) ;
#76960 = CARTESIAN_POINT ( 'NONE',  ( -87.33576820686256781, -293.3551532516469820, -214.4541076612754296 ) ) ;
#76961 = CARTESIAN_POINT ( 'NONE',  ( -53.93212986229021055, -275.5020100719474385, -344.5684756188985602 ) ) ;
#76962 = CARTESIAN_POINT ( 'NONE',  ( -53.96906400489967837, -277.9225782758521177, -341.5991676687450536 ) ) ;
#76963 = CARTESIAN_POINT ( 'NONE',  ( -55.24034981963281155, -285.2820377730427595, -343.3656847075271799 ) ) ;
#76964 = CARTESIAN_POINT ( 'NONE',  ( 196.0143093133015384, 73.40565171261611965, 12.00000000000000711 ) ) ;
#76965 = CARTESIAN_POINT ( 'NONE',  ( -105.2091565635610806, -292.0362512703659945, -303.6962708431841520 ) ) ;
#76966 = CARTESIAN_POINT ( 'NONE',  ( -80.93773930535884631, -293.6434239255821126, -331.4519757971451099 ) ) ;
#76967 = CARTESIAN_POINT ( 'NONE',  ( 27.00812565924913500, -286.1965218845581376, -228.3699434157463486 ) ) ;
#76968 = DIRECTION ( 'NONE',  ( 0.000000000000000000, 0.000000000000000000, 1.000000000000000000 ) ) ;
#76969 = CARTESIAN_POINT ( 'NONE',  ( 21.88849600603380452, -273.6314953436670976, -226.8521839007555343 ) ) ;
#76970 = CARTESIAN_POINT ( 'NONE',  ( 33.92952733776302665, -291.9624114762742693, -291.1739805902424223 ) ) ;
#76971 = CARTESIAN_POINT ( 'NONE',  ( 175.2296996224750103, 250.0000000000000568, -24.00000000000000355 ) ) ;
#76972 = CARTESIAN_POINT ( 'NONE',  ( -111.9578785049571223, -289.2343554908222814, -254.3266412939698000 ) ) ;
#76973 = CARTESIAN_POINT ( 'NONE',  ( -30.47694198535674559, -287.7403961922369717, -196.8297286551571972 ) ) ;
#76974 = CARTESIAN_POINT ( 'NONE',  ( 25.53167739099729516, -285.2216615680111431, -227.6657143534044110 ) ) ;
#76975 = EDGE_CURVE ( 'NONE', #32191, #77282, #28804, .T. ) ;
#76976 = CARTESIAN_POINT ( 'NONE',  ( -109.2923710593129840, -285.7745612175551173, -285.8635637361780937 ) ) ;
#76977 = CARTESIAN_POINT ( 'NONE',  ( 202.9738562182569694, 293.9636489450776367, -54.00000000000000000 ) ) ;
#76978 = CARTESIAN_POINT ( 'NONE',  ( -89.78572593098405719, -286.0916735583547847, -219.2763901724217135 ) ) ;
#76979 = CARTESIAN_POINT ( 'NONE',  ( 34.80249007755185886, -295.8132040623688113, -292.3009547389195291 ) ) ;
#76980 = AXIS2_PLACEMENT_3D ( 'NONE', #25715, #34246, #63152 ) ;
#76981 = CARTESIAN_POINT ( 'NONE',  ( 9.611743351465115381, -274.4922335098502231, -329.6283208015555033 ) ) ;
#76982 = CARTESIAN_POINT ( 'NONE',  ( 38.71553715295499387, -276.0381860407999852, -282.5718503297363213 ) ) ;
#76983 = CARTESIAN_POINT ( 'NONE',  ( -30.79715606001322215, -290.2139746343372622, -195.0333000752978592 ) ) ;
#76984 = CARTESIAN_POINT ( 'NONE',  ( -110.5496847997783476, -278.8543007676240109, -246.3257844339869962 ) ) ;
#76985 = CARTESIAN_POINT ( 'NONE',  ( -96.90184065772848498, -297.9136378316295009, -315.3759034152589606 ) ) ;
#76986 = CARTESIAN_POINT ( 'NONE',  ( 212.3569123273291268, -147.7221692137691775, -10.75739200365177695 ) ) ;
#76987 = CARTESIAN_POINT ( 'NONE',  ( 207.8033511093241827, 36.73028256270350766, 13.58522159759119852 ) ) ;
#76988 = CARTESIAN_POINT ( 'NONE',  ( -19.68124197500630501, -284.9688554521978290, -199.0214257039185100 ) ) ;
#76989 = CARTESIAN_POINT ( 'NONE',  ( 22.17613448769722240, -278.9268243360425004, -224.7043097940381529 ) ) ;
#76990 = CARTESIAN_POINT ( 'NONE',  ( 196.0143093133015384, 20.19615242270663913, -11.99999999999998579 ) ) ;
#76991 = CARTESIAN_POINT ( 'NONE',  ( 38.44658308318671658, -274.1496698841874036, -279.6825883453341817 ) ) ;
#76992 = CARTESIAN_POINT ( 'NONE',  ( -36.47327549706410110, -276.3896055142875525, -343.4703777290328048 ) ) ;
#76993 = CARTESIAN_POINT ( 'NONE',  ( 19.37902799195334680, -295.7332439217461797, -317.4086126645106560 ) ) ;
#76994 = CARTESIAN_POINT ( 'NONE',  ( 39.10468502056978934, -280.3956473024632601, -264.2420733834683801 ) ) ;
#76995 = CARTESIAN_POINT ( 'NONE',  ( -38.33349419775058209, -296.0061404914874856, -343.5896970578966716 ) ) ;
#76996 = CARTESIAN_POINT ( 'NONE',  ( -32.02992129025761869, -296.3016590936503576, -346.6965208343950735 ) ) ;
#76997 = CARTESIAN_POINT ( 'NONE',  ( -75.20882932078620797, -297.3658662381225781, -207.8919318826508800 ) ) ;
#76998 = CARTESIAN_POINT ( 'NONE',  ( -60.91100295596007186, -293.7465757119263117, -199.1062761145201989 ) ) ;
#76999 = CARTESIAN_POINT ( 'NONE',  ( -63.20343213100047564, -285.8910563097514341, -197.8340828693793583 ) ) ;
#77000 = CARTESIAN_POINT ( 'NONE',  ( 9.739654017775013273, -274.5519620265484377, -329.7884476712060291 ) ) ;
#77001 = CARTESIAN_POINT ( 'NONE',  ( 35.07174509385883709, -287.7178248370943834, -296.6943353081996975 ) ) ;
#77002 = CARTESIAN_POINT ( 'NONE',  ( -96.10090313381023464, -281.1669683924969263, -224.3057348175780419 ) ) ;
#77003 = ADVANCED_FACE ( 'NONE', ( #42385 ), #63745, .T. ) ;
#77004 = CARTESIAN_POINT ( 'NONE',  ( 33.61952280722571373, -286.3720464971211754, -252.2020916793732965 ) ) ;
#77005 = CARTESIAN_POINT ( 'NONE',  ( -41.90611935587904924, -289.9944572538296939, -195.5001353075423083 ) ) ;
#77006 = ORIENTED_EDGE ( 'NONE', *, *, #78174, .F. ) ;
#77007 = CARTESIAN_POINT ( 'NONE',  ( 81.08292338999881110, 82.25620239566015357, -296.3357184930298445 ) ) ;
#77008 = CARTESIAN_POINT ( 'NONE',  ( 35.71665683933490243, -287.0687889237887020, -271.0429674359417049 ) ) ;
#77009 = LINE ( 'NONE', #61871, #56561 ) ;
#77010 = CARTESIAN_POINT ( 'NONE',  ( 15.59995472104877301, -283.2660809251399883, -325.9488989629570028 ) ) ;
#77011 = CARTESIAN_POINT ( 'NONE',  ( -105.7888645952828597, -290.0610408584786910, -235.4904470152518456 ) ) ;
#77012 = CARTESIAN_POINT ( 'NONE',  ( 23.93614727145840959, -282.5439933668443473, -225.0680077438634612 ) ) ;
#77013 = CARTESIAN_POINT ( 'NONE',  ( -9.059085678266479036, -281.7295696065875177, -199.2739039927778322 ) ) ;
#77014 = CARTESIAN_POINT ( 'NONE',  ( 17.06422943565276285, -280.6891292655526513, -221.6887969692598688 ) ) ;
#77015 = CARTESIAN_POINT ( 'NONE',  ( 34.82919090812784901, -277.8154144086593647, -290.8131523905287281 ) ) ;
#77016 = CARTESIAN_POINT ( 'NONE',  ( -39.10783922643397403, -295.0737427575077731, -347.3408604651460792 ) ) ;
#77017 = CARTESIAN_POINT ( 'NONE',  ( -112.0125344030138450, -288.5976342690941010, -268.3938059634269280 ) ) ;
#77018 = CARTESIAN_POINT ( 'NONE',  ( -110.7382015680781535, -271.3832025871527094, -267.6071348884254917 ) ) ;
#77019 = ORIENTED_EDGE ( 'NONE', *, *, #43760, .F. ) ;
#77020 = CARTESIAN_POINT ( 'NONE',  ( -87.88906082301696188, -285.6850755159490518, -325.0784697405596830 ) ) ;
#77021 = CARTESIAN_POINT ( 'NONE',  ( -64.14522180977439803, -296.4734619401404530, -342.2155801616106032 ) ) ;
#77022 = CARTESIAN_POINT ( 'NONE',  ( -73.84050084666280611, -284.2016409813550695, -333.7570198402976303 ) ) ;
#77023 = ADVANCED_FACE ( 'NONE', ( #27743 ), #45448, .T. ) ;
#77024 = CARTESIAN_POINT ( 'NONE',  ( 28.30756358580422472, -274.0888206018845494, -230.4726114452056720 ) ) ;
#77025 = CARTESIAN_POINT ( 'NONE',  ( -114.0101373136554770, -291.1210124710574405, -276.9531225384577056 ) ) ;
#77026 = CARTESIAN_POINT ( 'NONE',  ( -84.72173070950167073, -283.5465763757330251, -211.2388871393937961 ) ) ;
#77027 = CARTESIAN_POINT ( 'NONE',  ( 29.45518768648751973, -293.3881812978008838, -232.0999095627983877 ) ) ;
#77028 = CARTESIAN_POINT ( 'NONE',  ( 20.37678908275908896, -288.5154087295122167, -315.1101416684124956 ) ) ;
#77029 = DIRECTION ( 'NONE',  ( -0.000000000000000000, -0.000000000000000000, -1.000000000000000000 ) ) ;
#77030 = CARTESIAN_POINT ( 'NONE',  ( -69.88240323175847379, -196.0786339892123635, -356.6774816750892114 ) ) ;
#77031 = CARTESIAN_POINT ( 'NONE',  ( 0.5411208059672262261, -284.0769505835842210, -336.6151734898739392 ) ) ;
#77032 = CARTESIAN_POINT ( 'NONE',  ( -69.85430415644619018, -289.1237833571632905, -202.7746430608542312 ) ) ;
#77033 = ORIENTED_EDGE ( 'NONE', *, *, #78611, .T. ) ;
#77034 = CARTESIAN_POINT ( 'NONE',  ( 20.41605115271496018, -281.1061830307352807, -315.5083021875493046 ) ) ;
#77035 = CARTESIAN_POINT ( 'NONE',  ( -56.92274980391026418, -276.9645806723872852, -344.8629614518559947 ) ) ;
#77036 = CARTESIAN_POINT ( 'NONE',  ( -82.41185862518261729, -281.4358380463647222, -210.5573600565763570 ) ) ;
#77037 = CARTESIAN_POINT ( 'NONE',  ( -37.46162067202239854, -140.9052193018087848, -362.9178459242288568 ) ) ;
#77038 = CARTESIAN_POINT ( 'NONE',  ( 37.10754630562437484, -279.9094352774340564, -253.1013608149115157 ) ) ;
#77039 = CARTESIAN_POINT ( 'NONE',  ( -99.46222977079803229, -283.1341647278430855, -228.9740837855790687 ) ) ;
#77040 = CARTESIAN_POINT ( 'NONE',  ( -112.9501668877829417, -274.4839910648973387, -264.7418366708396888 ) ) ;
#77041 = CARTESIAN_POINT ( 'NONE',  ( 33.36617924567667615, -293.8018475188829939, -251.9658947903538149 ) ) ;
#77042 = VERTEX_POINT ( 'NONE', #76986 ) ;
#77043 = CARTESIAN_POINT ( 'NONE',  ( -77.51078714589368701, -290.1854006632938194, -208.8169230859111281 ) ) ;
#77044 = CARTESIAN_POINT ( 'NONE',  ( -37.11892092752835737, -277.7008061531869885, -347.2719043138369557 ) ) ;
#77045 = CARTESIAN_POINT ( 'NONE',  ( 2.929940339339094812, -274.6090749914681055, -209.4139665111396198 ) ) ;
#77046 = CARTESIAN_POINT ( 'NONE',  ( -87.82252213641214666, -272.2865916653408931, -212.5568331142568468 ) ) ;
#77047 = FILL_AREA_STYLE ('',( #63341 ) ) ;
#77048 = CARTESIAN_POINT ( 'NONE',  ( -102.5945760320706910, -271.0459574960322016, -233.2837800218109976 ) ) ;
#77049 = ADVANCED_FACE ( 'NONE', ( #26324 ), #62809, .F. ) ;
#77050 = CIRCLE ( 'NONE', #31694, 5.000000000000004441 ) ;
#77051 = CARTESIAN_POINT ( 'NONE',  ( -43.53958148833284270, -248.2611259770202139, -477.2465563938658306 ) ) ;
#77052 = CARTESIAN_POINT ( 'NONE',  ( 34.63512194200365002, -282.4482011167932001, -256.3823509844918931 ) ) ;
#77053 = CARTESIAN_POINT ( 'NONE',  ( 33.64889274247908446, -283.6599195083750828, -297.4592680287849475 ) ) ;
#77054 = CARTESIAN_POINT ( 'NONE',  ( -108.5264572406010615, -283.6809846479206385, -287.0478253691944133 ) ) ;
#77055 = CARTESIAN_POINT ( 'NONE',  ( -21.74530855578876398, -272.6552654742687309, -198.2279565175680602 ) ) ;
#77056 = CARTESIAN_POINT ( 'NONE',  ( 35.26847523724462974, -283.2114244290195870, -254.8530575296113625 ) ) ;
#77057 = CARTESIAN_POINT ( 'NONE',  ( 31.77524096876192061, -273.6943458334019965, -244.7963726310247239 ) ) ;
#77058 = CARTESIAN_POINT ( 'NONE',  ( -23.40286736638519471, -122.5496321078137356, -22.50000000000000000 ) ) ;
#77059 = CARTESIAN_POINT ( 'NONE',  ( -2.780021451133341870, -275.6001369539969232, -205.7103914492528816 ) ) ;
#77060 = DIRECTION ( 'NONE',  ( 0.000000000000000000, 1.000000000000000000, 0.000000000000000000 ) ) ;
#77061 = CARTESIAN_POINT ( 'NONE',  ( -38.17842532867272354, -280.8447442492000619, -193.5271495036795670 ) ) ;
#77062 = ORIENTED_EDGE ( 'NONE', *, *, #25784, .T. ) ;
#77063 = CARTESIAN_POINT ( 'NONE',  ( 113.5000000000000568, -298.0521521680024080, -397.9547385950631337 ) ) ;
#77064 = CARTESIAN_POINT ( 'NONE',  ( -106.8033311858618362, -286.8060493221394154, -239.9744768840502331 ) ) ;
#77065 = CARTESIAN_POINT ( 'NONE',  ( 8.320992971831785212, -293.6061957033166436, -327.5884466100519035 ) ) ;
#77066 = CARTESIAN_POINT ( 'NONE',  ( -111.4459647421723503, -289.6430735994253496, -290.9006104981398835 ) ) ;
#77067 = CARTESIAN_POINT ( 'NONE',  ( 30.90472853489130145, -285.4113809929067997, -241.5856899920826493 ) ) ;
#77069 = CARTESIAN_POINT ( 'NONE',  ( -103.3026222840980495, -289.2430941396015101, -236.6749666403671597 ) ) ;
#77068 = CARTESIAN_POINT ( 'NONE',  ( -37.26215787424501258, -284.6278565616020160, -196.7593913820396097 ) ) ;
#77070 = CARTESIAN_POINT ( 'NONE',  ( -104.4703060873563345, -285.3599628368435788, -300.0407535202740519 ) ) ;
#77071 = CARTESIAN_POINT ( 'NONE',  ( -12.55191763875878586, -274.7297834185234819, -341.2002388274104874 ) ) ;
#77072 = CARTESIAN_POINT ( 'NONE',  ( 35.92770749046399459, -285.6847741258068254, -249.2443098591791397 ) ) ;
#77073 = CARTESIAN_POINT ( 'NONE',  ( -107.9760697139818859, -298.8790747096514906, -245.1463112088183891 ) ) ;
#77074 = CARTESIAN_POINT ( 'NONE',  ( 24.06252069718013331, -284.9640712522170247, -226.9851382692413608 ) ) ;
#77075 = CARTESIAN_POINT ( 'NONE',  ( 22.29816566643246034, -281.9015615755041608, -227.8582374154853198 ) ) ;
#77076 = CARTESIAN_POINT ( 'NONE',  ( 11.25051781303261045, -290.3808272807742696, -327.7093941479237174 ) ) ;
#77077 = DIRECTION ( 'NONE',  ( 1.000000000000000000, -1.805997381456195657E-15, 0.000000000000000000 ) ) ;
#77078 = FACE_OUTER_BOUND ( 'NONE', #55348, .T. ) ;
#77079 = CARTESIAN_POINT ( 'NONE',  ( -25.11624519921462451, -296.8177311834359102, -344.9785932560251354 ) ) ;
#77080 = CARTESIAN_POINT ( 'NONE',  ( -97.19280280957008245, -277.1702440446872515, -225.1419538124783628 ) ) ;
#77081 = CARTESIAN_POINT ( 'NONE',  ( 4.063150868354068024, -291.7915996332590112, -205.5694027574573113 ) ) ;
#77082 = CARTESIAN_POINT ( 'NONE',  ( -93.33825809041043442, -295.6291448942171201, -222.2706361474565995 ) ) ;
#77083 = CARTESIAN_POINT ( 'NONE',  ( 18.34910599065556980, -279.5584106096611663, -222.3857979285616580 ) ) ;
#77084 = CARTESIAN_POINT ( 'NONE',  ( 1.382029900557905089, -272.6537274690363688, -206.7860683948709379 ) ) ;
#77085 = CARTESIAN_POINT ( 'NONE',  ( 27.91680234231528601, -294.4107225774616836, -236.5591752580010620 ) ) ;
#77086 = CARTESIAN_POINT ( 'NONE',  ( -20.25526795762937127, -288.7662352645559736, -195.3538533559490702 ) ) ;
#77087 = CARTESIAN_POINT ( 'NONE',  ( -72.93978587911213651, -296.0694712879067652, -202.8084855493224836 ) ) ;
#77088 = CARTESIAN_POINT ( 'NONE',  ( 33.49859180651249346, -292.1449242058744176, -297.8497892959048841 ) ) ;
#77089 = EDGE_CURVE ( 'NONE', #72836, #77341, #57538, .T. ) ;
#77090 = CARTESIAN_POINT ( 'NONE',  ( -87.11466264322206143, -291.1867083139763963, -324.6338007384335924 ) ) ;
#77091 = CARTESIAN_POINT ( 'NONE',  ( 183.0442525570908288, 275.0000000000000568, -7.500000000000000000 ) ) ;
#77092 = CARTESIAN_POINT ( 'NONE',  ( -106.7276692892395573, -291.6624126686373302, -247.1622169206927140 ) ) ;
#77093 = CARTESIAN_POINT ( 'NONE',  ( 140.6539576904058606, 249.5000000000000568, 10.50000000000000000 ) ) ;
#77094 = CARTESIAN_POINT ( 'NONE',  ( -96.07667315357234372, -291.0917637214879505, -319.5567740437876978 ) ) ;
#77096 = CARTESIAN_POINT ( 'NONE',  ( 30.82839066351708013, -293.2034134699283641, -244.2490762878700536 ) ) ;
#77095 = CARTESIAN_POINT ( 'NONE',  ( -98.46934676353225768, -281.9742560001290599, -314.5144165387331441 ) ) ;
#77097 = CARTESIAN_POINT ( 'NONE',  ( -11.50935519425200226, -280.3793842889527923, -197.7676286605547773 ) ) ;
#77098 = CARTESIAN_POINT ( 'NONE',  ( -112.1995860153573972, -283.9936799669806078, -288.3624367532527799 ) ) ;
#77099 = CARTESIAN_POINT ( 'NONE',  ( -18.02420892919868223, -286.8025241078127010, -342.7120662234895576 ) ) ;
#77100 = CARTESIAN_POINT ( 'NONE',  ( -40.30702125146652293, -281.2294074770276211, -344.5370733382084154 ) ) ;
#77101 = CARTESIAN_POINT ( 'NONE',  ( -73.42058401816386493, -278.0623772438861465, -203.1077589245088006 ) ) ;
#77102 = CARTESIAN_POINT ( 'NONE',  ( -43.62716680474309783, -284.8949647816355082, -193.8751910643043743 ) ) ;
#77103 = CARTESIAN_POINT ( 'NONE',  ( 195.2369406736065116, 39.74098473494063910, 14.99224007599141473 ) ) ;
#77104 = CARTESIAN_POINT ( 'NONE',  ( 35.63212331641676656, -295.3003208156014239, -281.7059976894473721 ) ) ;
#77105 = CARTESIAN_POINT ( 'NONE',  ( 28.59670578578791122, -277.4838392500580539, -308.9711285660002318 ) ) ;
#77106 = CARTESIAN_POINT ( 'NONE',  ( -51.28907848291654403, -276.9021381626692460, -342.0378793750112436 ) ) ;
#77107 = CARTESIAN_POINT ( 'NONE',  ( -53.39139012624264780, -292.0185859414371521, -194.9978724050712913 ) ) ;
#77108 = CARTESIAN_POINT ( 'NONE',  ( -73.60676394207003170, -281.6090055231380234, -336.7079612746338739 ) ) ;
#77110 = CARTESIAN_POINT ( 'NONE',  ( 22.00238956904736654, -292.0122295526111884, -227.4249021459777680 ) ) ;
#77109 = CIRCLE ( 'NONE', #1476, 3.842139515347647638 ) ;
#77111 = CARTESIAN_POINT ( 'NONE',  ( -101.4204003466219461, -294.0295443658419572, -309.3344527832240374 ) ) ;
#77112 = EDGE_LOOP ( 'NONE', ( #10503, #77062 ) ) ;
#77113 = CARTESIAN_POINT ( 'NONE',  ( 150.4957602436334412, 21.00000000000000000, 3.637614988394419768 ) ) ;
#77114 = CARTESIAN_POINT ( 'NONE',  ( 17.12226068605793827, -293.7560628651285697, -319.0797258749728940 ) ) ;
#77115 = DIRECTION ( 'NONE',  ( 0.000000000000000000, 0.000000000000000000, -1.000000000000000000 ) ) ;
#77116 = AXIS2_PLACEMENT_3D ( 'NONE', #62504, #83782, #75291 ) ;
#77117 = CARTESIAN_POINT ( 'NONE',  ( -53.28691492658257545, -283.3380690714490697, -200.3538533559491555 ) ) ;
#77118 = CARTESIAN_POINT ( 'NONE',  ( -107.5529561909772696, -296.0095768446936404, -239.1942802845665028 ) ) ;
#77119 = CARTESIAN_POINT ( 'NONE',  ( 36.47945019456036420, -279.4743620972552662, -253.2528424591031353 ) ) ;
#77120 = CARTESIAN_POINT ( 'NONE',  ( 22.59502564391964796, -288.2266882164058757, -222.7914558966029972 ) ) ;
#77121 = CARTESIAN_POINT ( 'NONE',  ( 15.97591771424503371, -286.6679669768500389, -220.4805445411825815 ) ) ;
#77122 = CARTESIAN_POINT ( 'NONE',  ( -40.51644187217473103, -278.6128860674530188, -343.9986203765841992 ) ) ;
#77123 = CARTESIAN_POINT ( 'NONE',  ( -103.9898223251929892, -295.0198014417298396, -236.6324984908770830 ) ) ;
#77124 = CARTESIAN_POINT ( 'NONE',  ( -67.69050609239340588, -297.2160679832949199, -337.8800044027375407 ) ) ;
#77125 = CARTESIAN_POINT ( 'NONE',  ( -109.4361949955159616, -277.1655813682788789, -284.1940162291792831 ) ) ;
#77126 = ORIENTED_EDGE ( 'NONE', *, *, #15644, .F. ) ;
#77127 = CARTESIAN_POINT ( 'NONE',  ( -57.23711263161519724, -331.8906705383788562, 47.50000000000000000 ) ) ;
#77128 = CARTESIAN_POINT ( 'NONE',  ( -99.07294091365119471, -296.8309679794263047, -224.3500100255391771 ) ) ;
#77129 = CARTESIAN_POINT ( 'NONE',  ( -109.1076462815651951, -292.2138832813661793, -290.3236280021598645 ) ) ;
#77130 = CARTESIAN_POINT ( 'NONE',  ( 38.70526900344345478, -295.2230344794398320, -275.9598567637233373 ) ) ;
#77131 = DIRECTION ( 'NONE',  ( 0.000000000000000000, -0.2502735790305594676, 0.9681751575201846816 ) ) ;
#77132 = CARTESIAN_POINT ( 'NONE',  ( 23.59905060707956181, -288.7632899182822257, -310.7587002622397563 ) ) ;
#77133 = CARTESIAN_POINT ( 'NONE',  ( -48.18343439339133027, -254.0284636145295849, -457.8806065563774723 ) ) ;
#77134 = ORIENTED_EDGE ( 'NONE', *, *, #34031, .F. ) ;
#77135 = CARTESIAN_POINT ( 'NONE',  ( 36.37712711407280608, -280.3410715437157705, -248.9047471710078128 ) ) ;
#77136 = CARTESIAN_POINT ( 'NONE',  ( -108.7969599933700664, -297.5661075139699960, -241.8021672348784818 ) ) ;
#77137 = CARTESIAN_POINT ( 'NONE',  ( -95.61342889771168529, -289.3537127779962361, -221.9188601416647941 ) ) ;
#77138 = CARTESIAN_POINT ( 'NONE',  ( 19.36510139688301990, -299.0772331312804795, -193.3791356014287715 ) ) ;
#77139 = CARTESIAN_POINT ( 'NONE',  ( 208.4306832106270804, -148.7221692137691491, 0.000000000000000000 ) ) ;
#77140 = LINE ( 'NONE', #12271, #37128 ) ;
#77141 = CARTESIAN_POINT ( 'NONE',  ( 195.5916183739827545, 25.43510842100078051, 14.50572835022993701 ) ) ;
#77142 = CARTESIAN_POINT ( 'NONE',  ( 7.542467614791021013, -289.9726308056318089, -332.1362490203076732 ) ) ;
#77143 = CARTESIAN_POINT ( 'NONE',  ( -72.02372285203398405, -295.1237833571632336, -198.2697987213421698 ) ) ;
#77144 = ORIENTED_EDGE ( 'NONE', *, *, #11080, .F. ) ;
#77145 = CARTESIAN_POINT ( 'NONE',  ( -7.568785372384704502, -279.7809116860776157, -199.4462947077354897 ) ) ;
#77146 = CARTESIAN_POINT ( 'NONE',  ( -44.21756429591481208, -287.9651449195740724, -195.8443351868794764 ) ) ;
#77147 = CARTESIAN_POINT ( 'NONE',  ( -36.55314179334069280, -284.6366010916459572, -193.9414740894099225 ) ) ;
#77148 = CARTESIAN_POINT ( 'NONE',  ( 30.76490094069783154, -273.1427144188515399, -239.2272965527591566 ) ) ;
#77149 = CARTESIAN_POINT ( 'NONE',  ( -90.28314482040298117, -275.2160841483324134, -218.0302701873049500 ) ) ;
#77150 = CARTESIAN_POINT ( 'NONE',  ( -95.23941597198201237, -287.9830567207312697, -317.1496710895513615 ) ) ;
#77151 = CARTESIAN_POINT ( 'NONE',  ( -106.4397080345745792, -280.0077188122627945, -301.5655412829672173 ) ) ;
#77153 = CARTESIAN_POINT ( 'NONE',  ( -24.85082918697033705, -279.5643063469011054, -198.3342423664415435 ) ) ;
#77152 = CARTESIAN_POINT ( 'NONE',  ( -51.82736042554250844, -279.8617439022426083, -198.7610426472906227 ) ) ;
#77154 = CARTESIAN_POINT ( 'NONE',  ( 39.39822674470777741, -276.6417865678998282, -271.1546663137556266 ) ) ;
#77155 = CARTESIAN_POINT ( 'NONE',  ( 38.47606365382345217, -280.4846042018306775, -281.3007438277670076 ) ) ;
#77156 = CARTESIAN_POINT ( 'NONE',  ( 101.4667014786534196, 115.9046547678812402, -280.3899664935571536 ) ) ;
#77157 = CARTESIAN_POINT ( 'NONE',  ( 37.98554189617519228, -276.3079132803979974, -255.5750832655114380 ) ) ;
#77158 = ADVANCED_FACE ( 'NONE', ( #29610 ), #8730, .T. ) ;
#77159 = CARTESIAN_POINT ( 'NONE',  ( -111.1526627510328495, -274.3190909615437363, -250.8028351022462630 ) ) ;
#77160 = CARTESIAN_POINT ( 'NONE',  ( -20.19161114001083490, -285.3376638359844719, -345.3538533559490702 ) ) ;
#77161 = ORIENTED_EDGE ( 'NONE', *, *, #42403, .F. ) ;
#77162 = FACE_OUTER_BOUND ( 'NONE', #54651, .T. ) ;
#77163 = CARTESIAN_POINT ( 'NONE',  ( 23.01216766782999201, -289.2091694022353181, -311.9961898519719625 ) ) ;
#77164 = CARTESIAN_POINT ( 'NONE',  ( 38.62647161556693476, -289.2910459671626882, -268.6845461064718279 ) ) ;
#77165 = CARTESIAN_POINT ( 'NONE',  ( -66.37713829960758005, -288.7911076824233305, -337.5034831519449199 ) ) ;
#77166 = CARTESIAN_POINT ( 'NONE',  ( -3.510755920250064666, -285.9944197183993992, -201.2452687273539027 ) ) ;
#77167 = CARTESIAN_POINT ( 'NONE',  ( -69.93022918456772175, -196.8786560775615158, -360.4189127159840496 ) ) ;
#77168 = CARTESIAN_POINT ( 'NONE',  ( -49.25115757787841630, -278.2977017474166246, -197.5283970617807370 ) ) ;
#77169 = CARTESIAN_POINT ( 'NONE',  ( -7.784554799578522477, -288.3040946151819526, -202.2638299135906550 ) ) ;
#77170 = CARTESIAN_POINT ( 'NONE',  ( 14.39781181031079704, -280.7886961341544065, -322.9089477586801991 ) ) ;
#77171 = CARTESIAN_POINT ( 'NONE',  ( -79.35037821838379557, -280.7867802708560703, -210.0575986654147869 ) ) ;
#77172 = CARTESIAN_POINT ( 'NONE',  ( -69.27265456268649757, -277.9762532532120076, -336.0895201065175684 ) ) ;
#77173 = CARTESIAN_POINT ( 'NONE',  ( -105.6430817444238386, -289.7972595703521961, -235.5609246756592938 ) ) ;
#77174 = CARTESIAN_POINT ( 'NONE',  ( -113.7422162882503187, -285.2523065848033639, -278.5537946324250242 ) ) ;
#77175 = CARTESIAN_POINT ( 'NONE',  ( -65.22403631520238321, -283.8992606451167262, -342.0837629013142305 ) ) ;
#77176 = CARTESIAN_POINT ( 'NONE',  ( 34.33383619676914833, -281.5353573717350741, -256.4526769708820666 ) ) ;
#77177 = EDGE_LOOP ( 'NONE', ( #85772, #53618, #86937, #14189 ) ) ;
#77178 = LINE ( 'NONE', #53993, #47339 ) ;
#77179 = CARTESIAN_POINT ( 'NONE',  ( -101.2464683506749026, -291.8692335019797497, -311.1575699743892756 ) ) ;
#77180 = CARTESIAN_POINT ( 'NONE',  ( -96.18874809594754538, -289.8988664898998309, -221.4499465881910396 ) ) ;
#77181 = CARTESIAN_POINT ( 'NONE',  ( 33.08961400738228065, -274.3442248985718379, -250.1089695721849750 ) ) ;
#77182 = CARTESIAN_POINT ( 'NONE',  ( -104.5179047653451363, -295.4136782726236561, -307.8955234835698320 ) ) ;
#77183 = VECTOR ( 'NONE', #93642, 1000.000000000000000 ) ;
#77184 = CARTESIAN_POINT ( 'NONE',  ( -97.31443254186125102, -289.6257781146932757, -227.4498505701685360 ) ) ;
#77185 = CARTESIAN_POINT ( 'NONE',  ( -78.53204535554695553, -293.8545225344570326, -331.9155491757897494 ) ) ;
#77186 = CARTESIAN_POINT ( 'NONE',  ( -110.0958104779046209, -291.8893723169344412, -260.2897552016919462 ) ) ;
#77187 = CYLINDRICAL_SURFACE ( 'NONE', #26374, 4.000000000000003553 ) ;
#77188 = CARTESIAN_POINT ( 'NONE',  ( -83.90258770686145340, -291.6913500186184365, -329.2243383782388264 ) ) ;
#77189 = CARTESIAN_POINT ( 'NONE',  ( -37.75867566610864401, -290.0467844235909070, -195.1956035315612326 ) ) ;
#77190 = CARTESIAN_POINT ( 'NONE',  ( 37.58004250640482269, -295.4957536657421429, -265.9558591376419372 ) ) ;
#77191 = CARTESIAN_POINT ( 'NONE',  ( 22.17581839113421083, -287.8978231578880127, -227.6016006015461244 ) ) ;
#77192 = CARTESIAN_POINT ( 'NONE',  ( 30.58447879850155360, -295.9762457331753467, -302.6704645818480230 ) ) ;
#77193 = CARTESIAN_POINT ( 'NONE',  ( 21.45872483227258698, -276.8867311109390243, -223.2140608393319496 ) ) ;
#77194 = CARTESIAN_POINT ( 'NONE',  ( -20.54349816217299818, -297.4546192300558687, -193.5248136303333695 ) ) ;
#77195 = CARTESIAN_POINT ( 'NONE',  ( -4.638235026735377353, -274.8552159000870461, -336.7714146947103586 ) ) ;
#77196 = CARTESIAN_POINT ( 'NONE',  ( -35.60516676954190274, -278.1539211770402176, -195.9287245098378207 ) ) ;
#77197 = CARTESIAN_POINT ( 'NONE',  ( -109.5230369993198991, -273.9353492515585913, -256.7853752516125496 ) ) ;
#77198 = CARTESIAN_POINT ( 'NONE',  ( -108.7510992504447245, -298.2107675610492947, -252.5310447746156228 ) ) ;
#77199 = LINE ( 'NONE', #19434, #42989 ) ;
#77200 = CARTESIAN_POINT ( 'NONE',  ( -93.74459404252580441, -298.0142710445006173, -223.7442516318711796 ) ) ;
#77201 = LINE ( 'NONE', #63027, #48938 ) ;
#77203 = CARTESIAN_POINT ( 'NONE',  ( -87.33175687242416529, -273.1651468073987985, -217.0942201121042103 ) ) ;
#77202 = CARTESIAN_POINT ( 'NONE',  ( 19.31913756162407125, -286.2592727476167056, -320.0590784737461263 ) ) ;
#77204 = CARTESIAN_POINT ( 'NONE',  ( -35.14823699187664374, -286.0789470517875088, -193.3792229723000560 ) ) ;
#77205 = CARTESIAN_POINT ( 'NONE',  ( -48.87002248114648495, -288.8617396216693010, -346.5257704025116254 ) ) ;
#77206 = CARTESIAN_POINT ( 'NONE',  ( -103.1538531219983668, -298.0445600774226591, -307.1715045660848205 ) ) ;
#77207 = CARTESIAN_POINT ( 'NONE',  ( -23.19665252841348391, -292.8708136314868398, -343.8983406446320714 ) ) ;
#77208 = EDGE_CURVE ( 'NONE', #16269, #52326, #42342, .T. ) ;
#77209 = CARTESIAN_POINT ( 'NONE',  ( 32.24180987646308694, -281.1689552750741541, -303.0792889612517342 ) ) ;
#77210 = ADVANCED_FACE ( 'NONE', ( #64227 ), #49962, .T. ) ;
#77211 = CARTESIAN_POINT ( 'NONE',  ( 31.98288692825982693, -290.6237833571633473, -237.0123917617630980 ) ) ;
#77212 = CARTESIAN_POINT ( 'NONE',  ( -0.4778554359995536571, -278.5419125565632612, -205.0315369040635574 ) ) ;
#77213 = FACE_OUTER_BOUND ( 'NONE', #47443, .T. ) ;
#77214 = CARTESIAN_POINT ( 'NONE',  ( -63.97923812062445137, -288.2022525483117761, -338.8083807621004553 ) ) ;
#77215 = CARTESIAN_POINT ( 'NONE',  ( 183.0442525570908288, 293.9636489450775230, 0.000000000000000000 ) ) ;
#77216 = CARTESIAN_POINT ( 'NONE',  ( -106.9792876876985162, -288.1875797798215899, -298.3503455605481349 ) ) ;
#77217 = CARTESIAN_POINT ( 'NONE',  ( -86.64976378570321458, -298.9531321934215384, -215.4506884472496040 ) ) ;
#77218 = CARTESIAN_POINT ( 'NONE',  ( -10.88885579115580171, -284.1393066052172571, -342.1031320851379292 ) ) ;
#77220 = CARTESIAN_POINT ( 'NONE',  ( 30.02149271457893320, -281.1748314979352017, -242.2328359510785845 ) ) ;
#77219 = CARTESIAN_POINT ( 'NONE',  ( -74.93695352436466806, -295.5746080074775364, -204.9942468947497218 ) ) ;
#77221 = CARTESIAN_POINT ( 'NONE',  ( -102.3175327946302957, -297.2603842766558273, -229.0435530278357419 ) ) ;
#77222 = CARTESIAN_POINT ( 'NONE',  ( -48.98642912152735107, -275.3263192974031881, -197.6474684415731247 ) ) ;
#77223 = CARTESIAN_POINT ( 'NONE',  ( 32.45361939265070816, -283.1933631698066165, -242.7674620859592665 ) ) ;
#77224 = B_SPLINE_CURVE_WITH_KNOTS ( 'NONE', 3,
 ( #73037, #64584, #72128, #7244 ),
 .UNSPECIFIED., .F., .F.,
 ( 4, 4 ),
 ( 1.734723475976807094E-18, 0.0008449500572417431576 ),
 .UNSPECIFIED. ) ;
#77225 = CARTESIAN_POINT ( 'NONE',  ( -108.8333058931776947, -271.6855809578856338, -254.1384061293102548 ) ) ;
#77226 = ORIENTED_EDGE ( 'NONE', *, *, #6030, .F. ) ;
#77227 = LINE ( 'NONE', #10939, #83101 ) ;
#77228 = CARTESIAN_POINT ( 'NONE',  ( -95.41729670089114279, -287.1807752485198648, -223.4465878802722330 ) ) ;
#77229 = DIRECTION ( 'NONE',  ( 0.000000000000000000, 1.000000000000000000, 0.000000000000000000 ) ) ;
#77230 = CARTESIAN_POINT ( 'NONE',  ( -99.90806341382575795, -275.4094976428775681, -320.2154176792147382 ) ) ;
#77231 = CARTESIAN_POINT ( 'NONE',  ( -97.80818132016572974, -277.1141899951845744, -317.7738111518575579 ) ) ;
#77232 = CARTESIAN_POINT ( 'NONE',  ( -105.8038040998388993, -288.5165352701823167, -303.9382687494446031 ) ) ;
#77233 = CARTESIAN_POINT ( 'NONE',  ( -69.29241909287274837, -285.0004725045340592, -336.7818214500148883 ) ) ;
#77234 = CARTESIAN_POINT ( 'NONE',  ( 31.86149825917260969, -276.8140934790913548, -244.7221291755344055 ) ) ;
#77235 = CARTESIAN_POINT ( 'NONE',  ( -113.5655135601975019, -286.0536449265675287, -264.3130900155326231 ) ) ;
#77236 = CARTESIAN_POINT ( 'NONE',  ( -33.49065488986707351, -281.7975541347797730, -343.6697340270898735 ) ) ;
#77237 = CARTESIAN_POINT ( 'NONE',  ( 10.53417674869039544, -282.7130705968492066, -212.5621547007312699 ) ) ;
#77238 = CARTESIAN_POINT ( 'NONE',  ( -13.06449860147223774, -274.5257687079455877, -197.2884316317034745 ) ) ;
#77239 = CARTESIAN_POINT ( 'NONE',  ( -9.213795940154822617, -276.5277052220291694, -342.0397131871494594 ) ) ;
#77240 = CARTESIAN_POINT ( 'NONE',  ( -53.43737329538826941, -297.1802302930198039, -343.0931690192838914 ) ) ;
#77241 = CARTESIAN_POINT ( 'NONE',  ( 194.5881128153457098, 0.000000000000000000, -47.19625681453479871 ) ) ;
#77242 = DIRECTION ( 'NONE',  ( 0.000000000000000000, 0.000000000000000000, 1.000000000000000000 ) ) ;
#77243 = CARTESIAN_POINT ( 'NONE',  ( -81.17667521555783594, -293.7799658324468624, -332.2216527674179360 ) ) ;
#77244 = EDGE_CURVE ( 'NONE', #64642, #55253, #72684, .T. ) ;
#77245 = CARTESIAN_POINT ( 'NONE',  ( 32.15478393937396362, -275.3586503405441022, -292.9050116996871225 ) ) ;
#77246 = CARTESIAN_POINT ( 'NONE',  ( -36.20395713954953010, -299.1457486080698231, -193.6700243703820945 ) ) ;
#77247 = CIRCLE ( 'NONE', #60630, 25.00000000000000355 ) ;
#77248 = CARTESIAN_POINT ( 'NONE',  ( -41.40060480639604634, -287.7605246099691385, -196.4464889012422475 ) ) ;
#77249 = CARTESIAN_POINT ( 'NONE',  ( 36.40745503038448305, -294.8242035897088726, -250.7207104913053968 ) ) ;
#77250 = CARTESIAN_POINT ( 'NONE',  ( 35.90279891270316170, -294.4740753464654972, -247.9278373721565458 ) ) ;
#77251 = CARTESIAN_POINT ( 'NONE',  ( -111.6058545418704142, -292.4337688319313315, -279.5732727291029960 ) ) ;
#77252 = CARTESIAN_POINT ( 'NONE',  ( -5.978376501635822571, -278.4651481980118888, -202.4032514162272491 ) ) ;
#77253 = CARTESIAN_POINT ( 'NONE',  ( -110.1685977613244916, -280.2729174686764964, -285.7740081200694249 ) ) ;
#77254 = CARTESIAN_POINT ( 'NONE',  ( -56.19109979435656044, -293.3765524300336551, -342.4285268525277388 ) ) ;
#77255 = CARTESIAN_POINT ( 'NONE',  ( -91.53343208344301729, -285.6743392763380598, -323.3097881022966362 ) ) ;
#77256 = CARTESIAN_POINT ( 'NONE',  ( -110.5359407540881591, -283.5372398152482560, -265.4307739675700759 ) ) ;
#77257 = CARTESIAN_POINT ( 'NONE',  ( -97.57403984170483113, -248.8065872697612235, -333.5881438307000053 ) ) ;
#77258 = EDGE_LOOP ( 'NONE', ( #84363, #43260, #72740, #55012 ) ) ;
#77259 = CARTESIAN_POINT ( 'NONE',  ( -109.2130836966811387, -284.3900130454696296, -257.3837567132265463 ) ) ;
#77260 = VERTEX_POINT ( 'NONE', #44718 ) ;
#77261 = CARTESIAN_POINT ( 'NONE',  ( 36.29903743685528639, -282.3616686027557421, -248.9006549765587124 ) ) ;
#77262 = CARTESIAN_POINT ( 'NONE',  ( -68.29540153355293342, -273.9673374811358713, -204.2115265979955723 ) ) ;
#77263 = CARTESIAN_POINT ( 'NONE',  ( 36.99523792961881696, -286.1145090207178896, -251.8671092167354288 ) ) ;
#77264 = CARTESIAN_POINT ( 'NONE',  ( 38.02139949185922774, -282.3102198554902884, -255.7589459090048933 ) ) ;
#77265 =( NAMED_UNIT ( * ) PLANE_ANGLE_UNIT ( ) SI_UNIT ( $, .RADIAN. ) );
#77266 = CARTESIAN_POINT ( 'NONE',  ( -99.88602327595673103, -279.4891286030614310, -314.0751362733595329 ) ) ;
#77267 = CARTESIAN_POINT ( 'NONE',  ( -59.28100680299512248, -280.4268010511798934, -196.6591532262175974 ) ) ;
#77268 = CARTESIAN_POINT ( 'NONE',  ( -92.05005921254146983, -276.6952119285918457, -226.6919474004047572 ) ) ;
#77269 = CARTESIAN_POINT ( 'NONE',  ( -112.8251851669977412, -274.5109097693414242, -270.3860576588319304 ) ) ;
#77270 = VERTEX_POINT ( 'NONE', #36228 ) ;
#77271 = CARTESIAN_POINT ( 'NONE',  ( -72.79831222453096018, -275.5819331585354348, -204.4030136627089860 ) ) ;
#77272 = CARTESIAN_POINT ( 'NONE',  ( 173.4835934154848474, 243.5194095459789594, -179.5650955095518668 ) ) ;
#77273 = CARTESIAN_POINT ( 'NONE',  ( -39.72913769637881387, -278.0421591143949627, -195.7417012399943985 ) ) ;
#77274 = CARTESIAN_POINT ( 'NONE',  ( 38.49251824203401640, -295.3830215542195674, -275.9420958396887045 ) ) ;
#77275 = CARTESIAN_POINT ( 'NONE',  ( -50.49768193835280528, -294.5731957043777243, -342.2694819639166326 ) ) ;
#77276 = CARTESIAN_POINT ( 'NONE',  ( -11.16828578309394437, -291.8918138754450524, -197.9554217367301590 ) ) ;
#77277 = CARTESIAN_POINT ( 'NONE',  ( 197.2116943569230045, 249.5000000000000568, -12.92446933126075592 ) ) ;
#77279 = CARTESIAN_POINT ( 'NONE',  ( 36.24793321391939571, -286.0330173055198202, -276.5686898780962792 ) ) ;
#77278 = CARTESIAN_POINT ( 'NONE',  ( -96.07028261437285721, -294.4641418486955331, -319.2645939763480101 ) ) ;
#77280 = CARTESIAN_POINT ( 'NONE',  ( 35.69422701420712940, -295.2392574985910869, -257.0007532810924999 ) ) ;
#77281 = CARTESIAN_POINT ( 'NONE',  ( -105.6662596395761682, -285.5059467207601642, -297.5735045685493105 ) ) ;
#77282 = VERTEX_POINT ( 'NONE', #57556 ) ;
#77283 = CARTESIAN_POINT ( 'NONE',  ( -111.7694017034676790, -291.7299180762429387, -251.5108651682547816 ) ) ;
#77284 = CARTESIAN_POINT ( 'NONE',  ( 25.61523959131629624, -282.5544737994703723, -307.5341694113048447 ) ) ;
#77285 = CARTESIAN_POINT ( 'NONE',  ( -68.08099987688039789, -294.2418324800765959, -340.5259536945005721 ) ) ;
#77286 = CARTESIAN_POINT ( 'NONE',  ( -91.47749177689408384, -290.6016074051137821, -324.9655337851310719 ) ) ;
#77287 = CARTESIAN_POINT ( 'NONE',  ( -93.54355141942230034, -290.3266848980300097, -322.9819581056194693 ) ) ;
#77288 = CARTESIAN_POINT ( 'NONE',  ( 6.925239249690358534, -286.8402914982984271, -212.2503905482281255 ) ) ;
#77289 = VERTEX_POINT ( 'NONE', #21092 ) ;
#77290 = FACE_OUTER_BOUND ( 'NONE', #80985, .T. ) ;
#77291 = CARTESIAN_POINT ( 'NONE',  ( -113.0761406689542099, -298.4576147758664888, -266.8170708179517874 ) ) ;
#77292 = CARTESIAN_POINT ( 'NONE',  ( -112.8998493393293785, -295.3892078481714520, -258.2672281377859917 ) ) ;
#77293 = CARTESIAN_POINT ( 'NONE',  ( 5.069135742710565218, -279.7002664200090294, -210.6557627097400882 ) ) ;
#77294 = VERTEX_POINT ( 'NONE', #22481 ) ;
#77295 = CARTESIAN_POINT ( 'NONE',  ( 31.79722804924804080, -275.4949158563856599, -304.2364910928609447 ) ) ;
#77296 = CARTESIAN_POINT ( 'NONE',  ( -111.0781455506785989, -295.0177375948194367, -271.4542650046025187 ) ) ;
#77297 = CARTESIAN_POINT ( 'NONE',  ( -94.54290868380795132, -279.7527027546158251, -317.6979073773452455 ) ) ;
#77298 = CARTESIAN_POINT ( 'NONE',  ( 36.82233284998997647, -273.6363385670197772, -266.0911458571676462 ) ) ;
#77299 = CARTESIAN_POINT ( 'NONE',  ( -50.52756109534759332, -296.4293858258642445, -342.5640512630100716 ) ) ;
#77300 = CARTESIAN_POINT ( 'NONE',  ( -110.0446187179810238, -297.7604578176957943, -260.5690238123582958 ) ) ;
#77301 = FACE_OUTER_BOUND ( 'NONE', #89372, .T. ) ;
#77302 = CARTESIAN_POINT ( 'NONE',  ( -97.62889640276073067, -297.5236389424904360, -316.9647056497042286 ) ) ;
#77303 = CARTESIAN_POINT ( 'NONE',  ( -99.83017026760452950, -271.1403111205165715, -228.1541608417376779 ) ) ;
#77304 = CARTESIAN_POINT ( 'NONE',  ( -22.72834790946917494, -292.8955738398317976, -198.7347080154864614 ) ) ;
#77305 = CARTESIAN_POINT ( 'NONE',  ( -103.3821449118243265, -288.6904899815788781, -302.8270165252582728 ) ) ;
#77306 = DIRECTION ( 'NONE',  ( -1.000000000000000000, 0.000000000000000000, 0.000000000000000000 ) ) ;
#77307 = CARTESIAN_POINT ( 'NONE',  ( 21.79952980183030675, -275.3820483022533381, -221.1489058207764060 ) ) ;
#77308 = CARTESIAN_POINT ( 'NONE',  ( -102.5531277108105570, -297.3326026026563227, -237.3919050365249461 ) ) ;
#77309 = CARTESIAN_POINT ( 'NONE',  ( -42.34653686997286570, -281.9692149499761626, -195.1722995795721260 ) ) ;
#77310 = CARTESIAN_POINT ( 'NONE',  ( 5.919282313119296646, -279.3103535233535695, -207.2597260016497387 ) ) ;
#77311 = CARTESIAN_POINT ( 'NONE',  ( -14.62772986771192407, -276.1140199954659806, -343.8837877214476748 ) ) ;
#77312 = CARTESIAN_POINT ( 'NONE',  ( -14.44848591618436195, -278.7438323821601784, -197.6260773797845900 ) ) ;
#77313 = CARTESIAN_POINT ( 'NONE',  ( 29.45772765340825217, -281.1517444727174393, -300.3256788491529505 ) ) ;
#77314 = CARTESIAN_POINT ( 'NONE',  ( 33.60592920785114046, -279.2294068260043787, -245.3768462868488029 ) ) ;
#77315 = CARTESIAN_POINT ( 'NONE',  ( 19.46519033736816340, -273.4692530494965581, -223.5812920476788577 ) ) ;
#77316 = CARTESIAN_POINT ( 'NONE',  ( -109.5424002012343152, -280.2906051159577601, -290.7069027285324410 ) ) ;
#77317 = CYLINDRICAL_SURFACE ( 'NONE', #32285, 2.000000000000000888 ) ;
#77318 = DIRECTION ( 'NONE',  ( 0.000000000000000000, 0.000000000000000000, -1.000000000000000000 ) ) ;
#77319 = CARTESIAN_POINT ( 'NONE',  ( -15.15586600844804366, -296.5661453759868778, -194.3809848250822085 ) ) ;
#77320 = CIRCLE ( 'NONE', #71318, 24.50000000000000355 ) ;
#77321 = CARTESIAN_POINT ( 'NONE',  ( -8.511219139766771136, -292.4192644703935002, -198.9622148678591600 ) ) ;
#77322 = CARTESIAN_POINT ( 'NONE',  ( -35.72478514203644551, -279.0321009713018157, -345.5232069913787996 ) ) ;
#77323 = CARTESIAN_POINT ( 'NONE',  ( 28.40162965020363828, -273.0708667732494632, -234.1582794054303065 ) ) ;
#77324 = EDGE_CURVE ( 'NONE', #41101, #42782, #32114, .T. ) ;
#77325 = DIRECTION ( 'NONE',  ( 0.000000000000000000, 0.000000000000000000, 1.000000000000000000 ) ) ;
#77326 = CARTESIAN_POINT ( 'NONE',  ( -110.3366228393558544, -286.7236409346665482, -250.6435797490756272 ) ) ;
#77327 = CARTESIAN_POINT ( 'NONE',  ( 155.9223079842153368, 17.31716537716996740, -7.900495735315888446 ) ) ;
#77328 = CARTESIAN_POINT ( 'NONE',  ( 29.10142715569293159, -285.0898351751019959, -235.4609823526696175 ) ) ;
#77329 = DIRECTION ( 'NONE',  ( -0.5000000000000046629, 0.8660254037844359321, 0.000000000000000000 ) ) ;
#77330 = CARTESIAN_POINT ( 'NONE',  ( 34.71126590625547692, -292.5305231445061622, -284.3432705863880301 ) ) ;
#77331 = CARTESIAN_POINT ( 'NONE',  ( 18.72437503044040596, -285.0096811931502998, -221.7045593444512690 ) ) ;
#77332 = CARTESIAN_POINT ( 'NONE',  ( 27.50960667658514680, -292.0550941587824809, -308.0348309973611549 ) ) ;
#77333 = CARTESIAN_POINT ( 'NONE',  ( -91.39805402843452953, -283.7795906197707723, -216.5037289358239150 ) ) ;
#77334 = CARTESIAN_POINT ( 'NONE',  ( -110.9580787753649957, -280.2201773017984010, -265.1583102334440127 ) ) ;
#77335 = CARTESIAN_POINT ( 'NONE',  ( 36.00963802370197442, -289.0363214940731496, -292.4881452991650121 ) ) ;
#77336 = CARTESIAN_POINT ( 'NONE',  ( 37.86509368631639916, -279.9296282722160640, -281.2198553779076633 ) ) ;
#77337 = CARTESIAN_POINT ( 'NONE',  ( 24.23834806081161375, -288.0942030010875214, -309.5644043888502210 ) ) ;
#77338 = CARTESIAN_POINT ( 'NONE',  ( -95.26581759588367504, -280.6124383379262213, -224.9517165648865102 ) ) ;
#77339 = CARTESIAN_POINT ( 'NONE',  ( -6.711125407345084781, -281.2676868631708089, -203.9067202432402155 ) ) ;
#77340 = CARTESIAN_POINT ( 'NONE',  ( -66.57476175461849266, -287.6510473258031197, -200.9072850254773925 ) ) ;
#77341 = VERTEX_POINT ( 'NONE', #51816 ) ;
#77342 = CARTESIAN_POINT ( 'NONE',  ( -18.54997314560486288, -274.2876024936937256, -195.6343329760304073 ) ) ;
#77343 = CARTESIAN_POINT ( 'NONE',  ( -100.2138800420910059, -291.9877266598252277, -310.5971192104252623 ) ) ;
#77344 = CARTESIAN_POINT ( 'NONE',  ( 158.3135449435333442, 1.828427124746191623, -9.000000000000001776 ) ) ;
#77345 = CARTESIAN_POINT ( 'NONE',  ( -37.37352853689063181, -294.5519495502701375, -190.3611179825600175 ) ) ;
#77346 = EDGE_LOOP ( 'NONE', ( #45354, #79649, #24856, #6952 ) ) ;
#77347 = CARTESIAN_POINT ( 'NONE',  ( -75.48002086293303137, -271.5449969381613187, -205.5283310817638665 ) ) ;
#77348 = CYLINDRICAL_SURFACE ( 'NONE', #6572, 1.000000000000002887 ) ;
#77349 = CARTESIAN_POINT ( 'NONE',  ( -107.6449163768319437, -294.5727261290124943, -299.8899149845005923 ) ) ;
#77350 = CARTESIAN_POINT ( 'NONE',  ( -70.48986961165952891, -297.1105319472983410, -205.2381535029308282 ) ) ;
#77351 = CARTESIAN_POINT ( 'NONE',  ( -69.03882190068929958, -290.9969293095570606, -336.8893091954611236 ) ) ;
#77352 = CARTESIAN_POINT ( 'NONE',  ( 27.75682983075313004, -283.7861920194488334, -305.5769582877894095 ) ) ;
#77353 = CARTESIAN_POINT ( 'NONE',  ( -31.85085868743179560, -290.4095479473361934, -346.6265049199604960 ) ) ;
#77354 = CARTESIAN_POINT ( 'NONE',  ( -41.71551683489051499, -290.4213084805252834, -346.7559810974654511 ) ) ;
#77355 = CARTESIAN_POINT ( 'NONE',  ( -11.35217416547049751, -288.3909272591037620, -200.0081138632613715 ) ) ;
#77356 = CARTESIAN_POINT ( 'NONE',  ( -48.12088097647951201, -280.0854429653931561, -194.0654917074606089 ) ) ;
#77357 = CARTESIAN_POINT ( 'NONE',  ( -81.05885674789219308, -293.7202373202401304, -332.0539615452185558 ) ) ;
#77358 = CARTESIAN_POINT ( 'NONE',  ( -69.18839340495958368, -283.2929206411404266, -340.4810822252150615 ) ) ;
#77359 = CARTESIAN_POINT ( 'NONE',  ( 25.03493015157739521, -277.9615880738130045, -310.7054365858038523 ) ) ;
#77360 = CARTESIAN_POINT ( 'NONE',  ( -54.49178911615187815, -300.3376638359845856, -195.3683826091709363 ) ) ;
#77361 = CARTESIAN_POINT ( 'NONE',  ( 21.83750849964845742, -274.4395752303639142, -318.0450448354746982 ) ) ;
#77362 = CARTESIAN_POINT ( 'NONE',  ( 133.0872704186301405, -299.5541904835127980, -189.7068768330456123 ) ) ;
#77363 = CARTESIAN_POINT ( 'NONE',  ( 35.20010206636703742, -281.1798904496186537, -279.4721262232380354 ) ) ;
#77364 = CARTESIAN_POINT ( 'NONE',  ( -112.9049515239061634, -279.5991043119831261, -282.9390254968345175 ) ) ;
#77365 = CARTESIAN_POINT ( 'NONE',  ( -85.35638131283359087, -284.4655923995548505, -210.4661215053584726 ) ) ;
#77366 = CARTESIAN_POINT ( 'NONE',  ( 22.61257280515301460, -294.7131862893086236, -226.9407363848139312 ) ) ;
#77367 = CARTESIAN_POINT ( 'NONE',  ( -13.33405157559051446, -275.9589860885334929, -198.0418727902042804 ) ) ;
#77368 = CARTESIAN_POINT ( 'NONE',  ( -96.56505392314146263, -274.5219562103158637, -221.9062537604232830 ) ) ;
#77369 = DIRECTION ( 'NONE',  ( 0.000000000000000000, 1.000000000000000000, 0.000000000000000000 ) ) ;
#77370 = CARTESIAN_POINT ( 'NONE',  ( 3.132342629701405201, -276.3248588337945648, -331.1134995600137358 ) ) ;
#77371 = CARTESIAN_POINT ( 'NONE',  ( -97.87682630648174609, -297.9514028538691832, -314.3776039246594678 ) ) ;
#77372 = CARTESIAN_POINT ( 'NONE',  ( -110.1432894426382489, -282.7755235744673996, -252.9867443627554167 ) ) ;
#77373 = CARTESIAN_POINT ( 'NONE',  ( 38.04206837735083724, -293.0230429012081572, -254.7070203038033185 ) ) ;
#77374 = CARTESIAN_POINT ( 'NONE',  ( 23.79889418041276983, -274.1573543743063510, -313.2712431450771078 ) ) ;
#77375 = CARTESIAN_POINT ( 'NONE',  ( -26.24076471373900077, -290.5132203334983387, -345.7481834968157273 ) ) ;
#77376 = CARTESIAN_POINT ( 'NONE',  ( -109.2446036967447469, -289.2839221563621095, -284.7151912014841173 ) ) ;
#77377 = ORIENTED_EDGE ( 'NONE', *, *, #47505, .T. ) ;
#77378 = CARTESIAN_POINT ( 'NONE',  ( 28.97333788253397557, -291.6299110244307826, -232.4016392550730927 ) ) ;
#77379 = CARTESIAN_POINT ( 'NONE',  ( -104.7209413559483835, -290.5978710534776042, -242.0848330055396787 ) ) ;
#77380 = ORIENTED_EDGE ( 'NONE', *, *, #16494, .T. ) ;
#77381 = CARTESIAN_POINT ( 'NONE',  ( 37.98397888825627433, -288.4509250956489268, -255.9550570612347826 ) ) ;
#77382 = CARTESIAN_POINT ( 'NONE',  ( -92.22713538988517712, -279.5728480591091056, -222.1790755507894062 ) ) ;
#77383 = CARTESIAN_POINT ( 'NONE',  ( -65.50283942674079185, -294.3321621436324449, -341.7086054328553928 ) ) ;
#77384 = CARTESIAN_POINT ( 'NONE',  ( -113.3878946311204885, -285.3509056830875465, -258.5953143770485667 ) ) ;
#77385 = CARTESIAN_POINT ( 'NONE',  ( -83.26666720299689928, -285.7757818577235298, -208.5156694566777560 ) ) ;
#77386 = CARTESIAN_POINT ( 'NONE',  ( 35.45046789263039244, -281.9696746804660847, -276.7487675510756162 ) ) ;
#77387 = CARTESIAN_POINT ( 'NONE',  ( 103.0508316722241346, 116.5178241089715954, -282.9552863566690348 ) ) ;
#77388 = AXIS2_PLACEMENT_3D ( 'NONE', #50030, #78010, #20704 ) ;
#77389 = CARTESIAN_POINT ( 'NONE',  ( -23.47725864820640496, -107.6783844017259923, -361.4025868328823776 ) ) ;
#77390 = CARTESIAN_POINT ( 'NONE',  ( -98.64580574393880852, -246.0797455245688639, -331.3209657627199931 ) ) ;
#77391 = CARTESIAN_POINT ( 'NONE',  ( -6.451524256303274640, -273.6657537687231638, -204.0406930583991993 ) ) ;
#77392 = CARTESIAN_POINT ( 'NONE',  ( 15.81258065505600285, -275.1972062376293593, -320.8472399181486026 ) ) ;
#77393 = CARTESIAN_POINT ( 'NONE',  ( -65.51362775474740374, -297.2013135087214550, -198.7089991478085551 ) ) ;
#77394 = CARTESIAN_POINT ( 'NONE',  ( -46.28360890110539572, -155.9045745473734712, -362.0530608825127956 ) ) ;
#77395 = CARTESIAN_POINT ( 'NONE',  ( 3.225720779939448946, -275.2044512057388488, -335.2893538922770631 ) ) ;
#77396 = CARTESIAN_POINT ( 'NONE',  ( -32.64886520893520583, -275.8722196026442361, -196.4840060102316670 ) ) ;
#77397 = EDGE_LOOP ( 'NONE', ( #35226, #92157, #26211, #81009 ) ) ;
#77398 = CARTESIAN_POINT ( 'NONE',  ( -112.0481483480647711, -297.7149128191339855, -252.7041984195134035 ) ) ;
#77399 = CIRCLE ( 'NONE', #72866, 4.499999999999990230 ) ;
#77400 = CARTESIAN_POINT ( 'NONE',  ( -26.45953640725284473, -289.4024252463407834, -342.6587813542579966 ) ) ;
#77401 = CARTESIAN_POINT ( 'NONE',  ( -92.57381523852140504, -296.6216133328625801, -323.7799562400920763 ) ) ;
#77402 = CARTESIAN_POINT ( 'NONE',  ( -113.8813637145674420, -296.9465763628708714, -278.1845955469045748 ) ) ;
#77403 = CARTESIAN_POINT ( 'NONE',  ( -3.638144592954465129, -292.6767044796009145, -205.6071964888223249 ) ) ;
#77404 = ORIENTED_EDGE ( 'NONE', *, *, #88613, .T. ) ;
#77405 = CARTESIAN_POINT ( 'NONE',  ( 35.85008965298685268, -277.7116598873871567, -289.1301379266436697 ) ) ;
#77406 = ORIENTED_EDGE ( 'NONE', *, *, #72224, .F. ) ;
#77407 = CARTESIAN_POINT ( 'NONE',  ( 37.27310987508800366, -280.8248233538912473, -251.5952705020294502 ) ) ;
#77408 = CARTESIAN_POINT ( 'NONE',  ( -74.12110925451041510, -278.4951698956776909, -333.6910754478980152 ) ) ;
#77409 = CARTESIAN_POINT ( 'NONE',  ( 15.30855924699483595, -276.5438962422526288, -215.5712995857689407 ) ) ;
#77410 = CARTESIAN_POINT ( 'NONE',  ( -104.8825883084782902, -276.1320843338635882, -303.8946880390452066 ) ) ;
#77411 = CARTESIAN_POINT ( 'NONE',  ( -109.8384292365054478, -297.3322686944680981, -260.5913291757692036 ) ) ;
#77412 = CARTESIAN_POINT ( 'NONE',  ( -80.51501540564287041, -294.2252114374209100, -329.9550754243879851 ) ) ;
#77413 = CARTESIAN_POINT ( 'NONE',  ( 152.4883615486606914, 19.90193753873172611, -8.271207965221249125 ) ) ;
#77414 = CARTESIAN_POINT ( 'NONE',  ( 6.144306111678071503, -281.1175836400039429, -206.8906983809304450 ) ) ;
#77415 = CARTESIAN_POINT ( 'NONE',  ( -13.78339066984367811, -276.9045424514074512, -339.5084388980351946 ) ) ;
#77416 = CARTESIAN_POINT ( 'NONE',  ( 39.20877648171386198, -286.2520745157656847, -271.5603816381632214 ) ) ;
#77417 = CARTESIAN_POINT ( 'NONE',  ( -111.5687934622130797, -274.6947677400971202, -259.2664601885816751 ) ) ;
#77418 = CARTESIAN_POINT ( 'NONE',  ( 82.66796173774982037, -298.0572237680152057, -197.3908676648706546 ) ) ;
#77419 = CARTESIAN_POINT ( 'NONE',  ( -8.163471781230724034, -287.8572653847649576, -337.5064996368687389 ) ) ;
#77420 = EDGE_CURVE ( 'NONE', #54877, #13227, #35774, .T. ) ;
#77421 = CARTESIAN_POINT ( 'NONE',  ( -35.61702189677296104, -278.3139081398977055, -196.3553038020013162 ) ) ;
#77423 = CARTESIAN_POINT ( 'NONE',  ( -83.71043491836863382, -281.7735895281192029, -328.6617593302388514 ) ) ;
#77422 = CARTESIAN_POINT ( 'NONE',  ( -34.27071471297013261, -278.6662055073705915, -196.8233486303982431 ) ) ;
#77424 = CARTESIAN_POINT ( 'NONE',  ( 17.95762232805615000, -288.8445455696343060, -219.6769646416762782 ) ) ;
#77425 = CARTESIAN_POINT ( 'NONE',  ( -95.57876355041473460, -279.1321192728485698, -315.0329765732262217 ) ) ;
#77426 = CARTESIAN_POINT ( 'NONE',  ( 209.1374487190023501, 30.94653725228601715, 12.00000000000000000 ) ) ;
#77427 = CARTESIAN_POINT ( 'NONE',  ( -67.54727592993694429, -293.6560919845480271, -201.6985686519389276 ) ) ;
#77428 = CARTESIAN_POINT ( 'NONE',  ( -37.15229770530419984, -275.2896422888138659, -346.3604383442195740 ) ) ;
#77429 = CARTESIAN_POINT ( 'NONE',  ( 5.463179849941725230, -277.1070847272241053, -329.6826813774569587 ) ) ;
#77430 = CARTESIAN_POINT ( 'NONE',  ( 8.120700661274417698, -284.4322384300798490, -330.2209420551196786 ) ) ;
#77431 = DIRECTION ( 'NONE',  ( -1.000000000000000000, -0.000000000000000000, -0.000000000000000000 ) ) ;
#77432 = CARTESIAN_POINT ( 'NONE',  ( -97.86082782334997887, -291.8586552450849467, -315.6235199801517979 ) ) ;
#77433 = CARTESIAN_POINT ( 'NONE',  ( -106.5383782189670541, -294.1727330861852465, -299.4213802197311907 ) ) ;
#77434 = CARTESIAN_POINT ( 'NONE',  ( -91.78136191330990812, -284.4967643776529940, -216.1349061936205658 ) ) ;
#77435 = CARTESIAN_POINT ( 'NONE',  ( 197.2116943569230330, 250.0000000000000568, -11.92446933126075237 ) ) ;
#77436 = CARTESIAN_POINT ( 'NONE',  ( -21.81361185470477437, -272.9401739851583670, -198.5271291531404358 ) ) ;
#77437 = CARTESIAN_POINT ( 'NONE',  ( 34.63802555264857830, -291.9274201760563301, -288.5210897342315093 ) ) ;
#77438 = DIRECTION ( 'NONE',  ( 0.000000000000000000, 0.000000000000000000, 1.000000000000000000 ) ) ;
#77439 = CARTESIAN_POINT ( 'NONE',  ( 219.7099725226080977, -142.7221692137691775, -1.978481845683818907 ) ) ;
#77440 = CARTESIAN_POINT ( 'NONE',  ( -86.05540008278258313, -289.8712145154160567, -211.5585211824224245 ) ) ;
#77441 = CARTESIAN_POINT ( 'NONE',  ( -26.74001617445735590, -284.4249468900777060, -195.0648615902831011 ) ) ;
#77442 = EDGE_CURVE ( 'NONE', #75053, #4038, #82095, .T. ) ;
#77443 = CARTESIAN_POINT ( 'NONE',  ( -102.2827404765905470, -285.5082187710081030, -305.0821826743190286 ) ) ;
#77444 = CARTESIAN_POINT ( 'NONE',  ( -25.12489836091869932, -287.0146202568702734, -198.1754472287298086 ) ) ;
#77445 = CARTESIAN_POINT ( 'NONE',  ( -101.8217727014944671, -293.0532480950006970, -231.2639581509192510 ) ) ;
#77446 = CARTESIAN_POINT ( 'NONE',  ( 24.86715268174845050, -274.2100772408344938, -313.3395480074868260 ) ) ;
#77447 = VECTOR ( 'NONE', #39059, 1000.000000000000114 ) ;
#77448 = CARTESIAN_POINT ( 'NONE',  ( 34.70047193010576336, -275.5421872205032514, -243.2378855682353560 ) ) ;
#77449 = CARTESIAN_POINT ( 'NONE',  ( -36.37181904703815150, -290.1440745006411248, -194.7945497292644177 ) ) ;
#77450 = CARTESIAN_POINT ( 'NONE',  ( -111.4405165336055887, -278.2897470859475106, -291.2982956171031219 ) ) ;
#77451 = CARTESIAN_POINT ( 'NONE',  ( -112.0294948340390278, -298.5171885865095760, -271.5131086094469879 ) ) ;
#77452 = CARTESIAN_POINT ( 'NONE',  ( 208.4306832106271088, 20.44233620800389772, 7.500000000000013323 ) ) ;
#77453 = LINE ( 'NONE', #4543, #58682 ) ;
#77454 = CARTESIAN_POINT ( 'NONE',  ( -100.0212152562736065, -283.7633581369656213, -231.8907389205920140 ) ) ;
#77455 = CARTESIAN_POINT ( 'NONE',  ( -17.49604334400470051, -278.3080528014002084, -198.0344247584943957 ) ) ;
#77456 = DIRECTION ( 'NONE',  ( -0.000000000000000000, 1.000000000000000000, 0.000000000000000000 ) ) ;
#77457 = CARTESIAN_POINT ( 'NONE',  ( -13.26275721310359756, -272.8392384892069913, -197.9531608251776618 ) ) ;
#77458 = B_SPLINE_CURVE_WITH_KNOTS ( 'NONE', 3,
 ( #76094, #83178, #4586, #10277, #68058, #33460 ),
 .UNSPECIFIED., .F., .F.,
 ( 4, 2, 4 ),
 ( 0.000000000000000000, 0.0005356813221244592508, 0.001071362644248918502 ),
 .UNSPECIFIED. ) ;
#77459 = CARTESIAN_POINT ( 'NONE',  ( -104.3681639590162575, -277.5074553877019525, -299.6658236221556990 ) ) ;
#77460 = CIRCLE ( 'NONE', #83452, 28.04691768583012035 ) ;
#77461 = CARTESIAN_POINT ( 'NONE',  ( 30.13257583076671864, -295.4671337331292875, -299.9909987527423709 ) ) ;
#77462 = CARTESIAN_POINT ( 'NONE',  ( 14.96061581304658716, -279.6891171697345158, -214.1996500705374444 ) ) ;
#77463 = CARTESIAN_POINT ( 'NONE',  ( -92.35954251701267026, -296.8055902883151589, -318.6979100505135420 ) ) ;
#77464 = CARTESIAN_POINT ( 'NONE',  ( -76.81335628257380677, -296.8837969734492503, -335.9611801973882734 ) ) ;
#77465 = CARTESIAN_POINT ( 'NONE',  ( -107.2155191820545355, -272.5016592212732576, -248.9809439852922708 ) ) ;
#77466 = CARTESIAN_POINT ( 'NONE',  ( -112.3691769910507219, -292.5770464865422582, -268.4351378432108959 ) ) ;
#77467 = CARTESIAN_POINT ( 'NONE',  ( -54.96667055546318892, -285.9982447090957862, -195.4053949060794935 ) ) ;
#77468 = CARTESIAN_POINT ( 'NONE',  ( 31.44179341029144226, -273.2772771883630867, -238.4691902126157004 ) ) ;
#77469 = CARTESIAN_POINT ( 'NONE',  ( -65.44900140514982922, -289.2428097963760365, -342.1041383990375380 ) ) ;
#77470 = CARTESIAN_POINT ( 'NONE',  ( -75.36486859066312149, -281.5228309509111000, -206.0670845502641271 ) ) ;
#77471 = CARTESIAN_POINT ( 'NONE',  ( -38.61702128718089710, -285.0945527850954022, -197.1244058867658850 ) ) ;
#77472 = CARTESIAN_POINT ( 'NONE',  ( -109.6964322990371414, -288.8064335137029275, -250.5692621599298491 ) ) ;
#77473 = CARTESIAN_POINT ( 'NONE',  ( 22.29632774050155319, -23.10002859818378340, -338.8215327972035311 ) ) ;
#77474 = CARTESIAN_POINT ( 'NONE',  ( 31.90091445477538556, -286.7503814197424390, -247.0491303502828373 ) ) ;
#77475 = LINE ( 'NONE', #20181, #44485 ) ;
#77476 = CARTESIAN_POINT ( 'NONE',  ( 38.19619376431163715, -282.6657930535725995, -284.1033839688629996 ) ) ;
#77477 = CARTESIAN_POINT ( 'NONE',  ( -112.0365359206662390, -289.3880832818108502, -288.1233777822968705 ) ) ;
#77478 = CARTESIAN_POINT ( 'NONE',  ( -111.0483736974109519, -279.9071461720388925, -289.7453811506374564 ) ) ;
#77479 = CARTESIAN_POINT ( 'NONE',  ( -69.76869561916049634, -280.9492800978976561, -201.0518830684958402 ) ) ;
#77480 = CARTESIAN_POINT ( 'NONE',  ( 33.93995540664759147, -281.5931829933286394, -286.1067709943074533 ) ) ;
#77481 = CARTESIAN_POINT ( 'NONE',  ( 37.36812384980096624, -277.4604354034465246, -263.2052621739371716 ) ) ;
#77482 = CARTESIAN_POINT ( 'NONE',  ( -72.07403543291064807, -295.4987540259543835, -339.0827658402249654 ) ) ;
#77483 = CARTESIAN_POINT ( 'NONE',  ( -87.00497514474724881, -289.3772740435469473, -214.5653989026564261 ) ) ;
#77484 = CARTESIAN_POINT ( 'NONE',  ( -47.30119167050533235, -296.8430903940855501, -197.6802581844369229 ) ) ;
#77485 = ORIENTED_EDGE ( 'NONE', *, *, #32100, .T. ) ;
#77486 = ORIENTED_EDGE ( 'NONE', *, *, #63556, .F. ) ;
#77487 = CARTESIAN_POINT ( 'NONE',  ( 33.61117802323219195, -283.7670275350053544, -293.0459090269075659 ) ) ;
#77488 = CARTESIAN_POINT ( 'NONE',  ( -93.10128784045257078, -295.5488107609818371, -317.5287228185309232 ) ) ;
#77489 = CARTESIAN_POINT ( 'NONE',  ( 33.03526250480244641, -294.2419330457668707, -239.8885788777388086 ) ) ;
#77490 = CARTESIAN_POINT ( 'NONE',  ( -37.53246934173292715, -283.7060525861120936, -343.4752490306422033 ) ) ;
#77491 = CARTESIAN_POINT ( 'NONE',  ( -15.83176370678345712, -273.3824027561016692, -196.6164422370010527 ) ) ;
#77492 = CARTESIAN_POINT ( 'NONE',  ( -39.21753122765307609, -292.6806326328924115, -193.4729152999338169 ) ) ;
#77493 = CARTESIAN_POINT ( 'NONE',  ( -21.22327490183170084, -284.3963737000675565, -196.3307063532376162 ) ) ;
#77494 = CARTESIAN_POINT ( 'NONE',  ( -112.5437777050342874, -290.6797251057994913, -286.8047130811607985 ) ) ;
#77495 = CARTESIAN_POINT ( 'NONE',  ( 7.996389700461218553, -288.7457765152440174, -327.6022316804633761 ) ) ;
#77496 = DIRECTION ( 'NONE',  ( 1.049727191138620051E-16, 0.5150380749100522682, -0.8571673007021134438 ) ) ;
#77497 = CARTESIAN_POINT ( 'NONE',  ( 154.9842916688209868, 128.0000000000000568, -12.88888888888889461 ) ) ;
#77498 = CARTESIAN_POINT ( 'NONE',  ( -109.7947985209783184, -268.5820228192868058, -295.2857659021627228 ) ) ;
#77499 = CARTESIAN_POINT ( 'NONE',  ( -49.95962354570519182, -284.7303189076574199, -345.6707071636948285 ) ) ;
#77500 = CARTESIAN_POINT ( 'NONE',  ( -110.4542110544635705, -282.2666405000204009, -253.6410175316879361 ) ) ;
#77501 = ORIENTED_EDGE ( 'NONE', *, *, #47924, .T. ) ;
#77502 = CARTESIAN_POINT ( 'NONE',  ( 31.64081303228361008, -280.8033101443431860, -295.3232035731341512 ) ) ;
#77503 = CARTESIAN_POINT ( 'NONE',  ( 23.49872483143495572, -275.8490079095890906, -317.5437816025196298 ) ) ;
#77504 = CARTESIAN_POINT ( 'NONE',  ( -43.93743976431574083, -281.9688793267448546, -195.7675226082509141 ) ) ;
#77505 = CARTESIAN_POINT ( 'NONE',  ( -75.44914023181735274, -209.3092839176353834, -355.0955389360644290 ) ) ;
#77506 = CARTESIAN_POINT ( 'NONE',  ( 36.42100054318044045, -279.8746630386589231, -250.3697823562115445 ) ) ;
#77507 = CARTESIAN_POINT ( 'NONE',  ( -44.14984519467542867, -283.9857342012782624, -196.0274381112338631 ) ) ;
#77508 = CARTESIAN_POINT ( 'NONE',  ( -112.6452589435766214, -298.1785821128481189, -280.9116697671348675 ) ) ;
#77509 = CARTESIAN_POINT ( 'NONE',  ( 16.77954800854531570, -293.3411276293782066, -221.2065927208255971 ) ) ;
#77510 = ORIENTED_EDGE ( 'NONE', *, *, #49942, .T. ) ;
#77511 = CARTESIAN_POINT ( 'NONE',  ( -66.74610779413268347, -290.3434458811649392, -203.0066505072790051 ) ) ;
#77512 = CARTESIAN_POINT ( 'NONE',  ( -4.031487858280806691, -277.2757704414927389, -339.6846350234554279 ) ) ;
#77513 = CARTESIAN_POINT ( 'NONE',  ( -57.90681300412333599, -297.9456681201089054, -200.3177304510961108 ) ) ;
#77514 = ORIENTED_EDGE ( 'NONE', *, *, #81207, .F. ) ;
#77515 = CARTESIAN_POINT ( 'NONE',  ( -71.25369382832650444, -272.5352302795299124, -201.5754421881898395 ) ) ;
#77516 = CARTESIAN_POINT ( 'NONE',  ( -48.18343439339133027, -291.0521521680024080, -435.6442049081568939 ) ) ;
#77517 = VECTOR ( 'NONE', #89738, 1000.000000000000114 ) ;
#77518 = CARTESIAN_POINT ( 'NONE',  ( 156.6530531571616791, 18.17946993580249782, 9.832064661605528499 ) ) ;
#77519 = VECTOR ( 'NONE', #10301, 1000.000000000000000 ) ;
#77520 = CARTESIAN_POINT ( 'NONE',  ( 22.84638299952234775, -283.2126858954650288, -312.2134861756413784 ) ) ;
#77521 = CARTESIAN_POINT ( 'NONE',  ( 10.86723799987209915, -284.1564117300929411, -329.1648366521967546 ) ) ;
#77522 = CARTESIAN_POINT ( 'NONE',  ( -95.31001273124209661, -282.9825817881678063, -315.1374100938461993 ) ) ;
#77523 = CARTESIAN_POINT ( 'NONE',  ( 26.18118139920536791, -282.8913964389785178, -231.8465947934172675 ) ) ;
#77524 = CARTESIAN_POINT ( 'NONE',  ( 35.79168975985043488, -274.1558180669345575, -279.8344837313644575 ) ) ;
#77526 = LINE ( 'NONE', #5572, #3437 ) ;
#77525 = AXIS2_PLACEMENT_3D ( 'NONE', #84522, #48537, #77438 ) ;
#77527 = CARTESIAN_POINT ( 'NONE',  ( 25.53390351464331687, -276.1143329836826297, -232.5682004054660297 ) ) ;
#77528 = DIRECTION ( 'NONE',  ( 0.000000000000000000, 1.000000000000000000, 0.000000000000000000 ) ) ;
#77529 = AXIS2_PLACEMENT_3D ( 'NONE', #12187, #4616, #27819 ) ;
#77530 = CARTESIAN_POINT ( 'NONE',  ( -56.87309220113347408, -278.1005115891152286, -344.7308129160258545 ) ) ;
#77531 = ORIENTED_EDGE ( 'NONE', *, *, #79929, .T. ) ;
#77532 = ORIENTED_EDGE ( 'NONE', *, *, #60248, .T. ) ;
#77533 = CARTESIAN_POINT ( 'NONE',  ( 195.4781563537916043, 27.48493576247232895, 15.00000000000000000 ) ) ;
#77534 = CARTESIAN_POINT ( 'NONE',  ( -111.1616828378459729, -286.6293528005825806, -253.3048687552398235 ) ) ;
#77535 = CARTESIAN_POINT ( 'NONE',  ( -82.46742585626191158, -294.8834249094667825, -328.0127857633279973 ) ) ;
#77536 = CARTESIAN_POINT ( 'NONE',  ( 3.119437538161993206, -287.8728050301662051, -335.8163091276400678 ) ) ;
#77537 = ADVANCED_FACE ( 'NONE', ( #74536 ), #75691, .T. ) ;
#77538 = CARTESIAN_POINT ( 'NONE',  ( -94.89608127450399877, -283.4413473251815390, -223.8064584945653905 ) ) ;
#77540 = CARTESIAN_POINT ( 'NONE',  ( -2.914725045224477284, -286.8308839122032055, -335.9370060928645216 ) ) ;
#77539 = CARTESIAN_POINT ( 'NONE',  ( -104.6595739868808437, -282.7300381500899107, -300.0878529975846618 ) ) ;
#77541 = CARTESIAN_POINT ( 'NONE',  ( -110.2654406331460706, -285.6423026439239834, -279.1208975253079529 ) ) ;
#77542 = CARTESIAN_POINT ( 'NONE',  ( 11.38540089847801084, -274.3764101281125818, -327.3757676031328288 ) ) ;
#77543 = CARTESIAN_POINT ( 'NONE',  ( -10.25903341187131979, -284.7995405243312348, -199.0801187794445184 ) ) ;
#77544 = CARTESIAN_POINT ( 'NONE',  ( -21.07843767550062708, -300.2558935330509371, -195.3555647147243519 ) ) ;
#77545 = CARTESIAN_POINT ( 'NONE',  ( -21.34860693657575581, -284.2566516374712364, -196.9155640420842417 ) ) ;
#77546 = CARTESIAN_POINT ( 'NONE',  ( -39.72084680147518299, -280.9628309990401362, -197.1519179504336421 ) ) ;
#77547 = CARTESIAN_POINT ( 'NONE',  ( 37.27397641609041301, -289.6740782640075054, -279.8654853146505275 ) ) ;
#77548 = CARTESIAN_POINT ( 'NONE',  ( 193.6287975281925071, 275.6568570078858329, 16.89650703334467963 ) ) ;
#77549 = DIRECTION ( 'NONE',  ( 1.000000000000000000, 0.000000000000000000, 0.000000000000000000 ) ) ;
#77550 = CARTESIAN_POINT ( 'NONE',  ( -66.34859727899481641, -297.3490992430853908, -340.1454904656250164 ) ) ;
#77551 = VECTOR ( 'NONE', #10853, 1000.000000000000000 ) ;
#77552 = VECTOR ( 'NONE', #58380, 1000.000000000000000 ) ;
#77553 = CARTESIAN_POINT ( 'NONE',  ( -11.01795387066295184, -278.3949851673045259, -200.0775535118540347 ) ) ;
#77554 = CARTESIAN_POINT ( 'NONE',  ( -111.8354981165519604, -289.9861155769526704, -251.4711408001130621 ) ) ;
#77555 = CARTESIAN_POINT ( 'NONE',  ( -70.09726791484126807, -293.8910117257324259, -336.4936606259843757 ) ) ;
#77556 = CARTESIAN_POINT ( 'NONE',  ( -49.20513046525081791, -278.5826102365383576, -197.8317963427482766 ) ) ;
#77557 = CARTESIAN_POINT ( 'NONE',  ( -35.75929806470490746, -296.2117496729896402, -196.1264183674259982 ) ) ;
#77558 = CARTESIAN_POINT ( 'NONE',  ( 33.22837610134417474, -295.1374886194453779, -290.9272985017212818 ) ) ;
#77559 = CARTESIAN_POINT ( 'NONE',  ( -54.42813229853332757, -291.7662352645559167, -345.3683826091709648 ) ) ;
#77560 = CARTESIAN_POINT ( 'NONE',  ( -111.5951682169763473, -295.2539372854956241, -252.7790182125252443 ) ) ;
#77561 = CARTESIAN_POINT ( 'NONE',  ( -3.748867461086582420, -290.7291090862343026, -202.1888963750468236 ) ) ;
#77562 = ADVANCED_FACE ( 'NONE', ( #46114 ), #2114, .T. ) ;
#77563 = CARTESIAN_POINT ( 'NONE',  ( -108.6841585681019922, -292.2142887924738375, -252.2646370473189847 ) ) ;
#77564 = CARTESIAN_POINT ( 'NONE',  ( 175.2296996224750103, 140.2072866198470251, 0.000000000000000000 ) ) ;
#77565 = CARTESIAN_POINT ( 'NONE',  ( -30.80269962062244815, -292.9397581282994452, -197.4924470784148980 ) ) ;
#77566 = CARTESIAN_POINT ( 'NONE',  ( -105.6569842320517552, -292.2070231878549862, -235.5882255541883978 ) ) ;
#77568 = CARTESIAN_POINT ( 'NONE',  ( 8.848840249748281650, -292.7059267529546105, -213.7673825572400688 ) ) ;
#77567 = CARTESIAN_POINT ( 'NONE',  ( 35.02731207708480099, -279.3025990722478582, -249.3116408422868062 ) ) ;
#77569 = CARTESIAN_POINT ( 'NONE',  ( -38.16990651973561910, -280.0420416017230423, -193.3655721752028853 ) ) ;
#77570 = CARTESIAN_POINT ( 'NONE',  ( -38.73642072112740919, -282.7359182163079367, -347.3273381450512716 ) ) ;
#77571 = CARTESIAN_POINT ( 'NONE',  ( -95.54590254773420099, -287.9030632454436045, -317.3962033094007325 ) ) ;
#77572 = CARTESIAN_POINT ( 'NONE',  ( -13.14883539007644941, -280.8742238869150469, -340.5980335969160819 ) ) ;
#77573 = CARTESIAN_POINT ( 'NONE',  ( -77.11446277149565276, -278.0096369106523184, -205.1782616642073265 ) ) ;
#77574 = CARTESIAN_POINT ( 'NONE',  ( 24.46235161041294504, -285.8669373949409191, -224.9546019395624796 ) ) ;
#77575 = CARTESIAN_POINT ( 'NONE',  ( 196.1601127431574412, 41.43610473273403727, 14.06370431049791137 ) ) ;
#77576 = CARTESIAN_POINT ( 'NONE',  ( 25.51871704263546192, -294.6238995836630465, -231.5988065330656411 ) ) ;
#77577 = CARTESIAN_POINT ( 'NONE',  ( 37.36543594177911842, -276.7744240220985716, -254.2540778325939073 ) ) ;
#77578 = CARTESIAN_POINT ( 'NONE',  ( -109.9255271171182500, -278.1077361699048538, -278.7880431935706724 ) ) ;
#77579 = CARTESIAN_POINT ( 'NONE',  ( -111.6333564419386022, -290.9729238740556525, -250.0688033837156752 ) ) ;
#77580 = VECTOR ( 'NONE', #37356, 1000.000000000000000 ) ;
#77581 = CARTESIAN_POINT ( 'NONE',  ( -33.16328871464007477, -281.0797917528433914, -345.8183914831684547 ) ) ;
#77582 = CARTESIAN_POINT ( 'NONE',  ( 2.378148933008505939, -291.6571635687413959, -208.7726550309245397 ) ) ;
#77583 = CARTESIAN_POINT ( 'NONE',  ( -107.5739001937540564, -294.2085732501393522, -296.8220079075608737 ) ) ;
#77584 = ORIENTED_EDGE ( 'NONE', *, *, #65290, .F. ) ;
#77585 = DIRECTION ( 'NONE',  ( 0.000000000000000000, 0.000000000000000000, 1.000000000000000000 ) ) ;
#77586 = AXIS2_PLACEMENT_3D ( 'NONE', #74480, #74017, #81572 ) ;
#77587 = CARTESIAN_POINT ( 'NONE',  ( -75.00596157585009394, -291.0437860298532655, -207.6970091394162523 ) ) ;
#77588 = CARTESIAN_POINT ( 'NONE',  ( 208.4306832106271088, -74.55766379199613425, -7.500000000000013323 ) ) ;
#77589 = CARTESIAN_POINT ( 'NONE',  ( -102.0172624299486870, -298.6233781216987495, -301.5434626090942061 ) ) ;
#77590 = CARTESIAN_POINT ( 'NONE',  ( -113.8851927030090252, -295.6922264361884345, -263.8783595288938386 ) ) ;
#77591 = CARTESIAN_POINT ( 'NONE',  ( 18.26988535788170154, -278.9794544989266569, -218.9057291438649884 ) ) ;
#77592 = AXIS2_PLACEMENT_3D ( 'NONE', #80576, #65948, #51687 ) ;
#77593 = CARTESIAN_POINT ( 'NONE',  ( -87.98249520661562428, -285.0579179958273812, -327.7799726252342225 ) ) ;
#77594 = CARTESIAN_POINT ( 'NONE',  ( -9.491425486574028625, -286.2598194801654472, -202.8690043349675420 ) ) ;
#77595 = AXIS2_PLACEMENT_3D ( 'NONE', #69307, #33315, #3980 ) ;
#77596 = CARTESIAN_POINT ( 'NONE',  ( -94.12803802724369007, -279.4124638351806880, -317.3491652886649490 ) ) ;
#77597 = CARTESIAN_POINT ( 'NONE',  ( -109.0322021264194632, -294.8412171737081167, -249.5688423183820817 ) ) ;
#77598 = CARTESIAN_POINT ( 'NONE',  ( -111.2251547171315309, -298.3693256925972719, -265.9782936212701543 ) ) ;
#77599 = CARTESIAN_POINT ( 'NONE',  ( -73.04852903633221217, -276.3315117055853989, -334.5016495862799388 ) ) ;
#77600 = ORIENTED_EDGE ( 'NONE', *, *, #24713, .F. ) ;
#77601 = DIRECTION ( 'NONE',  ( 0.000000000000000000, 1.000000000000000000, 0.000000000000000000 ) ) ;
#77602 = CARTESIAN_POINT ( 'NONE',  ( -114.2129711458231611, -296.1566646993842369, -275.3337762793937600 ) ) ;
#77603 = CARTESIAN_POINT ( 'NONE',  ( -104.1267933230056997, -292.0353779681522042, -303.2406788346667668 ) ) ;
#77604 = CARTESIAN_POINT ( 'NONE',  ( -112.7724044462825219, -274.5149434905746944, -270.3861090177667847 ) ) ;
#77605 = AXIS2_PLACEMENT_3D ( 'NONE', #46088, #18153, #67886 ) ;
#77606 = ORIENTED_EDGE ( 'NONE', *, *, #54222, .F. ) ;
#77607 = CARTESIAN_POINT ( 'NONE',  ( 1.266038376184138503, -279.6129928427387767, -203.9510439291099146 ) ) ;
#77608 = CARTESIAN_POINT ( 'NONE',  ( -113.8409726979541858, -297.1056167466742863, -278.1825042208197374 ) ) ;
#77609 = CARTESIAN_POINT ( 'NONE',  ( -81.19583560464567995, -289.6026993450278724, -208.5782702029881364 ) ) ;
#77610 = CARTESIAN_POINT ( 'NONE',  ( -40.44365699919875112, -298.3475708375403315, -193.3926738376565879 ) ) ;
#77611 = CARTESIAN_POINT ( 'NONE',  ( 24.86365848257481304, -293.3572564928084034, -232.0214321816955874 ) ) ;
#77612 = CARTESIAN_POINT ( 'NONE',  ( 198.0296422097436846, 67.77566895945791714, -9.842458531120671594 ) ) ;
#77613 = CIRCLE ( 'NONE', #8052, 4.000000000000003553 ) ;
#77614 = DIRECTION ( 'NONE',  ( -0.3994899938748465162, 0.000000000000000000, -0.9167375550253601402 ) ) ;
#77615 = CARTESIAN_POINT ( 'NONE',  ( 138.6539576904058606, 130.8284271247462414, 11.67157287525380838 ) ) ;
#77616 = CARTESIAN_POINT ( 'NONE',  ( -54.32826532151603516, -290.7864940015391539, -344.8072986019737414 ) ) ;
#77617 = CARTESIAN_POINT ( 'NONE',  ( -37.30987171927208124, -279.5519495502701375, -350.3611179825600175 ) ) ;
#77618 = VERTEX_POINT ( 'NONE', #9188 ) ;
#77619 = CARTESIAN_POINT ( 'NONE',  ( 38.56588731261480518, -281.0558342886508285, -282.7457948011403914 ) ) ;
#77620 = CARTESIAN_POINT ( 'NONE',  ( -111.9208386496081573, -286.4730103291483374, -276.5239518980328057 ) ) ;
#77621 = CARTESIAN_POINT ( 'NONE',  ( 37.45053337412381467, -285.9289307630767212, -254.6539061944536684 ) ) ;
#77622 = CARTESIAN_POINT ( 'NONE',  ( -86.49567292929069140, -271.3678742391825267, -213.8658793018547328 ) ) ;
#77623 = CARTESIAN_POINT ( 'NONE',  ( -94.90724018450953281, -275.1280904704206023, -223.1445398048015534 ) ) ;
#77624 = CARTESIAN_POINT ( 'NONE',  ( -110.6914914859981849, -288.8000041624377445, -257.3739644369967436 ) ) ;
#77625 = CARTESIAN_POINT ( 'NONE',  ( -103.8793326444933172, -279.9359788209610542, -306.5971351089248742 ) ) ;
#77627 = CARTESIAN_POINT ( 'NONE',  ( -32.94861105629794196, -279.4575439087968221, -197.3913061646499045 ) ) ;
#77626 = CARTESIAN_POINT ( 'NONE',  ( -110.1683457724123230, -278.4767253480942486, -276.0788831266825696 ) ) ;
#77628 = CARTESIAN_POINT ( 'NONE',  ( -17.42487434981083894, -277.8806484263906214, -344.4206383687808852 ) ) ;
#77629 = CARTESIAN_POINT ( 'NONE',  ( -81.99489083885298157, -278.2532004084110895, -208.1188391287203387 ) ) ;
#77630 = CARTESIAN_POINT ( 'NONE',  ( -72.06482525295078290, -195.1395164891845297, -357.9071827626919458 ) ) ;
#77631 = CARTESIAN_POINT ( 'NONE',  ( 98.82013943189359395, -300.5191071293656364, -193.5044647189510840 ) ) ;
#77632 = EDGE_CURVE ( 'NONE', #20922, #37280, #89187, .T. ) ;
#77633 = CONTEXT_DEPENDENT_SHAPE_REPRESENTATION ( #18462, #7398 ) ;
#77634 = CARTESIAN_POINT ( 'NONE',  ( 97.87027569496429180, -301.1390480024426779, -193.9182337029051837 ) ) ;
#77635 = CARTESIAN_POINT ( 'NONE',  ( 39.58706461736021254, -290.0519495502703080, -270.3284710469133074 ) ) ;
#77636 = ORIENTED_EDGE ( 'NONE', *, *, #10818, .F. ) ;
#77637 = CARTESIAN_POINT ( 'NONE',  ( 188.7399167944524550, 8.542400036368780647, 13.00000000000000178 ) ) ;
#77638 = CARTESIAN_POINT ( 'NONE',  ( 34.00799630816176489, -288.4099563119616505, -253.4710270386866284 ) ) ;
#77639 = CARTESIAN_POINT ( 'NONE',  ( 36.38808773228214477, -289.0792462829769534, -251.9792682727587305 ) ) ;
#77640 = CARTESIAN_POINT ( 'NONE',  ( -37.27624396484597469, -288.3998967430293874, -343.4630220896499395 ) ) ;
#77641 = CARTESIAN_POINT ( 'NONE',  ( -99.29095730970597344, -284.6674710412652871, -224.6465403266671785 ) ) ;
#77642 = CARTESIAN_POINT ( 'NONE',  ( 21.16247624817584949, -279.3255753297187880, -225.3549980517821041 ) ) ;
#77643 = CARTESIAN_POINT ( 'NONE',  ( -9.044108566336742427, -288.2865880865172130, -201.7171295329684426 ) ) ;
#77644 = CARTESIAN_POINT ( 'NONE',  ( 30.66873245133542625, -279.6549542470181109, -241.9835068926161057 ) ) ;
#77645 = CARTESIAN_POINT ( 'NONE',  ( -95.18933739385968806, -280.5023578947685223, -225.0099136557651889 ) ) ;
#77646 = CARTESIAN_POINT ( 'NONE',  ( -89.12501638499873025, -278.2968334431417361, -321.9739716885067651 ) ) ;
#77647 = CARTESIAN_POINT ( 'NONE',  ( 2.958121926282671232, -287.3192317577753556, -335.5688122964978106 ) ) ;
#77648 = CARTESIAN_POINT ( 'NONE',  ( 0.7971106087138253304, -283.3597769747145776, -337.0815659215375604 ) ) ;
#77649 = CARTESIAN_POINT ( 'NONE',  ( -92.38532991824372687, -284.3064911333286204, -324.1172871420218939 ) ) ;
#77650 = CARTESIAN_POINT ( 'NONE',  ( 11.91825224058169752, -282.5110361062631910, -324.2355747976889120 ) ) ;
#77651 = ORIENTED_EDGE ( 'NONE', *, *, #80097, .F. ) ;
#77652 = ORIENTED_EDGE ( 'NONE', *, *, #57360, .T. ) ;
#77653 = CARTESIAN_POINT ( 'NONE',  ( 194.7155524329731122, 19.93649182339144232, -14.17849501842133719 ) ) ;
#77654 = CARTESIAN_POINT ( 'NONE',  ( -111.3535624238246271, -292.2066126722993999, -286.5645041727724447 ) ) ;
#77655 = VECTOR ( 'NONE', #28760, 1000.000000000000000 ) ;
#77656 = CARTESIAN_POINT ( 'NONE',  ( 17.15020131634659251, -291.4940543938898827, -216.5842576658749294 ) ) ;
#77657 = CARTESIAN_POINT ( 'NONE',  ( -13.97907046121468966, -273.4215907156046228, -200.9522137781057438 ) ) ;
#77658 = CARTESIAN_POINT ( 'NONE',  ( 23.94271087561843459, -293.5204018280648484, -316.8103779863600380 ) ) ;
#77659 = CARTESIAN_POINT ( 'NONE',  ( -103.4760910022184675, -288.5956555767142504, -302.8718868784371239 ) ) ;
#77660 = CARTESIAN_POINT ( 'NONE',  ( 35.71778792059226504, -291.6368684180904438, -258.4375140722710853 ) ) ;
#77661 = CARTESIAN_POINT ( 'NONE',  ( -109.0473625289618695, -291.5509763127051883, -286.0856443043307991 ) ) ;
#77662 = DIRECTION ( 'NONE',  ( 0.000000000000000000, 0.000000000000000000, 1.000000000000000000 ) ) ;
#77663 = CARTESIAN_POINT ( 'NONE',  ( -104.2322080542952705, -293.0019800083869654, -236.3251439875608924 ) ) ;
#77664 = CARTESIAN_POINT ( 'NONE',  ( -110.5263150196137332, -288.7716880657255274, -253.2135066475688632 ) ) ;
#77665 = CARTESIAN_POINT ( 'NONE',  ( -29.01272374781387953, -294.1577551507367616, -195.7734868572562732 ) ) ;
#77666 = CARTESIAN_POINT ( 'NONE',  ( 20.51920604996066899, -287.8630761712044546, -225.4665305011370720 ) ) ;
#77667 = CARTESIAN_POINT ( 'NONE',  ( 10.06234116798146516, -296.4011405614946284, -328.7624660474543248 ) ) ;
#77668 = AXIS2_PLACEMENT_3D ( 'NONE', #26785, #25368, #83119 ) ;
#77669 = CARTESIAN_POINT ( 'NONE',  ( 3.940544494944215437, -276.5845743567022623, -207.2580977677613419 ) ) ;
#77670 = CARTESIAN_POINT ( 'NONE',  ( -102.1746539962912124, -296.2910279576142898, -229.1197926763808539 ) ) ;
#77671 = CARTESIAN_POINT ( 'NONE',  ( 33.47958729538950706, -274.0733400833900646, -291.9066178841515011 ) ) ;
#77672 = CARTESIAN_POINT ( 'NONE',  ( 14.35235124876298052, -278.8650816931276495, -216.7258482153007151 ) ) ;
#77673 = CARTESIAN_POINT ( 'NONE',  ( -94.93377901851911815, -274.3958067380647208, -224.8607558379044633 ) ) ;
#77674 = CARTESIAN_POINT ( 'NONE',  ( -1.561216526088839540, -273.0917775835797556, -202.8454658172614984 ) ) ;
#77675 = CIRCLE ( 'NONE', #64128, 5.568361562975243650 ) ;
#77676 = CARTESIAN_POINT ( 'NONE',  ( -109.1630091193064231, -297.7676108451970549, -286.3946607564227520 ) ) ;
#77677 = CARTESIAN_POINT ( 'NONE',  ( 196.2452211277167748, 71.67373103464963435, 13.59235650557800135 ) ) ;
#77678 = CARTESIAN_POINT ( 'NONE',  ( -102.9083441053576990, -296.9145749786466126, -302.9350358127435356 ) ) ;
#77679 = DIRECTION ( 'NONE',  ( 0.7071067811864494290, 0.000000000000000000, 0.7071067811866457165 ) ) ;
#77681 = CARTESIAN_POINT ( 'NONE',  ( -108.5344255438734393, -272.5984244505103220, -254.2181364607774583 ) ) ;
#77680 = CARTESIAN_POINT ( 'NONE',  ( 28.70241879707406696, -285.0908619848139551, -233.9680596373990795 ) ) ;
#77682 = CIRCLE ( 'NONE', #14238, 3.491568894204821749 ) ;
#77683 = CARTESIAN_POINT ( 'NONE',  ( 5.179676330621761693, -286.6097201150020055, -206.1031211403636974 ) ) ;
#77684 = CARTESIAN_POINT ( 'NONE',  ( -70.63376909783086433, -289.1458729638741829, -339.7829659757355785 ) ) ;
#77685 = CARTESIAN_POINT ( 'NONE',  ( -74.98069705552798325, -299.5337533976257873, -205.0194274155513483 ) ) ;
#77686 = CARTESIAN_POINT ( 'NONE',  ( -69.32342310327962309, -293.4736863280037369, -338.0301870168362939 ) ) ;
#77687 = CARTESIAN_POINT ( 'NONE',  ( 34.17788284581840941, -280.3908214287328633, -242.1247786582720494 ) ) ;
#77688 = CARTESIAN_POINT ( 'NONE',  ( -95.95921662488163406, -288.6952119285919025, -223.5744983911110353 ) ) ;
#77689 = CARTESIAN_POINT ( 'NONE',  ( 208.4306832106270804, -198.2391364535880598, -7.500000000000012434 ) ) ;
#77690 = CIRCLE ( 'NONE', #55041, 1.000000000000000888 ) ;
#77691 = CARTESIAN_POINT ( 'NONE',  ( 18.11552068165402218, -287.0292726596195507, -318.5165774165824359 ) ) ;
#77692 = EDGE_CURVE ( 'NONE', #22214, #17985, #80225, .T. ) ;
#77693 = DIRECTION ( 'NONE',  ( 0.000000000000000000, 0.000000000000000000, 1.000000000000000000 ) ) ;
#77694 = CARTESIAN_POINT ( 'NONE',  ( -74.55896841310922696, -287.5470648371380094, -335.4902537927671347 ) ) ;
#77695 = CARTESIAN_POINT ( 'NONE',  ( -109.2153664135543920, -274.2849532673811268, -254.0858653124740272 ) ) ;
#77696 = CARTESIAN_POINT ( 'NONE',  ( -6.485081694435876898, -281.8747592092881291, -200.4436278864384633 ) ) ;
#77698 = CARTESIAN_POINT ( 'NONE',  ( 33.11358151885879408, -281.2991890548242964, -251.2069255579692992 ) ) ;
#77697 = CARTESIAN_POINT ( 'NONE',  ( -102.9665184239086955, -271.1289390746248387, -232.8035707031289405 ) ) ;
#77699 = CARTESIAN_POINT ( 'NONE',  ( -88.60384951804989839, -295.9143477658249708, -327.8886170038253454 ) ) ;
#77700 = CARTESIAN_POINT ( 'NONE',  ( -108.5146180578946087, -274.2247276866234529, -251.4628462230623143 ) ) ;
#77701 = EDGE_CURVE ( 'NONE', #28617, #6151, #24820, .T. ) ;
#77702 = CARTESIAN_POINT ( 'NONE',  ( 35.60913324842847061, -283.7765328666387745, -287.8279445386277189 ) ) ;
#77703 = CARTESIAN_POINT ( 'NONE',  ( -35.12682494449100545, -297.1392939730989724, -197.1261868491516793 ) ) ;
#77704 = ORIENTED_EDGE ( 'NONE', *, *, #10535, .T. ) ;
#77705 = LINE ( 'NONE', #28912, #46802 ) ;
#77706 = CARTESIAN_POINT ( 'NONE',  ( -109.6811386451170733, -286.2944316258024173, -288.7690630320087735 ) ) ;
#77707 = CARTESIAN_POINT ( 'NONE',  ( 191.4749582765727212, 14.19731191252289015, 13.00000000000000178 ) ) ;
#77708 = CARTESIAN_POINT ( 'NONE',  ( -55.63300648810263738, -274.7666405000204009, -350.3538533559490702 ) ) ;
#77709 = CARTESIAN_POINT ( 'NONE',  ( 10.41767779954267148, -275.6093752139835260, -330.6220813604535920 ) ) ;
#77710 = CARTESIAN_POINT ( 'NONE',  ( -71.71528547095849149, -285.0352177387784991, -335.5467328413386099 ) ) ;
#77711 = CARTESIAN_POINT ( 'NONE',  ( 28.75598869072684849, -277.5939111845766547, -303.3022290863825674 ) ) ;
#77712 = CARTESIAN_POINT ( 'NONE',  ( -65.02168542937295115, -284.8320352078922610, -341.5961685025373527 ) ) ;
#77713 = CARTESIAN_POINT ( 'NONE',  ( -85.13187999667241002, -282.5244508506763736, -326.0677532411175434 ) ) ;
#77714 = CARTESIAN_POINT ( 'NONE',  ( -1.019187615599564056, -282.5344932064879799, -204.7434699374900617 ) ) ;
#77715 = CARTESIAN_POINT ( 'NONE',  ( 32.55216893130537414, -275.3040469787976576, -237.9255313598904706 ) ) ;
#77716 = CARTESIAN_POINT ( 'NONE',  ( 26.06567488523061016, -275.9632682556931513, -314.1398373039746730 ) ) ;
#77717 = CARTESIAN_POINT ( 'NONE',  ( -104.0479078780042954, -298.0317166746140174, -303.5168368878861997 ) ) ;
#77718 = DIRECTION ( 'NONE',  ( 0.000000000000000000, 0.000000000000000000, 1.000000000000000000 ) ) ;
#77719 = CARTESIAN_POINT ( 'NONE',  ( 185.7724743053495615, 214.9732557907763635, 23.01307087489506742 ) ) ;
#77720 = CARTESIAN_POINT ( 'NONE',  ( -106.0562381696035601, -294.2766238441584505, -302.2769093644306508 ) ) ;
#77721 = CARTESIAN_POINT ( 'NONE',  ( 20.88216690037645407, -275.6795270999575678, -314.4969282740946142 ) ) ;
#77722 = CIRCLE ( 'NONE', #14215, 2.000000000000001776 ) ;
#77723 = CARTESIAN_POINT ( 'NONE',  ( -69.23157864404510065, -287.3869056968936775, -203.5563443510324930 ) ) ;
#77724 = CARTESIAN_POINT ( 'NONE',  ( 8.505167781035055441, -295.9570183292405545, -331.3592528217970425 ) ) ;
#77725 = CARTESIAN_POINT ( 'NONE',  ( 29.12346494758562798, -294.2598354576129509, -232.2771246368934044 ) ) ;
#77726 = CARTESIAN_POINT ( 'NONE',  ( -111.4346355418993113, -292.4160058650974747, -280.9535615949628777 ) ) ;
#77727 = CARTESIAN_POINT ( 'NONE',  ( -112.1129699557743038, -276.5127736120763871, -273.4083514812512590 ) ) ;
#77728 = CIRCLE ( 'NONE', #50488, 4.999999999999977796 ) ;
#77729 = CARTESIAN_POINT ( 'NONE',  ( -77.62120398176004699, -281.4274812970101038, -207.6987335635573686 ) ) ;
#77730 = CARTESIAN_POINT ( 'NONE',  ( -110.3008771213403207, -294.4400511559276765, -285.1987532809184813 ) ) ;
#77731 = CARTESIAN_POINT ( 'NONE',  ( -83.11775814082450609, -285.5313574879745033, -330.7996654721629852 ) ) ;
#77732 = CARTESIAN_POINT ( 'NONE',  ( -46.75097764371336950, -284.8503500048736328, -197.6073663542804866 ) ) ;
#77733 = CARTESIAN_POINT ( 'NONE',  ( -54.19524147295266658, -170.4633805983236243, -363.5514204490719976 ) ) ;
#77734 = ORIENTED_EDGE ( 'NONE', *, *, #66553, .F. ) ;
#77735 = CARTESIAN_POINT ( 'NONE',  ( -106.1950888416815815, -283.8935605391519630, -294.8283413578931800 ) ) ;
#77736 = ORIENTED_EDGE ( 'NONE', *, *, #13462, .F. ) ;
#77737 = CARTESIAN_POINT ( 'NONE',  ( 0.7269116491058242868, -283.6365711119959201, -336.9516109343309722 ) ) ;
#77738 = CARTESIAN_POINT ( 'NONE',  ( -99.01537480441263028, -283.9548576862641198, -224.8385612877828237 ) ) ;
#77739 = CIRCLE ( 'NONE', #36916, 25.00000000000000355 ) ;
#77740 = CARTESIAN_POINT ( 'NONE',  ( -111.5068200340285358, -279.7427459786285908, -250.5023810691645565 ) ) ;
#77741 = CARTESIAN_POINT ( 'NONE',  ( -12.07731067674798453, -278.2494985195435788, -342.4194524159306070 ) ) ;
#77742 = CARTESIAN_POINT ( 'NONE',  ( -2.443822705920469573, -281.1529579519755657, -201.8230499438094228 ) ) ;
#77743 = CARTESIAN_POINT ( 'NONE',  ( -21.33282851196157992, -271.7666405000204009, -200.3683826091710216 ) ) ;
#77744 = CARTESIAN_POINT ( 'NONE',  ( -62.74176713377130454, -183.3418054874163374, -362.5124067139283852 ) ) ;
#77745 = CARTESIAN_POINT ( 'NONE',  ( -63.98262090302324623, -275.7040825150743331, -200.4166767126971820 ) ) ;
#77746 = CARTESIAN_POINT ( 'NONE',  ( 184.7839567310230393, 263.7331535000452050, -153.2007708629784304 ) ) ;
#77747 = CIRCLE ( 'NONE', #36924, 1.000000000000000888 ) ;
#77748 = CARTESIAN_POINT ( 'NONE',  ( -57.53447368128914974, -277.8102896992081128, -198.4994543767004984 ) ) ;
#77749 = CARTESIAN_POINT ( 'NONE',  ( 14.72725970433147502, -294.5331989152616643, -214.9463461217171130 ) ) ;
#77750 = CARTESIAN_POINT ( 'NONE',  ( -39.70062654329873197, -294.4311075229616677, -343.4374290788379085 ) ) ;
#77751 = CARTESIAN_POINT ( 'NONE',  ( -114.1260278879859413, -290.1207313203814806, -265.4934785606679384 ) ) ;
#77752 = DIRECTION ( 'NONE',  ( 0.9531768234071978929, -0.3024135303179465439, -0.000000000000000000 ) ) ;
#77753 = EDGE_CURVE ( 'NONE', #13434, #76692, #66975, .T. ) ;
#77755 = CARTESIAN_POINT ( 'NONE',  ( -54.92743348445259244, -284.2222797707517543, -198.6341100497998582 ) ) ;
#77754 = CARTESIAN_POINT ( 'NONE',  ( -61.42321264789228508, -293.9335327574731878, -342.9332408237028744 ) ) ;
#77756 = CARTESIAN_POINT ( 'NONE',  ( -73.24477305733812216, -293.4315744566847002, -205.3276969249216961 ) ) ;
#77757 = ADVANCED_FACE ( 'NONE', ( #59416 ), #90128, .T. ) ;
#77758 = CARTESIAN_POINT ( 'NONE',  ( -49.51719730274771791, -284.3741141461949837, -197.6285641248489071 ) ) ;
#77759 = CARTESIAN_POINT ( 'NONE',  ( -104.5576213484313115, -285.4700433977267835, -300.0808658138208784 ) ) ;
#77760 = CARTESIAN_POINT ( 'NONE',  ( -84.13244910653557440, -292.3681377695119750, -209.4381703824881242 ) ) ;
#77761 = CARTESIAN_POINT ( 'NONE',  ( -64.07205397518960410, -283.9028455087408247, -338.3572695274557418 ) ) ;
#77762 = CARTESIAN_POINT ( 'NONE',  ( -113.8382851596718268, -295.2850104998828442, -275.2984077688835214 ) ) ;
#77763 = CIRCLE ( 'NONE', #56622, 1.895975569037589015 ) ;
#77764 = CARTESIAN_POINT ( 'NONE',  ( -105.0089236347139945, -290.8833014963769870, -306.7658660648459090 ) ) ;
#77765 = CARTESIAN_POINT ( 'NONE',  ( -73.13966934655017837, -290.0060818592173177, -338.4789626690590012 ) ) ;
#77766 = CARTESIAN_POINT ( 'NONE',  ( 21.99033934664551282, -287.1233763233467471, -227.7469768085139208 ) ) ;
#77767 = ORIENTED_EDGE ( 'NONE', *, *, #71269, .F. ) ;
#77768 = DIRECTION ( 'NONE',  ( -0.000000000000000000, 1.000000000000000000, -0.000000000000000000 ) ) ;
#77769 = CARTESIAN_POINT ( 'NONE',  ( -110.3946422607836126, -298.1568118272001584, -290.4502475818501921 ) ) ;
#77770 = CARTESIAN_POINT ( 'NONE',  ( -77.92658435468045752, -296.2037043965462999, -205.5061610055302310 ) ) ;
#77771 = CARTESIAN_POINT ( 'NONE',  ( 23.88581452348766732, -280.0545185465205691, -230.0875585399231795 ) ) ;
#77772 = CARTESIAN_POINT ( 'NONE',  ( 32.96099562826828588, -275.4590792988642534, -301.6190429368886612 ) ) ;
#77773 = B_SPLINE_CURVE_WITH_KNOTS ( 'NONE', 3,
 ( #81818, #45833, #44900, #74737, #75200, #24530, #9858, #38732, #67638, #15574, #36889, #87520, #44444, #73350, #8462, #73803, #66248, #59136 ),
 .UNSPECIFIED., .F., .F.,
 ( 4, 2, 2, 2, 2, 2, 2, 2, 4 ),
 ( 0.000000000000000000, 0.0006105671578862054225, 0.001221134315772410845, 0.001831701473658616268, 0.002442268631544821690, 0.003052835789431026896, 0.003663402947317232535, 0.004273970105203438175, 0.004884537263089643380 ),
 .UNSPECIFIED. ) ;
#77774 = CARTESIAN_POINT ( 'NONE',  ( -105.3951433894272327, -295.4076314074646348, -242.0868078917496007 ) ) ;
#77775 = CARTESIAN_POINT ( 'NONE',  ( 31.10348871756850286, -276.9383875020517962, -242.0623013506351811 ) ) ;
#77776 = CARTESIAN_POINT ( 'NONE',  ( -37.12443831161420604, -296.2947748573664626, -196.3449554908045229 ) ) ;
#77777 = CARTESIAN_POINT ( 'NONE',  ( -78.15788021377544226, -296.8192619657740465, -331.4238908116442417 ) ) ;
#77778 = CARTESIAN_POINT ( 'NONE',  ( -10.36350882710902610, -295.7712887474172589, -338.5256488470991485 ) ) ;
#77779 = DIRECTION ( 'NONE',  ( 0.000000000000000000, 1.000000000000000000, 0.000000000000000000 ) ) ;
#77780 = CARTESIAN_POINT ( 'NONE',  ( -79.02216245182466992, -297.2043292419114096, -334.1512384923340164 ) ) ;
#77781 = CARTESIAN_POINT ( 'NONE',  ( -74.84261421891243060, -295.5543429858998365, -205.1576297279182484 ) ) ;
#77782 = CARTESIAN_POINT ( 'NONE',  ( -79.59637677992579086, -292.1159801070423327, -210.6464483809947694 ) ) ;
#77783 = CARTESIAN_POINT ( 'NONE',  ( -70.07229665704188903, -274.4347458730334779, -200.8279102821391575 ) ) ;
#77784 = CARTESIAN_POINT ( 'NONE',  ( -104.5935277712419378, -288.7264203095251673, -300.3628844216444804 ) ) ;
#77785 = FACE_OUTER_BOUND ( 'NONE', #81661, .T. ) ;
#77786 = CARTESIAN_POINT ( 'NONE',  ( -44.04365173154280910, -274.4620505115028095, -193.6618427816122505 ) ) ;
#77787 = CARTESIAN_POINT ( 'NONE',  ( -106.0056192413246805, -296.5527686162330383, -295.3563757769372842 ) ) ;
#77788 = CARTESIAN_POINT ( 'NONE',  ( 14.02138225634661417, -282.7481880881042571, -215.1514332593396546 ) ) ;
#77789 = CARTESIAN_POINT ( 'NONE',  ( 36.13084604322573767, -279.9672099008169539, -248.9814357734026942 ) ) ;
#77790 = CARTESIAN_POINT ( 'NONE',  ( -9.256782621126726340, -276.0430502786781517, -341.9470816572583090 ) ) ;
#77791 = CARTESIAN_POINT ( 'NONE',  ( 37.87485366581713464, -280.1072722916130147, -282.6453787612191491 ) ) ;
#77792 = CARTESIAN_POINT ( 'NONE',  ( 27.71294056767867175, -279.0503911189208566, -232.7058109421343488 ) ) ;
#77793 = CARTESIAN_POINT ( 'NONE',  ( 0.9343157785141926741, -273.1485294302837588, -207.5095346831271002 ) ) ;
#77794 = CARTESIAN_POINT ( 'NONE',  ( -96.36765988166499142, -281.1874927779224436, -224.0705127729911226 ) ) ;
#77795 = DIRECTION ( 'NONE',  ( -1.000000000000000000, 0.000000000000000000, 0.000000000000000000 ) ) ;
#77796 = CARTESIAN_POINT ( 'NONE',  ( 145.2857639756989272, -297.1570670221753971, -195.3611179825600175 ) ) ;
#77797 = CARTESIAN_POINT ( 'NONE',  ( -33.37747646669512847, -296.3410002000283612, -194.3756134808325555 ) ) ;
#77798 = CARTESIAN_POINT ( 'NONE',  ( -40.53689108001209718, -290.0322976746473387, -195.0607842498029356 ) ) ;
#77799 = CARTESIAN_POINT ( 'NONE',  ( -44.89704630020091969, -291.9591444340095450, -193.6797626336525298 ) ) ;
#77800 = CARTESIAN_POINT ( 'NONE',  ( -15.10710243309569023, -278.7651667265386664, -342.2184831078598677 ) ) ;
#77801 = CARTESIAN_POINT ( 'NONE',  ( 30.91656252957844586, -273.1427144208873870, -239.1579048482124961 ) ) ;
#77802 = CYLINDRICAL_SURFACE ( 'NONE', #74067, 4.000000000000003553 ) ;
#77803 = CARTESIAN_POINT ( 'NONE',  ( -4.762154311256177941, -284.5465915205719512, -338.5507551766988286 ) ) ;
#77804 = CARTESIAN_POINT ( 'NONE',  ( 210.1640492649783312, 37.84931640281050846, 12.09245862095555779 ) ) ;
#77805 = CARTESIAN_POINT ( 'NONE',  ( -6.484393732722012693, -284.4572015869234747, -201.9891716034530020 ) ) ;
#77806 = DIRECTION ( 'NONE',  ( -1.000000000000000000, 0.000000000000000000, -5.880589007913310608E-16 ) ) ;
#77807 = CARTESIAN_POINT ( 'NONE',  ( -28.86527586023586167, -293.7373616666228600, -343.3183801584384582 ) ) ;
#77808 = CARTESIAN_POINT ( 'NONE',  ( 34.91802828742577702, -285.4703453651744667, -253.2944313378754373 ) ) ;
#77809 = CARTESIAN_POINT ( 'NONE',  ( 157.4851178187871312, 14.99999999999999645, -9.000000000000000000 ) ) ;
#77810 = CARTESIAN_POINT ( 'NONE',  ( -12.36558361046928489, -292.7272644521042935, -341.1349493831488076 ) ) ;
#77811 = CARTESIAN_POINT ( 'NONE',  ( -80.52970607768872924, -283.9585459959500326, -207.3886543045527162 ) ) ;
#77812 = CARTESIAN_POINT ( 'NONE',  ( -62.60171197721145830, -281.3181546951419705, -200.9647420576450543 ) ) ;
#77813 = CARTESIAN_POINT ( 'NONE',  ( -26.69157130273216438, -287.3896862812131303, -194.4489248195647804 ) ) ;
#77814 = CARTESIAN_POINT ( 'NONE',  ( 27.42935362671035904, -280.3192388539116564, -310.1934510155680869 ) ) ;
#77815 = CARTESIAN_POINT ( 'NONE',  ( 6.926924441421244971, -286.6736382773327136, -212.2516743373252837 ) ) ;
#77816 = CARTESIAN_POINT ( 'NONE',  ( -70.01814581552230266, -281.0382979637683434, -204.4106375890868037 ) ) ;
#77817 = CARTESIAN_POINT ( 'NONE',  ( 13.43984192653332066, -281.5876297188358421, -217.6233023206523853 ) ) ;
#77818 = CARTESIAN_POINT ( 'NONE',  ( -69.12262362710320929, -287.6161643423073997, -202.0215156371622811 ) ) ;
#77819 = ORIENTED_EDGE ( 'NONE', *, *, #56462, .F. ) ;
#77820 = CARTESIAN_POINT ( 'NONE',  ( -114.3417001280813849, -272.5521521680024648, -270.3611179825603017 ) ) ;
#77821 = CARTESIAN_POINT ( 'NONE',  ( -71.91262985746872971, -291.4913419672820396, -336.5321709462367608 ) ) ;
#77822 = CARTESIAN_POINT ( 'NONE',  ( 169.2744399300530347, -11.64849832608277325, 10.00000000000000000 ) ) ;
#77823 = CARTESIAN_POINT ( 'NONE',  ( 13.84574458161073096, -290.9090924074130839, -334.4957818155094174 ) ) ;
#77824 = EDGE_LOOP ( 'NONE', ( #74346, #40576, #21762, #20564, #7504, #24767 ) ) ;
#77825 = CARTESIAN_POINT ( 'NONE',  ( 1.493147996876710737, -272.5697584191618148, -206.0036553438961846 ) ) ;
#77826 = CARTESIAN_POINT ( 'NONE',  ( -96.79618238036371736, -294.3065505336375054, -318.0431316831548543 ) ) ;
#77827 = CARTESIAN_POINT ( 'NONE',  ( -105.5082903411829562, -272.2547354049543173, -243.8168174096828977 ) ) ;
#77828 = CARTESIAN_POINT ( 'NONE',  ( 10.58068572582067901, -289.8964943967174008, -326.4121095182097179 ) ) ;
#77829 = CIRCLE ( 'NONE', #29436, 11.40608546931776779 ) ;
#77831 = EDGE_CURVE ( 'NONE', #12908, #37793, #46933, .T. ) ;
#77830 = CARTESIAN_POINT ( 'NONE',  ( 32.93175798253300712, -283.0062388817232204, -246.9701215346832441 ) ) ;
#77832 = CARTESIAN_POINT ( 'NONE',  ( -95.92750843724100207, -291.3119246698091729, -319.4355536755416551 ) ) ;
#77833 = CARTESIAN_POINT ( 'NONE',  ( -95.07508638284664926, -291.1843557862740113, -320.5622572649332369 ) ) ;
#77834 = CARTESIAN_POINT ( 'NONE',  ( -42.84564067182729730, -287.9828744997710714, -195.5503704792633357 ) ) ;
#77835 = CARTESIAN_POINT ( 'NONE',  ( -93.07521974658013164, -279.4458976767204490, -217.1551422781808469 ) ) ;
#77836 = CARTESIAN_POINT ( 'NONE',  ( 5.771916914311491453, -292.5531352304536767, -332.4774978167889685 ) ) ;
#77837 = CARTESIAN_POINT ( 'NONE',  ( 37.19127262340634843, -281.6274672583128336, -289.6959564187018259 ) ) ;
#77838 = CARTESIAN_POINT ( 'NONE',  ( -6.029159428263385578, -276.3285712387122430, -203.0529440475563092 ) ) ;
#77839 = CARTESIAN_POINT ( 'NONE',  ( -37.37352853689063181, -276.5519495502701375, -200.3611179825600459 ) ) ;
#77840 = CARTESIAN_POINT ( 'NONE',  ( -1.959709683981272210, -274.8299380774016640, -337.6075957189154906 ) ) ;
#77841 = DIRECTION ( 'NONE',  ( 1.000000000000000000, -0.000000000000000000, 0.000000000000000000 ) ) ;
#77842 = CARTESIAN_POINT ( 'NONE',  ( 35.74908926908865681, -281.0364354699721616, -268.5883340753606490 ) ) ;
#77843 = CARTESIAN_POINT ( 'NONE',  ( -99.31941938901326239, -279.1565484298548085, -315.4030906218728774 ) ) ;
#77844 = CARTESIAN_POINT ( 'NONE',  ( -67.27358702228808340, -274.9664237572079628, -203.2256083818994057 ) ) ;
#77845 = CARTESIAN_POINT ( 'NONE',  ( -113.2529073734491902, -283.7584975083096310, -258.5956698820859856 ) ) ;
#77846 = CARTESIAN_POINT ( 'NONE',  ( -77.82794896661859241, -293.2602204306523390, -208.4027636859447910 ) ) ;
#77847 = CARTESIAN_POINT ( 'NONE',  ( -98.93259805941819707, -274.7549802943333361, -225.4071067310807166 ) ) ;
#77848 = CARTESIAN_POINT ( 'NONE',  ( -102.3091655580507506, -274.3992959762760506, -229.9565797758355359 ) ) ;
#77849 = CARTESIAN_POINT ( 'NONE',  ( 159.4851178187871312, 3.000000000000000000, 9.000000000000001776 ) ) ;
#77850 = CARTESIAN_POINT ( 'NONE',  ( -13.78740676530620846, -276.5712360821904099, -339.5098068145924231 ) ) ;
#77851 = CARTESIAN_POINT ( 'NONE',  ( -109.6127013934152927, -298.8030332293877791, -250.8969695909260622 ) ) ;
#77852 = CARTESIAN_POINT ( 'NONE',  ( -94.64290160504012306, -283.2188028014856513, -222.2300392587783335 ) ) ;
#77853 = CARTESIAN_POINT ( 'NONE',  ( -7.194570306159838502, -292.1036285232881937, -199.5167577954833860 ) ) ;
#77854 = CARTESIAN_POINT ( 'NONE',  ( 34.47356654315331781, -273.8360046415699003, -290.7650038886256425 ) ) ;
#77855 = CARTESIAN_POINT ( 'NONE',  ( -36.07944315171685901, -290.6367294326320234, -346.5636392002280104 ) ) ;
#77856 = CARTESIAN_POINT ( 'NONE',  ( -107.2924645115570712, -289.7624593109689499, -248.3844847533809173 ) ) ;
#77857 = VERTEX_POINT ( 'NONE', #45629 ) ;
#77858 = CARTESIAN_POINT ( 'NONE',  ( 27.56153710021769498, -291.5941862183674402, -229.9352296556147621 ) ) ;
#77859 = CARTESIAN_POINT ( 'NONE',  ( -108.6842922323005638, -290.0128686932682172, -285.9859576085128197 ) ) ;
#77860 = ORIENTED_EDGE ( 'NONE', *, *, #1655, .T. ) ;
#77861 = CARTESIAN_POINT ( 'NONE',  ( 28.64480375442017035, -289.1430128325756073, -309.4414687295179647 ) ) ;
#77862 = CARTESIAN_POINT ( 'NONE',  ( -110.3724700157753205, -278.9177369472043324, -267.9117865372344909 ) ) ;
#77863 = CARTESIAN_POINT ( 'NONE',  ( -68.11481489992183924, -294.3672165408218575, -340.6071706671751258 ) ) ;
#77864 = CARTESIAN_POINT ( 'NONE',  ( -83.81499226946739611, -284.3225493125258936, -331.6941910696224340 ) ) ;
#77865 = CARTESIAN_POINT ( 'NONE',  ( -114.1869479316844291, -284.8183872267521792, -275.7205382013739836 ) ) ;
#77866 = CARTESIAN_POINT ( 'NONE',  ( -40.23094732082699920, -283.4227500178218406, -343.3250798918173814 ) ) ;
#77867 = CARTESIAN_POINT ( 'NONE',  ( 45.21095933465400662, 12.48609948641568401, -332.0833974251048630 ) ) ;
#77868 = EDGE_CURVE ( 'NONE', #33195, #31059, #42432, .T. ) ;
#77869 = CARTESIAN_POINT ( 'NONE',  ( -32.31571139608886511, -123.7737035626091142, -363.2393823568430662 ) ) ;
#77870 = CARTESIAN_POINT ( 'NONE',  ( 102.0852645817304420, 115.1042933526224346, -279.6109006776878232 ) ) ;
#77871 = CARTESIAN_POINT ( 'NONE',  ( 33.05043141068819068, -275.0128741221709561, -290.3455852157211439 ) ) ;
#77872 = CARTESIAN_POINT ( 'NONE',  ( -3.951671187673817975, -273.4236201873168284, -205.0834662887545505 ) ) ;
#77873 = CARTESIAN_POINT ( 'NONE',  ( 4.188801008173478557, -294.0164634293062136, -335.1906872579032779 ) ) ;
#77874 = CARTESIAN_POINT ( 'NONE',  ( 154.3500357470443021, 204.3678965669933802, -214.6393225715670781 ) ) ;
#77875 = ADVANCED_FACE ( 'NONE', ( #60350 ), #54156, .F. ) ;
#77876 = CARTESIAN_POINT ( 'NONE',  ( 36.75691449646658526, -274.4768550205615156, -289.4056338577922247 ) ) ;
#77877 = CARTESIAN_POINT ( 'NONE',  ( -37.85442852042710626, -299.9060784993138782, -196.1276848580625938 ) ) ;
#77878 = ADVANCED_FACE ( 'NONE', ( #2582 ), #39359, .T. ) ;
#77879 = CARTESIAN_POINT ( 'NONE',  ( -90.04807432586440541, -292.3649870685533187, -219.4075686216673660 ) ) ;
#77880 = ORIENTED_EDGE ( 'NONE', *, *, #48014, .F. ) ;
#77881 = CARTESIAN_POINT ( 'NONE',  ( -93.49883429147621428, -298.2097262211927386, -217.9462348266160632 ) ) ;
#77882 =( BOUNDED_SURFACE ( )  B_SPLINE_SURFACE ( 3, 2, ( 
 ( #76131, #76601, #61478 ),
 ( #41036, #39642, #69034 ),
 ( #10781, #83216, #69491 ),
 ( #68566, #69964, #91245 ),
 ( #3702, #32587, #18361 ),
 ( #61926, #90308, #33983 ),
 ( #48631, #17903, #47221 ),
 ( #40577, #46757, #19300 ),
 ( #4164, #33036, #47702 ),
 ( #89852, #25013, #90763 ) ),
 .UNSPECIFIED., .F., .F., .F. ) 
 B_SPLINE_SURFACE_WITH_KNOTS ( ( 4, 2, 2, 2, 4 ),
 ( 3, 3 ),
 ( 6.806784082777886269, 7.068583470577035399, 7.330382858376184529, 7.592182246175333660, 7.853981633974482790 ),
 ( 0.000000000000000000, 1.000000000000000000 ),
 .UNSPECIFIED. ) 
 GEOMETRIC_REPRESENTATION_ITEM ( )  RATIONAL_B_SPLINE_SURFACE ( (
 ( 1.000000000000000000, 0.7905694150420951027, 1.000000000000000000),
 ( 1.000000000000000000, 0.8144940228947546990, 1.000000000000000000),
 ( 1.000000000000000000, 0.8408337462327619694, 1.000000000000000000),
 ( 1.000000000000000000, 0.8912170613361163340, 1.000000000000000000),
 ( 1.000000000000000000, 0.9152160855729576383, 1.000000000000000000),
 ( 1.000000000000000000, 0.9556126078140139146, 1.000000000000000000),
 ( 1.000000000000000000, 0.9720148405105164535, 1.000000000000000000),
 ( 1.000000000000000000, 0.9942062568700493763, 1.000000000000000000),
 ( 1.000000000000000000, 1.000000000000000000, 1.000000000000000000),
 ( 1.000000000000000000, 1.000000000000000000, 1.000000000000000000) ) ) 
 REPRESENTATION_ITEM ( '' )  SURFACE ( )  );
#77883 = CARTESIAN_POINT ( 'NONE',  ( 34.62691000563234667, -287.8747988460855822, -257.4858968189267330 ) ) ;
#77884 = CARTESIAN_POINT ( 'NONE',  ( -110.1893635948897838, -297.0465562167128155, -294.8024098420250994 ) ) ;
#77885 = CARTESIAN_POINT ( 'NONE',  ( -27.74928510507582757, -295.4259222851308664, -346.7525137249320437 ) ) ;
#77886 = CARTESIAN_POINT ( 'NONE',  ( 30.82763263933218312, -293.3700666634761092, -244.2470973320261862 ) ) ;
#77887 = VERTEX_POINT ( 'NONE', #23878 ) ;
#77888 =( BOUNDED_CURVE ( )  B_SPLINE_CURVE ( 3, ( #13063, #33401, #48534, #84519 ),
 .UNSPECIFIED., .F., .F. ) 
 B_SPLINE_CURVE_WITH_KNOTS ( ( 4, 4 ),
 ( 4.278565243615663150, 4.712388980384691450 ),
 .UNSPECIFIED. ) 
 CURVE ( )  GEOMETRIC_REPRESENTATION_ITEM ( )  RATIONAL_B_SPLINE_CURVE ( ( 1.000000000000000000, 0.9843778111405747655, 0.9843778111405747655, 1.000000000000000000 ) ) 
 REPRESENTATION_ITEM ( '' )  );
#77889 = AXIS2_PLACEMENT_3D ( 'NONE', #25051, #24103, #16541 ) ;
#77890 = CARTESIAN_POINT ( 'NONE',  ( 19.74860421915299824, -278.1540587828893649, -319.8782978123292651 ) ) ;
#77891 = ORIENTED_EDGE ( 'NONE', *, *, #14175, .F. ) ;
#77892 = CARTESIAN_POINT ( 'NONE',  ( -28.22606646958156773, -279.6724005652288270, -193.9109903708342131 ) ) ;
#77893 = CARTESIAN_POINT ( 'NONE',  ( 32.28177383408095125, -276.1910163916273859, -247.4828649506638669 ) ) ;
#77894 = CARTESIAN_POINT ( 'NONE',  ( 29.05108971108531435, -276.8255565761799062, -233.2939253991620205 ) ) ;
#77895 = CARTESIAN_POINT ( 'NONE',  ( -35.77161143971162716, -275.0526921226901322, -345.7128069339277658 ) ) ;
#77896 = CARTESIAN_POINT ( 'NONE',  ( -55.32675472505136582, -298.4661548596025114, -199.4537364939857582 ) ) ;
#77897 = CARTESIAN_POINT ( 'NONE',  ( -70.00176890781557404, -294.0658395143611301, -336.3057525351154027 ) ) ;
#77898 = CARTESIAN_POINT ( 'NONE',  ( 200.2296996224750103, 68.12454877777268791, 0.000000000000000000 ) ) ;
#77899 = CARTESIAN_POINT ( 'NONE',  ( -86.76999003683769729, -279.8786128753487787, -211.3309135519273241 ) ) ;
#77900 = CARTESIAN_POINT ( 'NONE',  ( 20.83820548198987765, -276.3384477307179168, -314.4530513460756538 ) ) ;
#77901 = AXIS2_PLACEMENT_3D ( 'NONE', #68170, #33113, #68642 ) ;
#77902 = CARTESIAN_POINT ( 'NONE',  ( -15.53786412000536998, -285.0132759303832586, -196.9719709206454752 ) ) ;
#77903 = CARTESIAN_POINT ( 'NONE',  ( -33.47854310738762962, -300.1005598813350161, -195.1931292090783359 ) ) ;
#77904 = CARTESIAN_POINT ( 'NONE',  ( 212.2107582607290510, 32.98517505407394168, 14.69807322781335657 ) ) ;
#77906 = EDGE_CURVE ( 'NONE', #20412, #64509, #4657, .T. ) ;
#77905 = CARTESIAN_POINT ( 'NONE',  ( 35.28327639339224930, -286.8657237183146549, -279.2050148687105207 ) ) ;
#77907 = AXIS2_PLACEMENT_3D ( 'NONE', #57173, #22101, #93583 ) ;
#77908 = CARTESIAN_POINT ( 'NONE',  ( -86.13564841907148661, -277.6042543601321881, -214.7093020070257126 ) ) ;
#77910 = CARTESIAN_POINT ( 'NONE',  ( -107.5396999278674173, -282.3069433636513281, -295.2848038767965022 ) ) ;
#77909 = CARTESIAN_POINT ( 'NONE',  ( -103.8950534298601553, -277.5491990153288953, -238.8403564528508127 ) ) ;
#77911 = CARTESIAN_POINT ( 'NONE',  ( -33.28594586776748088, -288.1032519430545449, -195.4204966776122205 ) ) ;
#77912 = CARTESIAN_POINT ( 'NONE',  ( -85.35345359285548739, -278.9378994995622065, -325.9442114815389004 ) ) ;
#77913 = CARTESIAN_POINT ( 'NONE',  ( 203.5977283565847813, 62.01285785379744198, -7.000000000000000888 ) ) ;
#77914 = CARTESIAN_POINT ( 'NONE',  ( -95.05656618886520448, -293.2136646671236235, -222.4455957921904314 ) ) ;
#77915 = CARTESIAN_POINT ( 'NONE',  ( -25.94437624670307230, -275.1487687691954420, -345.4881771570215960 ) ) ;
#77916 = CARTESIAN_POINT ( 'NONE',  ( -40.50188109374197154, -277.7443176950906718, -343.4071943015082411 ) ) ;
#77917 = CARTESIAN_POINT ( 'NONE',  ( 36.44992186715253268, -283.3689571388582067, -256.0494111413789255 ) ) ;
#77918 = CARTESIAN_POINT ( 'NONE',  ( -83.63170945779074827, -296.0521521680024080, -521.1711561948568487 ) ) ;
#77919 = CARTESIAN_POINT ( 'NONE',  ( -4.928195225406174274, -290.5488790721537384, -338.6298449423319994 ) ) ;
#77920 = CARTESIAN_POINT ( 'NONE',  ( -94.33683259953144784, -295.2274073608895719, -221.5918554959565938 ) ) ;
#77921 = CARTESIAN_POINT ( 'NONE',  ( 207.8905253643919195, 30.23467176727723782, 14.36943405361669157 ) ) ;
#77922 = CARTESIAN_POINT ( 'NONE',  ( 19.39014416156286558, -273.5793335152262671, -223.6413007421882924 ) ) ;
#77923 = CARTESIAN_POINT ( 'NONE',  ( -19.75697806506245158, -290.4200668121802664, -198.1855433051566422 ) ) ;
#77924 = LINE ( 'NONE', #54248, #89514 ) ;
#77925 = CARTESIAN_POINT ( 'NONE',  ( 188.7149167944524493, 8.542400036368780647, 10.00000000000000000 ) ) ;
#77926 = CARTESIAN_POINT ( 'NONE',  ( -95.12312225120990661, -289.7113846199916338, -220.5012585941549901 ) ) ;
#77927 = CARTESIAN_POINT ( 'NONE',  ( 37.56182725202084072, -285.6290270329834016, -257.5002479405208646 ) ) ;
#77928 = CARTESIAN_POINT ( 'NONE',  ( -54.91449638041446946, -287.2471936631757785, -198.8481140307592341 ) ) ;
#77929 = CARTESIAN_POINT ( 'NONE',  ( -65.16407879324741259, -286.4820148051673527, -202.6424477915757052 ) ) ;
#77930 = CARTESIAN_POINT ( 'NONE',  ( -41.97849182923987854, -293.9738672472051917, -195.1487056649911551 ) ) ;
#77931 = CARTESIAN_POINT ( 'NONE',  ( 36.23835796270876131, -273.4123459145749848, -253.1207721556502577 ) ) ;
#77932 = CARTESIAN_POINT ( 'NONE',  ( 29.92699025259534906, -275.3989262285777500, -232.8260239804113496 ) ) ;
#77933 = CARTESIAN_POINT ( 'NONE',  ( -112.9494946530976023, -288.6214560481333251, -271.1881267596637031 ) ) ;
#77934 = CARTESIAN_POINT ( 'NONE',  ( -20.12610442838468217, -276.8369733285863390, -345.4666413788748969 ) ) ;
#77935 = CARTESIAN_POINT ( 'NONE',  ( -107.5252555960994840, -298.1991143452128767, -295.9317583000727154 ) ) ;
#77936 = DIRECTION ( 'NONE',  ( -0.000000000000000000, -0.000000000000000000, 1.000000000000000000 ) ) ;
#77937 = CARTESIAN_POINT ( 'NONE',  ( -108.5753225508914852, -282.9998984035043463, -288.4446606620529110 ) ) ;
#77938 = CARTESIAN_POINT ( 'NONE',  ( -61.38180560496080318, -277.7399057772449851, -199.2635913898405704 ) ) ;
#77939 = CARTESIAN_POINT ( 'NONE',  ( 200.2349812190172713, 66.43136063442170780, 7.741079165001067963 ) ) ;
#77940 = CARTESIAN_POINT ( 'NONE',  ( -32.70521247465042336, -272.5894392137715272, -194.1824063602071533 ) ) ;
#77941 = CARTESIAN_POINT ( 'NONE',  ( -51.30847225048231053, -276.5840573300928895, -342.1164100823701801 ) ) ;
#77942 = CARTESIAN_POINT ( 'NONE',  ( -5.221979995643446060, -296.1416882902084353, -336.7002557253854889 ) ) ;
#77943 = CARTESIAN_POINT ( 'NONE',  ( -8.962664155152358703, -279.3351107549164567, -199.1142034729891179 ) ) ;
#77944 = CARTESIAN_POINT ( 'NONE',  ( -95.78488004436138681, -296.8751655969617218, -314.5156954167891854 ) ) ;
#77945 = CARTESIAN_POINT ( 'NONE',  ( -86.06827166205630419, -297.0268035059925751, -329.3443316791561983 ) ) ;
#77946 = CARTESIAN_POINT ( 'NONE',  ( -37.14748037964942284, -297.8879779239914569, -197.3582748454228408 ) ) ;
#77947 = CARTESIAN_POINT ( 'NONE',  ( -101.4335920447371109, -293.0744354842524331, -231.4094808189903176 ) ) ;
#77948 = ADVANCED_FACE ( 'NONE', ( #17718 ), #38551, .F. ) ;
#77949 = CARTESIAN_POINT ( 'NONE',  ( -69.79477315177382479, -285.8032460596815554, -200.5198374910926020 ) ) ;
#77950 = CARTESIAN_POINT ( 'NONE',  ( 7.490776091255906266, -274.5878949043317334, -331.5026876122603881 ) ) ;
#77951 = CARTESIAN_POINT ( 'NONE',  ( 37.14387511131583608, -287.6297729102961398, -289.8777541112779659 ) ) ;
#77952 = CARTESIAN_POINT ( 'NONE',  ( -90.66585033668808080, -281.2720822623585377, -218.0539240777975181 ) ) ;
#77953 = CARTESIAN_POINT ( 'NONE',  ( -27.79404683961005418, -285.2351210192896929, -197.7508517356553739 ) ) ;
#77954 = CARTESIAN_POINT ( 'NONE',  ( -98.26104027413573760, -287.9564642711482634, -314.1305269378204343 ) ) ;
#77955 = CARTESIAN_POINT ( 'NONE',  ( -89.67076919512652466, -242.4121354169174367, -340.4712336312485377 ) ) ;
#77956 = CARTESIAN_POINT ( 'NONE',  ( 33.44974758320255859, -286.8208786887635711, -252.2396500136737245 ) ) ;
#77957 = DIRECTION ( 'NONE',  ( 0.000000000000000000, 0.000000000000000000, 1.000000000000000000 ) ) ;
#77958 = CARTESIAN_POINT ( 'NONE',  ( -33.05985201258903317, -283.9407356820760242, -347.0194082359944332 ) ) ;
#77959 = CARTESIAN_POINT ( 'NONE',  ( -96.88010299293385685, -289.1794479861563900, -224.4577660744706691 ) ) ;
#77960 = CARTESIAN_POINT ( 'NONE',  ( -44.86202929437367715, -291.0180442021259637, -193.9129069774049299 ) ) ;
#77961 = CARTESIAN_POINT ( 'NONE',  ( -109.7954413275817416, -280.4541711175155001, -246.5948669354799563 ) ) ;
#77962 = CARTESIAN_POINT ( 'NONE',  ( -97.32078551127240473, -280.5069482343954519, -222.8657751399411779 ) ) ;
#77963 = CARTESIAN_POINT ( 'NONE',  ( 9.278169557086753727, -280.5465787402499700, -214.1206034837695711 ) ) ;
#77964 = CARTESIAN_POINT ( 'NONE',  ( 32.98510210217236249, -277.2140611195449651, -244.3007738723994180 ) ) ;
#77965 = CARTESIAN_POINT ( 'NONE',  ( -77.08222869163832058, -295.5688350394901818, -336.3753312726047966 ) ) ;
#77966 = CARTESIAN_POINT ( 'NONE',  ( -106.6494327325996778, -288.2078448062795246, -298.2179161902017768 ) ) ;
#77967 = CONICAL_SURFACE ( 'NONE', #11506, 4.025000000000000355, 0.7853981633973095011 ) ;
#77968 = CARTESIAN_POINT ( 'NONE',  ( -80.34717540523259061, -294.5707566997787126, -329.7307665325215567 ) ) ;
#77969 = EDGE_LOOP ( 'NONE', ( #7088, #62606, #39290, #56302 ) ) ;
#77970 = ORIENTED_EDGE ( 'NONE', *, *, #46209, .T. ) ;
#77971 = CARTESIAN_POINT ( 'NONE',  ( -65.84489675661505714, -285.3480853791600111, -339.1418494308663298 ) ) ;
#77972 = CARTESIAN_POINT ( 'NONE',  ( -110.2630065774707049, -296.1685290390551586, -274.1782572788544030 ) ) ;
#77973 = CARTESIAN_POINT ( 'NONE',  ( -42.04878047327095913, -293.0737918267600435, -193.8148188907349549 ) ) ;
#77974 = CARTESIAN_POINT ( 'NONE',  ( -45.64281653973429087, -283.8114164703379743, -343.0412688852480301 ) ) ;
#77975 = EDGE_CURVE ( 'NONE', #75154, #45901, #21296, .T. ) ;
#77976 = CARTESIAN_POINT ( 'NONE',  ( 31.04612929369649166, -274.1604457384432294, -235.4910018475604829 ) ) ;
#77977 = CARTESIAN_POINT ( 'NONE',  ( -44.89530065077337184, -292.6104526181504184, -193.7820876729325619 ) ) ;
#77978 = CARTESIAN_POINT ( 'NONE',  ( -92.99603803810333602, -283.4038404328582033, -218.8751118250499985 ) ) ;
#77979 = CARTESIAN_POINT ( 'NONE',  ( -92.79979941882028527, -291.6171577397007582, -216.8985433687288946 ) ) ;
#77980 = CARTESIAN_POINT ( 'NONE',  ( 35.65132491270625792, -287.9302143546821640, -273.7565812421768214 ) ) ;
#77981 = DIRECTION ( 'NONE',  ( 0.000000000000000000, 0.000000000000000000, 1.000000000000000000 ) ) ;
#77982 = CARTESIAN_POINT ( 'NONE',  ( 154.4030696693785956, 128.9756020784251120, -12.16842021443607713 ) ) ;
#77983 = CARTESIAN_POINT ( 'NONE',  ( 45.23250845692812305, 11.08492981906800701, -328.3308289300945830 ) ) ;
#77984 = CARTESIAN_POINT ( 'NONE',  ( 17.34304175893838007, -283.8092021542565817, -323.6558720886995957 ) ) ;
#77985 = CARTESIAN_POINT ( 'NONE',  ( 10.64812456238590777, -284.1952119285918457, -210.2361428286349110 ) ) ;
#77986 = VERTEX_POINT ( 'NONE', #10594 ) ;
#77987 = CARTESIAN_POINT ( 'NONE',  ( -34.28674091711881289, -279.0117505499570711, -197.1030895341135931 ) ) ;
#77988 = CARTESIAN_POINT ( 'NONE',  ( 27.62870382355426102, -275.7612537966296600, -311.7468852477241512 ) ) ;
#77989 = CARTESIAN_POINT ( 'NONE',  ( -111.0885591932006520, -280.3878400200118222, -283.1421908959335383 ) ) ;
#77990 = CARTESIAN_POINT ( 'NONE',  ( 155.0569925984352437, 204.5026487299929272, -215.2223648592982101 ) ) ;
#77991 = ADVANCED_FACE ( 'NONE', ( #39455 ), #74201, .T. ) ;
#77992 = CARTESIAN_POINT ( 'NONE',  ( 5.866126571937878786, -279.2002729723147354, -207.3397723647147188 ) ) ;
#77993 = CARTESIAN_POINT ( 'NONE',  ( -96.23967892941550417, -283.2044057919530360, -224.4832575617479051 ) ) ;
#77994 = CARTESIAN_POINT ( 'NONE',  ( -112.9328559201644566, -298.2141660918381945, -278.1039326154722175 ) ) ;
#77995 = CARTESIAN_POINT ( 'NONE',  ( 28.79155699555532166, -293.6239379426692153, -239.1872575319255532 ) ) ;
#77996 = ORIENTED_EDGE ( 'NONE', *, *, #49490, .F. ) ;
#77997 = CARTESIAN_POINT ( 'NONE',  ( -110.6157490441761411, -289.1544942125172497, -276.6555871042371564 ) ) ;
#77998 = CARTESIAN_POINT ( 'NONE',  ( 31.15573365154443408, -275.7528545977390309, -235.4123790656805681 ) ) ;
#77999 = CARTESIAN_POINT ( 'NONE',  ( -69.49096092639894096, -273.6167721611693082, -204.8216258413955302 ) ) ;
#78000 = EDGE_LOOP ( 'NONE', ( #59245, #85997 ) ) ;
#78001 = CARTESIAN_POINT ( 'NONE',  ( 196.6877655503061533, 293.9636489450776367, -59.00000000000003553 ) ) ;
#78002 = DIRECTION ( 'NONE',  ( -1.000000000000000000, -0.000000000000000000, -0.000000000000000000 ) ) ;
#78003 = DIRECTION ( 'NONE',  ( 0.000000000000000000, 0.000000000000000000, 1.000000000000000000 ) ) ;
#78004 = CARTESIAN_POINT ( 'NONE',  ( 35.73836176923398966, -282.7159446937331495, -276.7645155475801744 ) ) ;
#78005 = CARTESIAN_POINT ( 'NONE',  ( 0.8450743835883158805, -282.3139502053393812, -204.6068958529008057 ) ) ;
#78006 = CARTESIAN_POINT ( 'NONE',  ( -66.66475680542281168, -282.5046936961529696, -337.4833533606856122 ) ) ;
#78007 = CARTESIAN_POINT ( 'NONE',  ( 16.13297601197039555, -282.6807190127457261, -218.7966961930482057 ) ) ;
#78008 = CARTESIAN_POINT ( 'NONE',  ( 5.787031647423192204, -274.9358990430971517, -330.1787889949113719 ) ) ;
#78009 = CYLINDRICAL_SURFACE ( 'NONE', #85087, 2.395975569037589459 ) ;
#78010 = DIRECTION ( 'NONE',  ( -0.9693563597868444237, -0.2456588035076248677, -0.000000000000000000 ) ) ;
#78011 = CARTESIAN_POINT ( 'NONE',  ( -38.53218329042907442, -277.8695521315996189, -347.1904194959677739 ) ) ;
#78012 = ORIENTED_EDGE ( 'NONE', *, *, #34464, .T. ) ;
#78013 = VERTEX_POINT ( 'NONE', #77822 ) ;
#78014 = DIRECTION ( 'NONE',  ( -0.000000000000000000, -0.000000000000000000, -1.000000000000000000 ) ) ;
#78015 = CARTESIAN_POINT ( 'NONE',  ( -98.43975039623825296, -285.9334007008319531, -314.5553682605402628 ) ) ;
#78016 = CARTESIAN_POINT ( 'NONE',  ( 31.68901697243846272, -293.0728598703734633, -294.7482962532113788 ) ) ;
#78017 = CARTESIAN_POINT ( 'NONE',  ( 37.40337367037867722, -287.1276814807554842, -288.4856632237528515 ) ) ;
#78018 = CARTESIAN_POINT ( 'NONE',  ( -82.07344192543625638, -283.6724660893178225, -211.3946420260229786 ) ) ;
#78020 = CARTESIAN_POINT ( 'NONE',  ( -61.60811762394020974, -287.6116653174140083, -340.2833247160724568 ) ) ;
#78019 = CARTESIAN_POINT ( 'NONE',  ( -110.6844972590510565, -283.0481292776624400, -276.3785115289605301 ) ) ;
#78021 = CARTESIAN_POINT ( 'NONE',  ( -36.17189450360240954, -284.2422398756755797, -343.7488694187027818 ) ) ;
#78022 = CARTESIAN_POINT ( 'NONE',  ( 8.313569684162438023, -272.6768079095342614, -210.8582022216696430 ) ) ;
#78023 = CARTESIAN_POINT ( 'NONE',  ( -43.58023711589384419, -284.3745917571832251, -194.3642154339628405 ) ) ;
#78024 = CARTESIAN_POINT ( 'NONE',  ( -51.45003256453077967, -299.8720352404391178, -196.6471005666851397 ) ) ;
#78025 = CARTESIAN_POINT ( 'NONE',  ( -108.2393916541987267, -282.8746962262992497, -245.3902196875901325 ) ) ;
#78026 = CARTESIAN_POINT ( 'NONE',  ( -24.84799789795610891, -281.1567151623135032, -198.1993839950561380 ) ) ;
#78027 = CARTESIAN_POINT ( 'NONE',  ( 28.76282144291930010, -290.0276912174375070, -306.2502114654001844 ) ) ;
#78028 = LINE ( 'NONE', #56729, #15702 ) ;
#78029 = FACE_OUTER_BOUND ( 'NONE', #56104, .T. ) ;
#78030 = CARTESIAN_POINT ( 'NONE',  ( 5.812028816583048041, -296.3928250819216714, -332.4496372304887473 ) ) ;
#78031 = AXIS2_PLACEMENT_3D ( 'NONE', #48597, #63789, #50003 ) ;
#78032 = CARTESIAN_POINT ( 'NONE',  ( -104.9445066263934336, -276.1229172585535139, -302.9599979713765947 ) ) ;
#78033 = CARTESIAN_POINT ( 'NONE',  ( -88.53427863837782752, -290.5526114677807072, -213.0594711866723969 ) ) ;
#78034 = CARTESIAN_POINT ( 'NONE',  ( -47.92771635643258321, -293.5887522324441079, -343.4497788984960494 ) ) ;
#78035 = CARTESIAN_POINT ( 'NONE',  ( -71.15374545444680621, -278.2809459688517109, -205.0936680473996603 ) ) ;
#78036 = CARTESIAN_POINT ( 'NONE',  ( -111.6239364621605574, -270.7041710373114825, -264.7816375358765981 ) ) ;
#78037 = CARTESIAN_POINT ( 'NONE',  ( 34.55348230529268960, -295.0678418764408093, -285.6637969265142942 ) ) ;
#78038 = CARTESIAN_POINT ( 'NONE',  ( -54.49178911615188525, -288.3376638359845288, -195.3683826091709363 ) ) ;
#78039 = CARTESIAN_POINT ( 'NONE',  ( -89.12347088402501072, -295.8198303883943936, -214.2417575089994841 ) ) ;
#78040 = CARTESIAN_POINT ( 'NONE',  ( 18.44349158545691125, -289.8340234761826082, -318.7538335018079465 ) ) ;
#78041 = CARTESIAN_POINT ( 'NONE',  ( -37.76657183856354294, -290.2867648098452378, -194.3756358058248566 ) ) ;
#78042 = CARTESIAN_POINT ( 'NONE',  ( -96.22900833525611120, -291.3626350569492729, -314.5144402165781798 ) ) ;
#78043 = CARTESIAN_POINT ( 'NONE',  ( 159.4851178187871312, 0.000000000000000000, 9.000000000000001776 ) ) ;
#78044 = CARTESIAN_POINT ( 'NONE',  ( -55.06133827327901287, -292.6212219061191036, -199.3779076407261641 ) ) ;
#78045 = DIRECTION ( 'NONE',  ( 1.000000000000000000, 0.000000000000000000, 0.000000000000000000 ) ) ;
#78046 = CARTESIAN_POINT ( 'NONE',  ( -101.3606066848042104, -292.3141433312226809, -228.1994284328014544 ) ) ;
#78048 = CARTESIAN_POINT ( 'NONE',  ( -3.636257387683622166, -292.5100513929653516, -205.6081788239876857 ) ) ;
#78047 = CARTESIAN_POINT ( 'NONE',  ( 32.04141589397940493, -279.9561610777213332, -299.8947781878780461 ) ) ;
#78049 = CARTESIAN_POINT ( 'NONE',  ( 38.87126650710599307, -281.6894854985901588, -281.3421797100900221 ) ) ;
#78050 = CARTESIAN_POINT ( 'NONE',  ( 29.27041051114071024, -280.7170019708249242, -231.7791143067110511 ) ) ;
#78051 = CARTESIAN_POINT ( 'NONE',  ( -61.87961827879398413, -287.3716847475225791, -341.0570796647887732 ) ) ;
#78052 = CARTESIAN_POINT ( 'NONE',  ( 22.33584591161826438, -279.0827678749289475, -226.1870705725358448 ) ) ;
#78053 = CARTESIAN_POINT ( 'NONE',  ( -104.8670900613770982, -282.9819557755931214, -237.7218416429464014 ) ) ;
#78054 = CARTESIAN_POINT ( 'NONE',  ( 21.44901790306999700, -279.3722026598804860, -221.7158794859921045 ) ) ;
#78055 = CARTESIAN_POINT ( 'NONE',  ( 26.88642267267063346, -285.9197277107601280, -228.4535917965323506 ) ) ;
#78056 = CARTESIAN_POINT ( 'NONE',  ( 195.8217498488526189, 40.98913131717844038, 14.50814483734951921 ) ) ;
#78057 = CARTESIAN_POINT ( 'NONE',  ( 13.43902604296970260, -294.3775230667600340, -216.8096636284770682 ) ) ;
#78058 = CARTESIAN_POINT ( 'NONE',  ( 26.42873537441102982, -276.4195853971948509, -228.2667258571102309 ) ) ;
#78059 = CARTESIAN_POINT ( 'NONE',  ( -94.47223206747702307, -277.5766073369651394, -315.8584469437942630 ) ) ;
#78060 = CARTESIAN_POINT ( 'NONE',  ( -101.6851289270089183, -291.2759151002916269, -227.9697699020849768 ) ) ;
#78061 = CARTESIAN_POINT ( 'NONE',  ( -52.65022701274669004, -281.3264997077161524, -344.4075889059903943 ) ) ;
#78062 = CARTESIAN_POINT ( 'NONE',  ( -110.6028678928897335, -289.6361073270563224, -268.4436776839389722 ) ) ;
#78063 = CARTESIAN_POINT ( 'NONE',  ( -44.62737072644875980, -293.1440563135716388, -345.0584305643869811 ) ) ;
#78064 = ORIENTED_EDGE ( 'NONE', *, *, #53698, .F. ) ;
#78065 = CARTESIAN_POINT ( 'NONE',  ( 150.7067237505056596, 20.03350844490810800, 5.072059973230453878 ) ) ;
#78066 = CARTESIAN_POINT ( 'NONE',  ( 16.78798984941439443, -292.3565922022360155, -221.2158878559043842 ) ) ;
#78067 = CARTESIAN_POINT ( 'NONE',  ( 207.8273378092535211, 29.30631323223389018, 13.54762445178045738 ) ) ;
#78068 = CARTESIAN_POINT ( 'NONE',  ( -92.05005921254146983, -270.6952119285918457, -226.6919474004047572 ) ) ;
#78069 = CARTESIAN_POINT ( 'NONE',  ( -93.48246105589508659, -296.3275259632841880, -217.9286993795860212 ) ) ;
#78070 = CARTESIAN_POINT ( 'NONE',  ( 34.16983101757539032, -279.3691288536743969, -245.1761672046240790 ) ) ;
#78071 = CARTESIAN_POINT ( 'NONE',  ( -102.4893226013559371, -285.3396367682113919, -310.4745266897137981 ) ) ;
#78072 = CARTESIAN_POINT ( 'NONE',  ( 19.51652875285404676, -286.7379501504116774, -224.5576706834501977 ) ) ;
#78073 = CARTESIAN_POINT ( 'NONE',  ( -16.16327066967548021, -278.2935859473080882, -340.9992073342293111 ) ) ;
#78074 = CARTESIAN_POINT ( 'NONE',  ( -64.18348173831088843, -293.4240369830604891, -340.0676365198945064 ) ) ;
#78075 = CARTESIAN_POINT ( 'NONE',  ( -47.91595552745854292, -296.9484807267889437, -343.6671803159232468 ) ) ;
#78076 = CARTESIAN_POINT ( 'NONE',  ( 5.616831537261391283, -275.2508945685091817, -329.9360129651079205 ) ) ;
#78077 = VERTEX_POINT ( 'NONE', #56526 ) ;
#78078 = FACE_BOUND ( 'NONE', #53945, .T. ) ;
#78079 = CARTESIAN_POINT ( 'NONE',  ( -106.4924653643163452, -296.6533104477818483, -236.5392913216862212 ) ) ;
#78080 = CARTESIAN_POINT ( 'NONE',  ( 21.51069490846390408, -290.1020244241570936, -315.9636680769573900 ) ) ;
#78081 = CARTESIAN_POINT ( 'NONE',  ( 202.0873885898396338, 295.7612547068911226, -54.00000000005271517 ) ) ;
#78082 = CARTESIAN_POINT ( 'NONE',  ( 22.04934442253710003, -288.7985424882168104, -312.9826676442696680 ) ) ;
#78084 = ORIENTED_EDGE ( 'NONE', *, *, #46974, .F. ) ;
#78083 = EDGE_CURVE ( 'NONE', #65957, #47026, #59077, .T. ) ;
#78085 = CARTESIAN_POINT ( 'NONE',  ( -64.64738932163504614, -278.7630909172327165, -198.5609388446419814 ) ) ;
#78086 = CARTESIAN_POINT ( 'NONE',  ( -86.32400088434911822, -296.3631495316701034, -329.6405157434542730 ) ) ;
#78087 = CARTESIAN_POINT ( 'NONE',  ( -112.4385296479938035, -288.8242006916239575, -259.9394053488470604 ) ) ;
#78088 = CARTESIAN_POINT ( 'NONE',  ( -77.06767906920180167, -295.9020624739444543, -336.3593935745793146 ) ) ;
#78089 = CARTESIAN_POINT ( 'NONE',  ( 27.17874114803742458, -294.3523879368091229, -304.6627473358265092 ) ) ;
#78090 = CARTESIAN_POINT ( 'NONE',  ( 165.2494399300530290, -11.64849832608277325, 10.00000000000000000 ) ) ;
#78091 = SURFACE_STYLE_USAGE ( .BOTH. , #78553 ) ;
#78092 = DIRECTION ( 'NONE',  ( 1.000000000000000000, 0.000000000000000000, -0.000000000000000000 ) ) ;
#78093 = CARTESIAN_POINT ( 'NONE',  ( 33.40684426212698099, -289.4401213434811098, -299.0913033591211274 ) ) ;
#78094 = CARTESIAN_POINT ( 'NONE',  ( 44.71564893372296723, -278.0519495502701375, -270.3284710469131937 ) ) ;
#78095 = ORIENTED_EDGE ( 'NONE', *, *, #63231, .T. ) ;
#78096 = CARTESIAN_POINT ( 'NONE',  ( 8.492444172443342154, -280.0097280366674113, -208.5491200923931672 ) ) ;
#78097 = CARTESIAN_POINT ( 'NONE',  ( 6.690891535007532198, -284.4519230596821444, -330.8686323516036509 ) ) ;
#78098 = CARTESIAN_POINT ( 'NONE',  ( 15.90171716690819892, -285.3637075533840743, -215.5546876419895455 ) ) ;
#78099 = CARTESIAN_POINT ( 'NONE',  ( -91.65993919530676237, -287.9130770110612048, -321.3367461437783277 ) ) ;
#78100 = CARTESIAN_POINT ( 'NONE',  ( 16.10102229784061834, -278.1648091990335274, -324.1389714895616407 ) ) ;
#78101 = ORIENTED_EDGE ( 'NONE', *, *, #20867, .F. ) ;
#78103 = CARTESIAN_POINT ( 'NONE',  ( -34.30079519696562329, -279.4399395265006660, -197.3098990009437443 ) ) ;
#78102 = CARTESIAN_POINT ( 'NONE',  ( -96.40570294426359510, -279.1525450687675516, -227.4607267101017385 ) ) ;
#78104 = CARTESIAN_POINT ( 'NONE',  ( 3.349194028415048763, -277.5989106332669962, -335.4293566858443114 ) ) ;
#78105 = CARTESIAN_POINT ( 'NONE',  ( -103.0629969284240985, -277.8640761644923032, -230.9042351043891870 ) ) ;
#78106 = CARTESIAN_POINT ( 'NONE',  ( -49.18953983233350158, -154.2942235963202791, -362.3100455858933060 ) ) ;
#78107 = CARTESIAN_POINT ( 'NONE',  ( -32.70881697004364241, -275.0504157368431493, -193.7232294712062810 ) ) ;
#78108 = EDGE_CURVE ( 'NONE', #90054, #25728, #85383, .T. ) ;
#78109 = ITEM_DEFINED_TRANSFORMATION ( 'NONE', 'NONE', #12874,  #18940 ) ;
#78110 = CARTESIAN_POINT ( 'NONE',  ( -73.02176949901455316, -299.0143876308192148, -202.7339417031545281 ) ) ;
#78111 = CARTESIAN_POINT ( 'NONE',  ( 35.77081079830085031, -289.8376638359844719, -253.6410175316879361 ) ) ;
#78112 = EDGE_LOOP ( 'NONE', ( #78695, #78688, #680, #11535 ) ) ;
#78113 = DIRECTION ( 'NONE',  ( 0.000000000000000000, -1.000000000000000000, 0.000000000000000000 ) ) ;
#78114 = CARTESIAN_POINT ( 'NONE',  ( 29.71334334767416507, -289.0303694817180258, -300.1156040278231103 ) ) ;
#78115 = CARTESIAN_POINT ( 'NONE',  ( -105.7763437893944456, -286.7416523193910507, -237.3357707742747778 ) ) ;
#78116 = EDGE_CURVE ( 'NONE', #53738, #19033, #81432, .T. ) ;
#78117 = CARTESIAN_POINT ( 'NONE',  ( -21.11476984719934080, -288.1869865413264620, -341.6393011909145798 ) ) ;
#78118 = CARTESIAN_POINT ( 'NONE',  ( -66.55869265611643470, -282.9323418135126076, -341.5503888361544682 ) ) ;
#78119 = CARTESIAN_POINT ( 'NONE',  ( 17.67262830335883450, -279.2559124369163328, -221.1690039466874680 ) ) ;
#78120 = CARTESIAN_POINT ( 'NONE',  ( -1.612341663451327678, -288.3910328146881170, -205.2321168238686937 ) ) ;
#78121 = CARTESIAN_POINT ( 'NONE',  ( 27.07418708481774416, -279.5472425279842241, -234.5658497833289005 ) ) ;
#78122 = CARTESIAN_POINT ( 'NONE',  ( -64.49990146468725527, -278.7292768637358336, -338.7062659103573310 ) ) ;
#78123 = CARTESIAN_POINT ( 'NONE',  ( 35.16795938795580412, -276.1679627353783530, -279.7280099715379151 ) ) ;
#78124 = CARTESIAN_POINT ( 'NONE',  ( 30.00623854018101611, -286.8229709056450361, -306.9722039344758286 ) ) ;
#78125 = CARTESIAN_POINT ( 'NONE',  ( -27.38287775629013154, -283.7316426767608277, -346.6047914931318701 ) ) ;
#78126 = CARTESIAN_POINT ( 'NONE',  ( -102.8623873487384088, -284.5169425481083749, -310.6918314558797078 ) ) ;
#78127 = CARTESIAN_POINT ( 'NONE',  ( -10.97378853559589551, -282.8654076314809913, -338.4862295860845620 ) ) ;
#78128 = ORIENTED_EDGE ( 'NONE', *, *, #46981, .T. ) ;
#78129 = ORIENTED_EDGE ( 'NONE', *, *, #36918, .F. ) ;
#78130 = CARTESIAN_POINT ( 'NONE',  ( 202.9738562182569694, 293.9636489450776367, 3.999999999999991562 ) ) ;
#78131 = CARTESIAN_POINT ( 'NONE',  ( 26.41834574880639863, -289.9592940477430147, -311.3841986868908407 ) ) ;
#78132 = CARTESIAN_POINT ( 'NONE',  ( -81.63118595850768600, -290.1478534872501882, -207.9773082523015546 ) ) ;
#78133 = CARTESIAN_POINT ( 'NONE',  ( -110.4226823353708937, -271.6829154849941119, -264.8839556211831905 ) ) ;
#78134 = CARTESIAN_POINT ( 'NONE',  ( 37.96907782122586639, -293.0953925575020094, -285.9045896564433633 ) ) ;
#78135 = CARTESIAN_POINT ( 'NONE',  ( -78.57826584841215833, -288.0980639559382439, -331.4983610439551853 ) ) ;
#78136 = CARTESIAN_POINT ( 'NONE',  ( -5.586818723188489599, -290.7154999873113184, -203.4920638445140924 ) ) ;
#78137 = CARTESIAN_POINT ( 'NONE',  ( -107.3260747433741500, -291.4635883352420365, -292.6496351781394196 ) ) ;
#78138 = CARTESIAN_POINT ( 'NONE',  ( 31.03373250439201669, -301.4082689599840705, -195.3320873922940848 ) ) ;
#78139 = CARTESIAN_POINT ( 'NONE',  ( -72.22056698076656289, -291.5136513959164404, -336.7717638204637751 ) ) ;
#78140 = CARTESIAN_POINT ( 'NONE',  ( -95.15213559790508668, -289.2139908476052028, -222.2997750956995731 ) ) ;
#78141 = CARTESIAN_POINT ( 'NONE',  ( -111.1497079133605297, -292.3803911499525157, -283.7507008984343315 ) ) ;
#78142 = CARTESIAN_POINT ( 'NONE',  ( -27.81778322067169285, -287.1173217162890410, -197.7477345432518803 ) ) ;
#78143 = CARTESIAN_POINT ( 'NONE',  ( 18.04707330162870349, -294.8440685000667827, -219.5466298389553685 ) ) ;
#78144 = DIRECTION ( 'NONE',  ( -0.000000000000000000, -1.000000000000000000, -0.000000000000000000 ) ) ;
#78145 = DIRECTION ( 'NONE',  ( 1.000000000000000000, 0.000000000000000000, 0.000000000000000000 ) ) ;
#78146 = CARTESIAN_POINT ( 'NONE',  ( -31.41511807427017899, -276.1065096258465132, -195.2263364042563865 ) ) ;
#78147 = CARTESIAN_POINT ( 'NONE',  ( -110.1958620557682735, -295.4411499741268585, -294.7830325296898195 ) ) ;
#78148 = CARTESIAN_POINT ( 'NONE',  ( -35.34077346015080678, -272.3174319252889859, -196.3621547258715907 ) ) ;
#78149 = CARTESIAN_POINT ( 'NONE',  ( -106.6166514506029159, -276.2747047338826860, -297.6062150647823614 ) ) ;
#78150 = CARTESIAN_POINT ( 'NONE',  ( -34.47241943930104924, -299.4039840146938900, -196.8673052391749820 ) ) ;
#78151 = CARTESIAN_POINT ( 'NONE',  ( -15.92497645602875700, -272.8984603680809755, -196.9581903346149829 ) ) ;
#78152 = CARTESIAN_POINT ( 'NONE',  ( -95.22576251495287636, -297.3417654636216980, -315.8013010876480280 ) ) ;
#78153 = CARTESIAN_POINT ( 'NONE',  ( 165.0427047786672290, 275.0000000000000568, 23.37680765314704701 ) ) ;
#78154 = CARTESIAN_POINT ( 'NONE',  ( -110.4023911443710517, -297.3044599074138432, -274.2000181807960644 ) ) ;
#78155 = CARTESIAN_POINT ( 'NONE',  ( 201.2104617360081704, 25.32700003806615996, 10.00000000000000000 ) ) ;
#78157 = CARTESIAN_POINT ( 'NONE',  ( -72.84688197322741132, -297.5677205883679335, -206.5772480612146182 ) ) ;
#78156 = CARTESIAN_POINT ( 'NONE',  ( 1.906320906490790223, -284.5947088680614456, -206.0338325817769487 ) ) ;
#78158 = CARTESIAN_POINT ( 'NONE',  ( 2.741011375799959460, -286.5742817885151794, -204.6163369083437544 ) ) ;
#78159 = CARTESIAN_POINT ( 'NONE',  ( -57.28951361561180988, -288.9693248741229468, -344.7655802980067392 ) ) ;
#78160 = CARTESIAN_POINT ( 'NONE',  ( -110.9982694717852780, -298.7360770413811792, -254.3911565861511974 ) ) ;
#78161 = CARTESIAN_POINT ( 'NONE',  ( -56.29155764638935011, -293.2965588898631495, -342.8090991580810396 ) ) ;
#78162 = CARTESIAN_POINT ( 'NONE',  ( -56.50647530761765580, -279.0085380875518126, -195.8960865851302344 ) ) ;
#78163 = CARTESIAN_POINT ( 'NONE',  ( 35.77081079830085031, -285.2666405000204577, -287.0812184334320705 ) ) ;
#78164 = FACE_OUTER_BOUND ( 'NONE', #12388, .T. ) ;
#78165 = CARTESIAN_POINT ( 'NONE',  ( -68.94276687916048729, -288.2721729156947958, -336.6068958587171664 ) ) ;
#78166 = CARTESIAN_POINT ( 'NONE',  ( 138.6539576904058606, 249.5000000000000568, 10.50000000000000000 ) ) ;
#78167 = CARTESIAN_POINT ( 'NONE',  ( -61.93421492268576145, -287.3716847480724823, -341.2145502469942357 ) ) ;
#78168 = CARTESIAN_POINT ( 'NONE',  ( -39.20877240894571258, -299.6284989585577705, -196.5721919568737235 ) ) ;
#78169 = CARTESIAN_POINT ( 'NONE',  ( 25.78351116305544011, -282.4040907476954771, -227.2128857121682586 ) ) ;
#78171 = CARTESIAN_POINT ( 'NONE',  ( 32.23131939602069451, -281.8471831943485313, -292.6299335906476813 ) ) ;
#78170 = CARTESIAN_POINT ( 'NONE',  ( -100.2689438469268310, -294.0142056378176676, -311.9111575173043320 ) ) ;
#78172 = CARTESIAN_POINT ( 'NONE',  ( -113.3898825005471451, -296.8708226820280629, -258.2080291540393659 ) ) ;
#78173 = CARTESIAN_POINT ( 'NONE',  ( -110.1685606238186210, -274.1202508383929626, -259.4470971184537120 ) ) ;
#78174 = EDGE_CURVE ( 'NONE', #50719, #79037, #92313, .T. ) ;
#78175 = CARTESIAN_POINT ( 'NONE',  ( 35.91759642342782399, -283.7593415629847868, -286.4852652283802854 ) ) ;
#78176 = CARTESIAN_POINT ( 'NONE',  ( -104.1561834864384508, -295.2067863679745869, -300.4723459569428314 ) ) ;
#78177 = CARTESIAN_POINT ( 'NONE',  ( 208.4306832106271088, -74.55766379199613425, 0.000000000000000000 ) ) ;
#78178 = CARTESIAN_POINT ( 'NONE',  ( -32.00346527606124170, -284.9643559479886221, -344.8147952057261136 ) ) ;
#78179 = CARTESIAN_POINT ( 'NONE',  ( 165.2494399300530290, 8.542400036368780647, 10.00000000000000000 ) ) ;
#78180 = CARTESIAN_POINT ( 'NONE',  ( 10.59707575819633618, -285.9094976428776818, -330.5268031993606428 ) ) ;
#78181 = CARTESIAN_POINT ( 'NONE',  ( -4.074031739948677178, -275.8217601209036616, -339.6390031621251069 ) ) ;
#78182 = CARTESIAN_POINT ( 'NONE',  ( -36.20400071169095924, -291.9000928814721192, -197.3575075417269318 ) ) ;
#78183 = CARTESIAN_POINT ( 'NONE',  ( 35.24672098506439966, -282.9061459568919190, -257.6477834972278060 ) ) ;
#78184 = CARTESIAN_POINT ( 'NONE',  ( 32.86545046033224793, -277.4507883913867090, -293.1074676097956058 ) ) ;
#78185 = CARTESIAN_POINT ( 'NONE',  ( -109.6611063110171074, -285.6642053532696650, -295.0291090164496381 ) ) ;
#78186 = CARTESIAN_POINT ( 'NONE',  ( -76.35109088460164628, -282.3809962773257212, -332.5935568054922555 ) ) ;
#78187 = CARTESIAN_POINT ( 'NONE',  ( -95.50732103470559764, -281.2045895960123403, -223.0138773276377719 ) ) ;
#78188 = CARTESIAN_POINT ( 'NONE',  ( -110.1025574160018579, -273.0364890683796375, -245.1647362735621414 ) ) ;
#78189 = CARTESIAN_POINT ( 'NONE',  ( 33.01890935381643288, -275.7846940342395783, -301.6402586008851472 ) ) ;
#78190 = CARTESIAN_POINT ( 'NONE',  ( 17.23113993169376101, -296.1858419071984940, -320.9883767091038749 ) ) ;
#78191 = DIRECTION ( 'NONE',  ( 0.000000000000000000, 1.000000000000000000, 0.000000000000000000 ) ) ;
#78192 = DIRECTION ( 'NONE',  ( 0.000000000000000000, -0.000000000000000000, 1.000000000000000000 ) ) ;
#78193 = EDGE_CURVE ( 'NONE', #35594, #75749, #50005, .T. ) ;
#78194 = CARTESIAN_POINT ( 'NONE',  ( -112.8871706354899516, -294.7732105220253516, -263.9509943620176955 ) ) ;
#78195 = CARTESIAN_POINT ( 'NONE',  ( -6.256133189139672979, -276.1400287222732572, -336.4935480826406433 ) ) ;
#78196 = CARTESIAN_POINT ( 'NONE',  ( 12.95351572872406365, -295.8852534934060259, -327.8167220553053767 ) ) ;
#78197 = CARTESIAN_POINT ( 'NONE',  ( 30.55751651418675507, -295.2171216475704796, -305.8252561628572721 ) ) ;
#78198 = CARTESIAN_POINT ( 'NONE',  ( -7.463671678042305579, -290.6598054510139946, -339.0265230571637289 ) ) ;
#78199 = CARTESIAN_POINT ( 'NONE',  ( -73.75584774849309611, -275.5365553449037748, -335.7519926407345565 ) ) ;
#78200 = CARTESIAN_POINT ( 'NONE',  ( -106.5987690837830684, -280.1143944106486288, -297.6516400629935220 ) ) ;
#78201 = CARTESIAN_POINT ( 'NONE',  ( -109.7045088548589433, -294.4054011891456639, -287.8774202178561268 ) ) ;
#78202 = CARTESIAN_POINT ( 'NONE',  ( 36.46869706612780249, -283.1945915462823677, -253.2065130481381345 ) ) ;
#78203 = CARTESIAN_POINT ( 'NONE',  ( -77.20566991804004431, -284.4245870164913867, -208.7778095031564476 ) ) ;
#78204 = CARTESIAN_POINT ( 'NONE',  ( -111.5753029650709465, -274.4291645131854693, -270.3850168459313181 ) ) ;
#78205 = ORIENTED_EDGE ( 'NONE', *, *, #90641, .F. ) ;
#78206 = CARTESIAN_POINT ( 'NONE',  ( -71.18425261407487881, -285.2591111901812155, -205.6558699104188292 ) ) ;
#78207 = ORIENTED_EDGE ( 'NONE', *, *, #56930, .T. ) ;
#78208 = CARTESIAN_POINT ( 'NONE',  ( 39.10248958358808125, -282.5546423019979443, -264.2147069624708706 ) ) ;
#78209 = CARTESIAN_POINT ( 'NONE',  ( -113.2083300039566467, -283.2091657554186099, -281.3317456748765721 ) ) ;
#78210 = CARTESIAN_POINT ( 'NONE',  ( -108.4340002377611683, -279.1244606192580022, -299.3215233232049854 ) ) ;
#78211 = EDGE_CURVE ( 'NONE', #10842, #86547, #22759, .T. ) ;
#78212 = CARTESIAN_POINT ( 'NONE',  ( -79.82397299963848525, -279.1350294293844740, -333.8121289196917019 ) ) ;
#78213 = CARTESIAN_POINT ( 'NONE',  ( -28.24530500278205380, -280.8159766702625575, -193.9494060382646126 ) ) ;
#78214 = CARTESIAN_POINT ( 'NONE',  ( 27.36219212280433055, -272.6237833571633473, -239.2376011013261916 ) ) ;
#78215 = CARTESIAN_POINT ( 'NONE',  ( 122.8483417650791836, 148.9427304151107307, -263.5502861110473418 ) ) ;
#78216 = ORIENTED_EDGE ( 'NONE', *, *, #80097, .T. ) ;
#78217 = CARTESIAN_POINT ( 'NONE',  ( -3.292708276216301577, -276.5029539112508701, -203.7081979764361392 ) ) ;
#78218 = CARTESIAN_POINT ( 'NONE',  ( 202.8071895515903122, 295.9636489450776367, -54.00000000004035883 ) ) ;
#78219 = CARTESIAN_POINT ( 'NONE',  ( -34.21985529895107447, -278.1116752371696634, -195.7687982677718423 ) ) ;
#78220 = CARTESIAN_POINT ( 'NONE',  ( 23.15468906069257216, -294.6911167974343471, -224.3597084903977077 ) ) ;
#78221 = CARTESIAN_POINT ( 'NONE',  ( 3.867018498677363247, -293.8293822646695048, -330.7410333277059635 ) ) ;
#78222 = CARTESIAN_POINT ( 'NONE',  ( -65.43040447464409226, -288.9171951892036532, -342.0452869295789924 ) ) ;
#78223 = DIRECTION ( 'NONE',  ( 1.000000000000000000, 0.000000000000000000, 0.000000000000000000 ) ) ;
#78225 = CARTESIAN_POINT ( 'NONE',  ( -98.00201650591019131, -283.5315760617929755, -228.3058677575226625 ) ) ;
#78224 = CARTESIAN_POINT ( 'NONE',  ( -30.66068886033499652, -293.5439739987444341, -346.4792523598452476 ) ) ;
#78226 = CARTESIAN_POINT ( 'NONE',  ( -30.71999500373535241, -293.9971708917041155, -196.4218286878305548 ) ) ;
#78227 = CARTESIAN_POINT ( 'NONE',  ( -1.835491417002458325, -285.0110408916730194, -205.7281883333272106 ) ) ;
#78228 = CARTESIAN_POINT ( 'NONE',  ( -61.68236061479817778, -284.6902125115734066, -339.7600452678200895 ) ) ;
#78229 = ORIENTED_EDGE ( 'NONE', *, *, #34825, .T. ) ;
#78230 = CARTESIAN_POINT ( 'NONE',  ( -79.47531798111366186, -292.4396946352862869, -206.1292101712163856 ) ) ;
#78231 = CARTESIAN_POINT ( 'NONE',  ( -33.48671308066791141, -283.4947028727016800, -343.3334675316916105 ) ) ;
#78232 = CARTESIAN_POINT ( 'NONE',  ( 35.98509963879727280, -292.6287501404636373, -292.7034723565416243 ) ) ;
#78233 = CARTESIAN_POINT ( 'NONE',  ( -54.45568091545072065, -290.0693200335015263, -345.3241275155259018 ) ) ;
#78234 = CARTESIAN_POINT ( 'NONE',  ( -112.5038811090080912, -290.8387653768328391, -286.7980718894850725 ) ) ;
#78235 = CARTESIAN_POINT ( 'NONE',  ( 35.63009059669786893, -287.7636400287147467, -273.7577124809947122 ) ) ;
#78236 = ORIENTED_EDGE ( 'NONE', *, *, #899, .F. ) ;
#78237 = FACE_OUTER_BOUND ( 'NONE', #55861, .T. ) ;
#78238 = CARTESIAN_POINT ( 'NONE',  ( -109.6142948817539633, -298.1216896178034403, -293.1416382998448285 ) ) ;
#78239 = CARTESIAN_POINT ( 'NONE',  ( -82.66487049059166736, -296.1323356984701718, -208.6583963620937539 ) ) ;
#78240 = ADVANCED_FACE ( 'NONE', ( #47510 ), #87771, .T. ) ;
#78241 = CARTESIAN_POINT ( 'NONE',  ( -108.0505578942962046, -277.3598136360681110, -289.4311437306490120 ) ) ;
#78242 = CARTESIAN_POINT ( 'NONE',  ( -58.09898027320685543, -273.2987220833773563, -196.2202324819549517 ) ) ;
#78243 = CARTESIAN_POINT ( 'NONE',  ( -99.32687365041907412, -294.4845456379242137, -310.3112039782097895 ) ) ;
#78244 = CARTESIAN_POINT ( 'NONE',  ( 33.49263129951447837, -277.5930543212922998, -291.8636966324963851 ) ) ;
#78245 = CARTESIAN_POINT ( 'NONE',  ( -37.80669735810238308, -296.2861075207721342, -196.3492419481402749 ) ) ;
#78246 = CARTESIAN_POINT ( 'NONE',  ( -28.83480362977233824, -296.1471247591911720, -343.3148325497661517 ) ) ;
#78247 = CARTESIAN_POINT ( 'NONE',  ( -12.89224436125023665, -295.8065999431065052, -339.5264730276013552 ) ) ;
#78248 = CARTESIAN_POINT ( 'NONE',  ( -53.10365836173552623, -296.8509630773195909, -344.9670938096699615 ) ) ;
#78249 = CARTESIAN_POINT ( 'NONE',  ( -86.24960189229837226, -295.3757364917250356, -213.2132306156502750 ) ) ;
#78250 = CARTESIAN_POINT ( 'NONE',  ( -65.37370893771648639, -292.3272120712665583, -202.8338881731086190 ) ) ;
#78251 = CARTESIAN_POINT ( 'NONE',  ( 7.906247026854799742, -299.2561368632369749, -193.4581864202968688 ) ) ;
#78252 = CARTESIAN_POINT ( 'NONE',  ( -91.03501290151477576, -288.4078789402160510, -320.7585411176893331 ) ) ;
#78253 = CARTESIAN_POINT ( 'NONE',  ( -66.61667398526682859, -275.6688505030992928, -201.3105817330240654 ) ) ;
#78254 = CARTESIAN_POINT ( 'NONE',  ( -66.20995228424645518, -274.1766140077583600, -199.0297031343532694 ) ) ;
#78255 = CARTESIAN_POINT ( 'NONE',  ( -72.86087804014364622, -297.9009479429373073, -206.5608398698246049 ) ) ;
#78256 = CARTESIAN_POINT ( 'NONE',  ( -66.74443605542816726, -281.6487294461595638, -200.9789450227856094 ) ) ;
#78257 = CARTESIAN_POINT ( 'NONE',  ( -11.65902343234288097, -279.0644222654100872, -198.2381707162253690 ) ) ;
#78258 = EDGE_LOOP ( 'NONE', ( #82843, #73414, #92141, #82971 ) ) ;
#78259 = CARTESIAN_POINT ( 'NONE',  ( -76.71284650256086479, -282.9128417912821760, -336.4775758886877952 ) ) ;
#78260 = CARTESIAN_POINT ( 'NONE',  ( 38.08077018398219593, -275.0884878916513117, -285.3532412132651643 ) ) ;
#78261 = CARTESIAN_POINT ( 'NONE',  ( 31.30966784710482997, -279.5219981305814372, -237.1726039575034122 ) ) ;
#78262 = CARTESIAN_POINT ( 'NONE',  ( 16.49497035111065202, -280.2894872588807971, -322.8915533308707495 ) ) ;
#78263 = CARTESIAN_POINT ( 'NONE',  ( -35.35638404869035867, -272.6522467003142083, -196.7860660831684640 ) ) ;
#78264 = CARTESIAN_POINT ( 'NONE',  ( 31.37081170764443527, -277.1573261644568333, -240.1737162067874749 ) ) ;
#78265 = CARTESIAN_POINT ( 'NONE',  ( 197.5379522065468052, 250.0000000000000568, -11.97918851819043873 ) ) ;
#78266 = FACE_OUTER_BOUND ( 'NONE', #49102, .T. ) ;
#78267 = CARTESIAN_POINT ( 'NONE',  ( -98.26636462649079817, -295.4043386109883613, -224.9284058695760109 ) ) ;
#78268 = CARTESIAN_POINT ( 'NONE',  ( -14.34391950530947746, -290.3688540135494804, -198.5462537631774183 ) ) ;
#78269 = CARTESIAN_POINT ( 'NONE',  ( 1.700100917900669639, -292.5587675933670084, -203.9319858678950368 ) ) ;
#78270 = CARTESIAN_POINT ( 'NONE',  ( 36.68209423794102975, -277.3840819315672661, -257.2299041075381183 ) ) ;
#78271 = CARTESIAN_POINT ( 'NONE',  ( -46.39563600217162076, -271.9370851214541744, -195.9096109961765819 ) ) ;
#78272 = DIRECTION ( 'NONE',  ( -0.000000000000000000, -0.000000000000000000, 1.000000000000000000 ) ) ;
#78273 = CARTESIAN_POINT ( 'NONE',  ( 34.25268226494973334, -283.7842335365593840, -294.6808344674290083 ) ) ;
#78274 = DIRECTION ( 'NONE',  ( -1.000000000000000000, -0.000000000000000000, -0.000000000000000000 ) ) ;
#78275 = CARTESIAN_POINT ( 'NONE',  ( -111.8967894818025854, -282.6625610866086618, -261.7495260186613564 ) ) ;
#78276 = DIRECTION ( 'NONE',  ( -1.000000000000000000, 0.000000000000000000, 0.000000000000000000 ) ) ;
#78277 = CARTESIAN_POINT ( 'NONE',  ( -55.91854954511688902, -294.0915156814653528, -341.4210509019096094 ) ) ;
#78278 = CARTESIAN_POINT ( 'NONE',  ( 21.33123772657210893, -285.0618616834468639, -224.8819815898654042 ) ) ;
#78279 = LINE ( 'NONE', #88132, #44249 ) ;
#78280 = CARTESIAN_POINT ( 'NONE',  ( 13.69777801911289394, -292.3372727896691003, -325.3865505291607292 ) ) ;
#78281 = CARTESIAN_POINT ( 'NONE',  ( -49.99774993565495862, -281.6905643934345562, -345.6643079940985217 ) ) ;
#78282 = CARTESIAN_POINT ( 'NONE',  ( -32.93538861181966837, -281.7087219086758410, -196.6927744773726943 ) ) ;
#78283 = CARTESIAN_POINT ( 'NONE',  ( -95.52507491415474306, -286.4336857164828416, -220.4548070453019193 ) ) ;
#78284 = CARTESIAN_POINT ( 'NONE',  ( 34.37879508655905170, -279.4693874069580488, -245.1011474304457352 ) ) ;
#78285 = CARTESIAN_POINT ( 'NONE',  ( 32.27359270981354200, -287.2604090777331862, -248.3485840590310261 ) ) ;
#78286 = CARTESIAN_POINT ( 'NONE',  ( -98.12537369434022594, -279.4049043940268007, -311.8426794918250380 ) ) ;
#78287 = CARTESIAN_POINT ( 'NONE',  ( -89.19306452860043066, -278.6072687886634185, -322.0473644619289644 ) ) ;
#78288 = CARTESIAN_POINT ( 'NONE',  ( -51.88116316873244216, -287.8470255392998638, -196.3686488436300408 ) ) ;
#78289 = ORIENTED_EDGE ( 'NONE', *, *, #5090, .F. ) ;
#78290 = CARTESIAN_POINT ( 'NONE',  ( -101.5485180013057374, -296.9448233496169678, -227.8343504451467254 ) ) ;
#78291 = CARTESIAN_POINT ( 'NONE',  ( 22.50703440647753339, -290.1443688299032715, -314.9916680717385020 ) ) ;
#78292 = CARTESIAN_POINT ( 'NONE',  ( 221.8344101925596306, 15.36528803885690664, 21.50000000000000000 ) ) ;
#78293 = CARTESIAN_POINT ( 'NONE',  ( -88.52914483777347243, -287.9090924074130839, -206.2264541496106460 ) ) ;
#78294 = VERTEX_POINT ( 'NONE', #91999 ) ;
#78295 = CARTESIAN_POINT ( 'NONE',  ( -41.07559082729378019, -272.0052366226703384, -195.2362280283337270 ) ) ;
#78296 = CARTESIAN_POINT ( 'NONE',  ( 8.409404898755894919, -292.8372702006462305, -331.2977802006754473 ) ) ;
#78297 = CARTESIAN_POINT ( 'NONE',  ( -109.2284136122852942, -272.0791603529684153, -256.8167345609106178 ) ) ;
#78298 = CARTESIAN_POINT ( 'NONE',  ( 34.96820303596955881, -289.2588488277343686, -284.6386020409750017 ) ) ;
#78299 = CARTESIAN_POINT ( 'NONE',  ( -16.65973667170447925, -282.0831840653772247, -199.2961449017545874 ) ) ;
#78300 = CARTESIAN_POINT ( 'NONE',  ( -57.12073960555999719, -290.7275953252116665, -344.2222733945458799 ) ) ;
#78301 = CARTESIAN_POINT ( 'NONE',  ( -74.17510388940996791, -290.8462840822272710, -337.4327558389133515 ) ) ;
#78302 = CARTESIAN_POINT ( 'NONE',  ( -109.2804093825592275, -286.8275520544906385, -248.9717581267117055 ) ) ;
#78303 = CARTESIAN_POINT ( 'NONE',  ( -19.75828574208869526, -280.4387327722728855, -195.3408655458659666 ) ) ;
#78304 = CARTESIAN_POINT ( 'NONE',  ( -6.409975722179727775, -292.7288920642370726, -339.2998054251737017 ) ) ;
#78305 = CARTESIAN_POINT ( 'NONE',  ( 26.28181498157088569, -280.8123952974474946, -226.8970263228519855 ) ) ;
#78306 = CARTESIAN_POINT ( 'NONE',  ( 35.03278656305512584, -277.1976479175255008, -253.7877331182183411 ) ) ;
#78307 = CARTESIAN_POINT ( 'NONE',  ( -106.6662871844225293, -299.4805209788416391, -237.0123917617630980 ) ) ;
#78308 = CARTESIAN_POINT ( 'NONE',  ( 23.54211671714417875, -274.4049405898031182, -315.8268728129942247 ) ) ;
#78309 = CARTESIAN_POINT ( 'NONE',  ( 175.2296996224750103, 276.0000000000000568, 0.000000000000000000 ) ) ;
#78310 = CARTESIAN_POINT ( 'NONE',  ( 7.184788178814246251, -280.1849474899177608, -212.3714581194895175 ) ) ;
#78311 = CARTESIAN_POINT ( 'NONE',  ( -25.81449592184696584, -278.1135081855322255, -346.0917741324411168 ) ) ;
#78312 = CARTESIAN_POINT ( 'NONE',  ( -6.336058425474879741, -275.7834175514993831, -203.7285909245110247 ) ) ;
#78313 = CARTESIAN_POINT ( 'NONE',  ( -1.070120186143436625, -285.5803442769611706, -202.7061647127713684 ) ) ;
#78314 = CARTESIAN_POINT ( 'NONE',  ( -106.9785084891391023, -291.9829201981611391, -295.4347881104945372 ) ) ;
#78315 = CARTESIAN_POINT ( 'NONE',  ( -60.64604339787312881, -275.3550378565459482, -197.7571250308804451 ) ) ;
#78316 = CARTESIAN_POINT ( 'NONE',  ( -103.8094469705283842, -274.3637462301140317, -232.3689197104448283 ) ) ;
#78317 = CARTESIAN_POINT ( 'NONE',  ( 152.4536156746142410, 275.5000000000000568, -12.49999999999999289 ) ) ;
#78318 = CARTESIAN_POINT ( 'NONE',  ( -109.3604362198488502, -298.2901384300380414, -290.6916388824978981 ) ) ;
#78319 = CARTESIAN_POINT ( 'NONE',  ( -38.94937919989016706, -281.0721757532335232, -345.1899886907590371 ) ) ;
#78320 = CARTESIAN_POINT ( 'NONE',  ( -92.79390621262160721, -290.9507028680513940, -216.8924315482295242 ) ) ;
#78321 = CARTESIAN_POINT ( 'NONE',  ( 24.42727591624192129, -273.0020381159397402, -228.4282720569481455 ) ) ;
#78322 = CARTESIAN_POINT ( 'NONE',  ( 7.061050246335325298, -288.2454037619567657, -208.3700882003813604 ) ) ;
#78323 = CARTESIAN_POINT ( 'NONE',  ( -69.13929068415136214, -290.5441636556618619, -204.2931938160888876 ) ) ;
#78324 = EDGE_LOOP ( 'NONE', ( #6970, #66246, #7277, #26151 ) ) ;
#78325 = CARTESIAN_POINT ( 'NONE',  ( -111.6935907602036053, -288.9041413973887416, -288.0354051462061875 ) ) ;
#78326 = CARTESIAN_POINT ( 'NONE',  ( -95.12852218884312094, -290.8471963740800561, -225.7206578260619665 ) ) ;
#78327 = VERTEX_POINT ( 'NONE', #76416 ) ;
#78328 = CARTESIAN_POINT ( 'NONE',  ( -1.127709513165200628, -287.6009411039925112, -202.7590514895931619 ) ) ;
#78329 = CARTESIAN_POINT ( 'NONE',  ( -100.5990294264053233, -278.3841973351577508, -306.9400203185992950 ) ) ;
#78330 = CARTESIAN_POINT ( 'NONE',  ( 1.600581836954556803, -293.4645680352248860, -336.4291979080119290 ) ) ;
#78331 = CARTESIAN_POINT ( 'NONE',  ( -114.2250769792311331, -285.2440651346432787, -267.1269796536276431 ) ) ;
#78332 = CARTESIAN_POINT ( 'NONE',  ( -112.5035268974379363, -284.6774356220762456, -286.9877258253117702 ) ) ;
#78333 = CARTESIAN_POINT ( 'NONE',  ( 5.607951058262628408, -282.7853120791038464, -329.4154569396601460 ) ) ;
#78334 = CARTESIAN_POINT ( 'NONE',  ( -63.59754655805116386, -182.8661901358721309, -362.5093420553077976 ) ) ;
#78335 = CARTESIAN_POINT ( 'NONE',  ( -32.41727912486597063, -123.7363485282854896, -362.9951886188725894 ) ) ;
#78336 = CARTESIAN_POINT ( 'NONE',  ( -112.1542233637230908, -270.3668851746004407, -283.6615718338756551 ) ) ;
#78337 = CARTESIAN_POINT ( 'NONE',  ( -74.34624968938332756, -272.7440816174270708, -207.1893234989277914 ) ) ;
#78338 = CARTESIAN_POINT ( 'NONE',  ( 29.37303827091535169, -274.0630553738110393, -239.8512678150489137 ) ) ;
#78339 = CARTESIAN_POINT ( 'NONE',  ( -72.05188845079854332, -295.0064864794960613, -339.0250075467953934 ) ) ;
#78340 = CARTESIAN_POINT ( 'NONE',  ( 203.3290562182569943, 291.9839156117442940, -53.99999999998728129 ) ) ;
#78341 = CARTESIAN_POINT ( 'NONE',  ( -1.517488088399022050, -273.2018580692800924, -202.7599041949939931 ) ) ;
#78342 = CARTESIAN_POINT ( 'NONE',  ( -110.2634163752252192, -298.5937993823400234, -256.3904709118299934 ) ) ;
#78343 = CARTESIAN_POINT ( 'NONE',  ( -44.34335962587524449, -293.0413301273801494, -197.3360970108299455 ) ) ;
#78344 = ORIENTED_EDGE ( 'NONE', *, *, #85799, .F. ) ;
#78345 = CARTESIAN_POINT ( 'NONE',  ( -87.31819247139647189, -298.3166755962409979, -212.0229436309392668 ) ) ;
#78346 = CARTESIAN_POINT ( 'NONE',  ( -18.45155229318037371, -289.2946306705424604, -340.9910173114611212 ) ) ;
#78347 = CARTESIAN_POINT ( 'NONE',  ( 33.27222314002835191, -294.7431795583277108, -300.7912860737888536 ) ) ;
#78348 = CARTESIAN_POINT ( 'NONE',  ( -47.61714456234479087, -295.6718046058143159, -346.6103287640002577 ) ) ;
#78349 = CARTESIAN_POINT ( 'NONE',  ( 30.58634157623776417, -294.0780099583164997, -297.2348242193176020 ) ) ;
#78350 = ORIENTED_EDGE ( 'NONE', *, *, #87501, .F. ) ;
#78351 = CARTESIAN_POINT ( 'NONE',  ( 17.03597120988462521, -276.7395145957429463, -217.8228770296917105 ) ) ;
#78352 = ADVANCED_FACE ( 'NONE', ( #19574 ), #83250, .F. ) ;
#78353 = ORIENTED_EDGE ( 'NONE', *, *, #69069, .F. ) ;
#78354 = CARTESIAN_POINT ( 'NONE',  ( -106.1177533559898336, -278.5051262261009697, -235.7550713857343112 ) ) ;
#78355 = CIRCLE ( 'NONE', #67727, 6.286090667950827715 ) ;
#78356 = CARTESIAN_POINT ( 'NONE',  ( 33.08297254554128841, -276.2264248726715437, -250.0858929216487923 ) ) ;
#78357 = CARTESIAN_POINT ( 'NONE',  ( -27.15485575526050255, -275.9399409156598608, -195.0076471617659877 ) ) ;
#78358 = CARTESIAN_POINT ( 'NONE',  ( 30.36609332827191565, -274.0076102129252718, -303.5564886503789808 ) ) ;
#78359 = CARTESIAN_POINT ( 'NONE',  ( -69.30959058829047592, -298.2714248764343097, -204.6196040959292191 ) ) ;
#78360 = CARTESIAN_POINT ( 'NONE',  ( -68.78546357107944687, -294.0484813987965822, -336.9081459888010386 ) ) ;
#78361 = CARTESIAN_POINT ( 'NONE',  ( 164.2231345125756263, 300.2961574867697436, -7.500000000000000000 ) ) ;
#78362 = CARTESIAN_POINT ( 'NONE',  ( -96.77390321102514292, -279.7015354658562387, -221.4802143903870899 ) ) ;
#78363 = CARTESIAN_POINT ( 'NONE',  ( 33.58703610328374367, -275.9472700432625629, -287.6797706704508641 ) ) ;
#78364 = APPLICATION_CONTEXT ( 'automotive_design' ) ;
#78365 = CARTESIAN_POINT ( 'NONE',  ( 26.73394810780187569, -285.6842630779813135, -228.5566974557147262 ) ) ;
#78366 = CARTESIAN_POINT ( 'NONE',  ( -67.46667442081138688, -299.6582395621390447, -201.4397465638191420 ) ) ;
#78367 = CARTESIAN_POINT ( 'NONE',  ( 82.68044179851318631, -297.0770420877388460, -195.7386261002818912 ) ) ;
#78368 = CARTESIAN_POINT ( 'NONE',  ( 35.81655398972591087, -286.7583535030299799, -271.0478354302956063 ) ) ;
#78369 = CARTESIAN_POINT ( 'NONE',  ( 19.63028343106945428, -279.1309812026076997, -223.0956244082971125 ) ) ;
#78370 = CARTESIAN_POINT ( 'NONE',  ( -65.02104947398494517, -278.2580079355589646, -202.1758663696145675 ) ) ;
#78371 = CARTESIAN_POINT ( 'NONE',  ( -86.82248143355772640, -287.3644923948191376, -213.9312115247869315 ) ) ;
#78372 = CARTESIAN_POINT ( 'NONE',  ( -8.568951285032019527, -277.8720777042691452, -337.8970240043456101 ) ) ;
#78373 = DIRECTION ( 'NONE',  ( 0.5370370370370398660, -2.048677426712644618E-14, 0.8435586647355814982 ) ) ;
#78374 = CARTESIAN_POINT ( 'NONE',  ( -41.35365668423214913, -275.3418465024450370, -346.2548370054150837 ) ) ;
#78375 = CARTESIAN_POINT ( 'NONE',  ( -38.09171799484808218, -274.6939233269887950, -197.2630322226893611 ) ) ;
#78376 = CARTESIAN_POINT ( 'NONE',  ( 34.41771835781664635, -283.2643670656914878, -247.9867065829535306 ) ) ;
#78377 = FACE_OUTER_BOUND ( 'NONE', #37610, .T. ) ;
#78378 = CARTESIAN_POINT ( 'NONE',  ( 15.69299422997897153, -290.2292460827072205, -324.2542994614541954 ) ) ;
#78379 = CARTESIAN_POINT ( 'NONE',  ( -8.888675440074152334, -290.4241454990054763, -200.9541106807363064 ) ) ;
#78380 = PLANE ( 'NONE',  #13404 ) ;
#78381 = CARTESIAN_POINT ( 'NONE',  ( 28.30927743145671727, -273.7916668127161870, -237.3279131416217353 ) ) ;
#78382 = CARTESIAN_POINT ( 'NONE',  ( 34.97337904310720802, -291.9099984919495796, -287.1918667519220776 ) ) ;
#78383 = CARTESIAN_POINT ( 'NONE',  ( -111.8441652935849646, -278.1196860901031300, -270.4320060261264871 ) ) ;
#78384 = DIRECTION ( 'NONE',  ( -1.000000000000000000, -0.000000000000000000, -0.000000000000000000 ) ) ;
#78385 = CARTESIAN_POINT ( 'NONE',  ( -98.48529726871387879, -288.4189354325264958, -316.0354243202887119 ) ) ;
#78386 = CARTESIAN_POINT ( 'NONE',  ( -74.17862599039634119, -285.1502030596065538, -334.3683977373329412 ) ) ;
#78387 = CARTESIAN_POINT ( 'NONE',  ( 34.97637758395062235, -286.0892622408953230, -293.6864186126551886 ) ) ;
#78388 = CARTESIAN_POINT ( 'NONE',  ( -99.51925121296332577, -285.4366913320662320, -309.8179703291999658 ) ) ;
#78389 = CARTESIAN_POINT ( 'NONE',  ( -51.03812470570034066, -284.0343867308039307, -342.2808091758216733 ) ) ;
#78390 = CARTESIAN_POINT ( 'NONE',  ( -35.03654083359199944, -294.0608247401532367, -195.0283106696795983 ) ) ;
#78391 = CARTESIAN_POINT ( 'NONE',  ( 36.81038724188080380, -273.4469698837517626, -255.8427799423238014 ) ) ;
#78392 = CARTESIAN_POINT ( 'NONE',  ( 22.62720205646445848, -276.5326587223444221, -318.6466053410275663 ) ) ;
#78393 = CARTESIAN_POINT ( 'NONE',  ( -111.1638028333777868, -288.4266546160624785, -286.4735775844918635 ) ) ;
#78394 = CARTESIAN_POINT ( 'NONE',  ( -98.80342328284632458, -277.9342014865476926, -316.7665546254544893 ) ) ;
#78395 = CARTESIAN_POINT ( 'NONE',  ( -42.47829642095573632, -297.0971599397786918, -344.8289780431859413 ) ) ;
#78396 = CARTESIAN_POINT ( 'NONE',  ( 85.55100297371609486, -298.0521521680024080, -521.1711561948568487 ) ) ;
#78397 = DIRECTION ( 'NONE',  ( 0.000000000000000000, 0.000000000000000000, -1.000000000000000000 ) ) ;
#78398 = CARTESIAN_POINT ( 'NONE',  ( -78.66766804204782204, -282.3066913607690935, -331.1345320139957380 ) ) ;
#78399 = ADVANCED_FACE ( 'NONE', ( #70721 ), #27627, .T. ) ;
#78400 = CARTESIAN_POINT ( 'NONE',  ( -2.053338970258056229, -278.5192938388750008, -204.1815726689978021 ) ) ;
#78401 = EDGE_CURVE ( 'NONE', #83027, #37103, #57599, .T. ) ;
#78402 = CARTESIAN_POINT ( 'NONE',  ( 175.2296996224749250, 275.5000000000000568, -24.99999999999999289 ) ) ;
#78403 = CARTESIAN_POINT ( 'NONE',  ( 9.103795711878566621, -273.1567691800516968, -209.8175496446503701 ) ) ;
#78404 = CARTESIAN_POINT ( 'NONE',  ( -11.22536265483237372, -276.0511823895362227, -338.6387100988942507 ) ) ;
#78405 = CARTESIAN_POINT ( 'NONE',  ( 10.75856280437803214, -295.8928824573421252, -326.1918662891938538 ) ) ;
#78406 = CARTESIAN_POINT ( 'NONE',  ( 37.37945845847486481, -280.2549802172915179, -253.0337193628718353 ) ) ;
#78407 = CARTESIAN_POINT ( 'NONE',  ( -15.51129814104582216, -295.7039670232302910, -340.3204145593449539 ) ) ;
#78408 = CARTESIAN_POINT ( 'NONE',  ( -96.12171209824758478, -297.2041448875631318, -319.3529893802767674 ) ) ;
#78409 = CARTESIAN_POINT ( 'NONE',  ( -96.29592946883931859, -272.8230558558606731, -227.1901537869062224 ) ) ;
#78410 = CARTESIAN_POINT ( 'NONE',  ( -87.27917837666056755, -293.3566860727104881, -214.3336309366040950 ) ) ;
#78411 = CARTESIAN_POINT ( 'NONE',  ( -49.34682206839899976, -286.0699846215512139, -194.2490027569031383 ) ) ;
#78412 = CARTESIAN_POINT ( 'NONE',  ( -8.144324461542206350, -272.5699349044903101, -200.3924827513508546 ) ) ;
#78413 = CARTESIAN_POINT ( 'NONE',  ( 25.54633227888296432, -286.7972556030635474, -225.9075912452445323 ) ) ;
#78414 = CARTESIAN_POINT ( 'NONE',  ( -86.58781622024113744, -281.3436857260083457, -214.2659591026491057 ) ) ;
#78415 = CARTESIAN_POINT ( 'NONE',  ( 0.2998550268531107732, -285.6252057537514588, -207.4806428895656722 ) ) ;
#78416 = CIRCLE ( 'NONE', #2835, 4.000000000000003553 ) ;
#78417 = CARTESIAN_POINT ( 'NONE',  ( -48.59473957666993016, -287.1951287104843118, -344.5646564750267089 ) ) ;
#78418 = CARTESIAN_POINT ( 'NONE',  ( -110.2140130185358942, -271.2396475792842807, -270.3444066551136871 ) ) ;
#78419 = CARTESIAN_POINT ( 'NONE',  ( 35.05799769567690305, -286.9256033758499598, -260.1795142919913815 ) ) ;
#78420 = CARTESIAN_POINT ( 'NONE',  ( -8.117325910327814142, -283.6200023080649544, -341.4016855523141771 ) ) ;
#78421 = CARTESIAN_POINT ( 'NONE',  ( -66.91369441533387885, -290.7326943542555000, -199.5210349282357640 ) ) ;
#78422 = CARTESIAN_POINT ( 'NONE',  ( -96.21251145214854716, -280.8091371125991600, -221.9603711676448654 ) ) ;
#78423 = CARTESIAN_POINT ( 'NONE',  ( -111.2589409935327609, -280.1166075648310425, -250.5737354612289778 ) ) ;
#78424 = CARTESIAN_POINT ( 'NONE',  ( 25.55795177190707079, -281.8955526958179121, -307.5100733637838744 ) ) ;
#78425 = CARTESIAN_POINT ( 'NONE',  ( 6.320955576305673063, -276.6447947840239294, -209.3168402642163244 ) ) ;
#78426 = CARTESIAN_POINT ( 'NONE',  ( 1.769434916572098615, -294.5440652500597594, -336.6884812312139843 ) ) ;
#78427 = CARTESIAN_POINT ( 'NONE',  ( -18.07268976553725892, -286.8227891367428697, -342.5297369036424016 ) ) ;
#78428 = SHAPE_REPRESENTATION ( 'MAS-324', ( #34088, #70334, #64343, #68826, #53680, #12874, #65816, #71888, #49155, #28012 ), #76393 ) ;
#78429 = CARTESIAN_POINT ( 'NONE',  ( -110.0409435198949240, -295.6014632553917068, -260.5417629004472246 ) ) ;
#78430 = ORIENTED_EDGE ( 'NONE', *, *, #15267, .T. ) ;
#78431 = VERTEX_POINT ( 'NONE', #70263 ) ;
#78432 = CARTESIAN_POINT ( 'NONE',  ( -40.26694038014439769, -285.0093664185279749, -344.7436237853778493 ) ) ;
#78433 = CARTESIAN_POINT ( 'NONE',  ( -47.80025952003029488, -294.8553954343872761, -342.6807050971036119 ) ) ;
#78434 =( BOUNDED_CURVE ( )  B_SPLINE_CURVE ( 3, ( #75730, #90379, #62963, #84224 ),
 .UNSPECIFIED., .F., .F. ) 
 B_SPLINE_CURVE_WITH_KNOTS ( ( 4, 4 ),
 ( 6.022196528194273313, 6.283185307179586232 ),
 .UNSPECIFIED. ) 
 CURVE ( )  GEOMETRIC_REPRESENTATION_ITEM ( )  RATIONAL_B_SPLINE_CURVE ( ( 1.000000000000000000, 0.9943317885200936290, 0.9943317885200936290, 1.000000000000000000 ) ) 
 REPRESENTATION_ITEM ( '' )  );
#78435 = CARTESIAN_POINT ( 'NONE',  ( 38.01892542963208399, -294.4532349136481457, -256.1390004877245019 ) ) ;
#78436 = CARTESIAN_POINT ( 'NONE',  ( -88.96040021043248203, -284.4523281539379695, -322.1951046163125625 ) ) ;
#78437 = CARTESIAN_POINT ( 'NONE',  ( 7.108535864358120016, -273.6996941862225867, -207.7099614268474284 ) ) ;
#78438 = CARTESIAN_POINT ( 'NONE',  ( -100.5920300223631330, -290.6252149670721678, -314.0956415870195997 ) ) ;
#78439 = CARTESIAN_POINT ( 'NONE',  ( -58.17029636089915812, -281.4579371267788588, -343.2612872958006847 ) ) ;
#78440 = CARTESIAN_POINT ( 'NONE',  ( -96.56532263054504028, -291.5470550255757303, -221.1644630560952578 ) ) ;
#78441 = CARTESIAN_POINT ( 'NONE',  ( 34.30572813080871697, -288.0721999624807381, -284.5230614834006246 ) ) ;
#78442 = CARTESIAN_POINT ( 'NONE',  ( 198.6357980679388220, 66.99333465236068719, 8.405329074384228605 ) ) ;
#78443 = CARTESIAN_POINT ( 'NONE',  ( 152.4536156746142410, 130.6065089285656313, -11.50000000000000000 ) ) ;
#78444 = CARTESIAN_POINT ( 'NONE',  ( -102.0040017515520532, -254.2189882600752640, -324.0990601116661765 ) ) ;
#78445 = CARTESIAN_POINT ( 'NONE',  ( 39.58706461736021254, -285.0523547857346784, -270.3937649182068981 ) ) ;
#78446 = EDGE_LOOP ( 'NONE', ( #55489, #78901, #79222, #44963 ) ) ;
#78447 = CARTESIAN_POINT ( 'NONE',  ( -51.87524831574088324, -278.7822462262372483, -198.4551371268680668 ) ) ;
#78448 = CARTESIAN_POINT ( 'NONE',  ( -26.99515829319025784, -273.8468557075844956, -194.0273421752997649 ) ) ;
#78449 = CARTESIAN_POINT ( 'NONE',  ( -40.55973565844323048, -279.0928470218787538, -345.1380091550995530 ) ) ;
#78450 = CARTESIAN_POINT ( 'NONE',  ( -81.45210018623211568, -220.0163494656852947, -350.2350564171413225 ) ) ;
#78451 = CARTESIAN_POINT ( 'NONE',  ( 38.28547164587251928, -280.2644431678554042, -281.2761160248477381 ) ) ;
#78452 = CARTESIAN_POINT ( 'NONE',  ( 1.946051286740130282, -280.5441342584977633, -333.8905056948813126 ) ) ;
#78453 = CARTESIAN_POINT ( 'NONE',  ( -96.57077276360662665, -298.9586978438368305, -222.7597422412592607 ) ) ;
#78454 = CARTESIAN_POINT ( 'NONE',  ( 26.28506580502691747, -293.5521184276691997, -234.3465108053729296 ) ) ;
#78455 = VERTEX_POINT ( 'NONE', #83485 ) ;
#78456 = CARTESIAN_POINT ( 'NONE',  ( -64.23658967843672940, -290.3785769373666312, -201.9522582982607446 ) ) ;
#78457 = CARTESIAN_POINT ( 'NONE',  ( -24.18521922064208240, -274.8672001459042349, -194.5427860907640820 ) ) ;
#78458 = CARTESIAN_POINT ( 'NONE',  ( -49.95600444325668832, -298.0533782744596465, -198.4592450505566319 ) ) ;
#78459 = ORIENTED_EDGE ( 'NONE', *, *, #70809, .F. ) ;
#78460 = SURFACE_SIDE_STYLE ('',( #69944 ) ) ;
#78461 = FACE_OUTER_BOUND ( 'NONE', #21123, .T. ) ;
#78462 = CYLINDRICAL_SURFACE ( 'NONE', #9500, 15.36528803885689420 ) ;
#78463 = CARTESIAN_POINT ( 'NONE',  ( 7.319803951760524008, -281.7567131493385091, -212.1627766860408713 ) ) ;
#78464 = CARTESIAN_POINT ( 'NONE',  ( -40.98256546537702150, -281.7670953062150829, -194.4487015466088451 ) ) ;
#78465 = CARTESIAN_POINT ( 'NONE',  ( -70.33161826673779160, -282.5567461330404058, -335.7591906940342028 ) ) ;
#78466 = CARTESIAN_POINT ( 'NONE',  ( -16.59889848231464526, -282.1834426315358542, -199.0827786510282635 ) ) ;
#78467 = CARTESIAN_POINT ( 'NONE',  ( 32.75173006594489067, -274.3310413565459385, -293.1123552247106545 ) ) ;
#78468 = DIRECTION ( 'NONE',  ( -1.000000000000000000, -0.000000000000000000, -0.000000000000000000 ) ) ;
#78469 = DIRECTION ( 'NONE',  ( -0.000000000000000000, -0.000000000000000000, -1.000000000000000000 ) ) ;
#78470 = CARTESIAN_POINT ( 'NONE',  ( -70.22261918109316525, -278.2772412999402150, -339.8233752520499706 ) ) ;
#78471 = VERTEX_POINT ( 'NONE', #4431 ) ;
#78472 = ORIENTED_EDGE ( 'NONE', *, *, #12553, .T. ) ;
#78473 = DIRECTION ( 'NONE',  ( 1.000000000000000000, 0.000000000000000000, 0.000000000000000000 ) ) ;
#78474 = CARTESIAN_POINT ( 'NONE',  ( -112.5131042436098028, -286.6081755116678664, -264.4039219905544655 ) ) ;
#78475 = CARTESIAN_POINT ( 'NONE',  ( 34.48095159329980675, -292.9327012606881908, -284.2933980217973726 ) ) ;
#78476 = CARTESIAN_POINT ( 'NONE',  ( 36.68403091330414156, -287.1625547339869513, -291.2301462495102555 ) ) ;
#78477 = CARTESIAN_POINT ( 'NONE',  ( -79.87352801256264456, -283.7083829713150749, -209.7257957932574470 ) ) ;
#78479 = CARTESIAN_POINT ( 'NONE',  ( -98.96665030307347877, -288.2305241148876576, -311.3761454465097245 ) ) ;
#78478 = CARTESIAN_POINT ( 'NONE',  ( -107.9148938436018170, -283.4026722296071057, -249.3326970086081360 ) ) ;
#78480 = VECTOR ( 'NONE', #89170, 1000.000000000000000 ) ;
#78481 = CARTESIAN_POINT ( 'NONE',  ( -13.38534140587776733, -283.9392215877786043, -339.7924165430966355 ) ) ;
#78482 = CARTESIAN_POINT ( 'NONE',  ( 29.48023259841298582, -273.1017076613928793, -236.3048417269511106 ) ) ;
#78483 = CARTESIAN_POINT ( 'NONE',  ( -109.2158436419237546, -283.2746638471179494, -245.0520700225553696 ) ) ;
#78484 = CARTESIAN_POINT ( 'NONE',  ( -99.94444018351963166, -297.9936164148192006, -311.7575081680385551 ) ) ;
#78485 = CARTESIAN_POINT ( 'NONE',  ( -65.17426539874490743, -283.6891656536947153, -200.5234046843481792 ) ) ;
#78486 = CARTESIAN_POINT ( 'NONE',  ( -110.5869072513067977, -279.5256099270086452, -267.9123145746898444 ) ) ;
#78487 = CARTESIAN_POINT ( 'NONE',  ( 25.58861575695056700, -288.9990628942610442, -229.2538951532462761 ) ) ;
#78488 = CARTESIAN_POINT ( 'NONE',  ( 196.7631351679105194, 292.9610677455149812, -7.940802731072580833 ) ) ;
#78489 = FACE_BOUND ( 'NONE', #34433, .T. ) ;
#78490 = CARTESIAN_POINT ( 'NONE',  ( 28.21393930871990463, -294.9747986362789902, -232.7875590099642409 ) ) ;
#78491 = CARTESIAN_POINT ( 'NONE',  ( -110.2274324427090164, -276.7790754386518302, -252.6786216133278913 ) ) ;
#78492 = CARTESIAN_POINT ( 'NONE',  ( -79.49726655252457874, -290.6958910110059264, -206.0552681249102989 ) ) ;
#78493 = CARTESIAN_POINT ( 'NONE',  ( -82.86917528380666909, -294.0862573907730848, -328.5097559344705473 ) ) ;
#78494 = CARTESIAN_POINT ( 'NONE',  ( -89.81402319500199383, -277.9775472419046878, -218.8312759855063518 ) ) ;
#78495 = CARTESIAN_POINT ( 'NONE',  ( -93.99410272325668814, -271.3057950871630624, -222.0525330141317966 ) ) ;
#78496 = CARTESIAN_POINT ( 'NONE',  ( -95.51494404148783701, -292.4953847904963595, -225.4487903644360358 ) ) ;
#78497 = CARTESIAN_POINT ( 'NONE',  ( 10.59707575819634329, -283.1948066931273615, -210.1954327657594490 ) ) ;
#78498 = CARTESIAN_POINT ( 'NONE',  ( -34.89642681218753495, -293.5018399251170536, -346.6285972431149958 ) ) ;
#78499 = CARTESIAN_POINT ( 'NONE',  ( -20.93185143611571064, -290.4381658120578891, -342.3135833948044251 ) ) ;
#78500 = CARTESIAN_POINT ( 'NONE',  ( 10.49843300442863026, -290.9418648339523088, -211.2570125170873609 ) ) ;
#78501 = CARTESIAN_POINT ( 'NONE',  ( -109.5130702540078431, -291.7884607331311599, -284.8014540948812510 ) ) ;
#78502 = DIRECTION ( 'NONE',  ( 0.7957555401921980742, 0.6056179655966482667, 0.000000000000000000 ) ) ;
#78503 = CARTESIAN_POINT ( 'NONE',  ( -62.86662375479551201, -292.5139747021296444, -201.7966957155939838 ) ) ;
#78504 = LINE ( 'NONE', #13642, #74764 ) ;
#78505 = CARTESIAN_POINT ( 'NONE',  ( -110.8554476210593549, -292.0287250168922810, -248.8265492972847142 ) ) ;
#78507 = CARTESIAN_POINT ( 'NONE',  ( 35.53467388016392903, -293.4856031940490766, -265.3163420777694910 ) ) ;
#78506 = CARTESIAN_POINT ( 'NONE',  ( 23.75853565688203872, -280.1701052742652109, -314.4870708245243804 ) ) ;
#78508 = CARTESIAN_POINT ( 'NONE',  ( 6.184255125203040215, -280.6253157357538157, -206.8434730381110285 ) ) ;
#78509 = CARTESIAN_POINT ( 'NONE',  ( 31.05641446366167102, -281.6742719479181005, -305.6802659299880816 ) ) ;
#78510 = CARTESIAN_POINT ( 'NONE',  ( 3.558444390643651811, -284.6021483064833433, -207.4947611173977009 ) ) ;
#78511 = CARTESIAN_POINT ( 'NONE',  ( 34.14258903376332199, -279.9519642562785862, -290.3826535109857332 ) ) ;
#78512 = ADVANCED_FACE ( 'NONE', ( #56040, #83970 ), #33311, .F. ) ;
#78513 = CARTESIAN_POINT ( 'NONE',  ( -72.64837932770662121, -283.5848898623127639, -204.1338314561199070 ) ) ;
#78514 = CARTESIAN_POINT ( 'NONE',  ( -147.0026986695707762, 31.65052214425332622, -21.50000000000000000 ) ) ;
#78515 = CARTESIAN_POINT ( 'NONE',  ( -59.08588370616837437, -278.2556155432524179, -197.2181194678722420 ) ) ;
#78516 = CARTESIAN_POINT ( 'NONE',  ( -65.75002696594327745, -284.6095061475264174, -199.1117810749830142 ) ) ;
#78517 = CARTESIAN_POINT ( 'NONE',  ( -29.98377074073661674, -274.9504960968371279, -197.5705787482251594 ) ) ;
#78518 = CARTESIAN_POINT ( 'NONE',  ( 195.0811277900482992, 39.56969527624787730, 15.19607843187435137 ) ) ;
#78519 = CARTESIAN_POINT ( 'NONE',  ( -6.959312775711741672, -294.0577942450718183, -203.1052561125959528 ) ) ;
#78520 = CARTESIAN_POINT ( 'NONE',  ( 15.60557607635313637, -276.2090812642587707, -215.2685392229145975 ) ) ;
#78521 = CARTESIAN_POINT ( 'NONE',  ( -101.8775896937261365, -277.7536353275127112, -304.5255211627210770 ) ) ;
#78522 = CARTESIAN_POINT ( 'NONE',  ( -67.01740533659108223, -291.8404474295331283, -199.3093585047412546 ) ) ;
#78523 = CARTESIAN_POINT ( 'NONE',  ( -3.021931480836714368, -278.5818066254904579, -203.0304868062031858 ) ) ;
#78524 = CARTESIAN_POINT ( 'NONE',  ( -81.92865648480223228, -291.2961625524351348, -207.5837070186526319 ) ) ;
#78525 = CARTESIAN_POINT ( 'NONE',  ( -91.84026347515181499, -290.3089997870071102, -221.4208454254958269 ) ) ;
#78526 = CARTESIAN_POINT ( 'NONE',  ( -19.78094129014038316, -292.8263582765110868, -343.3297327393677278 ) ) ;
#78527 = ORIENTED_EDGE ( 'NONE', *, *, #70157, .F. ) ;
#78528 = CARTESIAN_POINT ( 'NONE',  ( 151.0356227161011020, 20.07892719423917427, 6.469110745572608678 ) ) ;
#78529 = CARTESIAN_POINT ( 'NONE',  ( -0.05415658918259873278, -292.0705723706474259, -207.5309696578219700 ) ) ;
#78530 = DIRECTION ( 'NONE',  ( 0.000000000000000000, 1.000000000000000000, 0.000000000000000000 ) ) ;
#78531 = CARTESIAN_POINT ( 'NONE',  ( -53.35057174420112602, -274.7666405000204009, -340.3538533559490702 ) ) ;
#78532 = CARTESIAN_POINT ( 'NONE',  ( -114.0739551433859162, -295.6563977908514289, -266.7344052728408883 ) ) ;
#78533 = CARTESIAN_POINT ( 'NONE',  ( -93.56876060867189437, -286.5789179362483878, -218.4007432970724949 ) ) ;
#78534 = CARTESIAN_POINT ( 'NONE',  ( -7.014568142378860394, -286.2948331066494916, -203.9450938034151477 ) ) ;
#78535 = CARTESIAN_POINT ( 'NONE',  ( 36.06705071093982440, -276.9804742235096455, -263.3355728474290345 ) ) ;
#78536 = CARTESIAN_POINT ( 'NONE',  ( -91.62022021752939338, -293.8498222468210770, -321.6770628179526739 ) ) ;
#78537 = CARTESIAN_POINT ( 'NONE',  ( -71.37710732562911176, -297.2680960404190387, -336.0986929038641051 ) ) ;
#78538 = CARTESIAN_POINT ( 'NONE',  ( -35.12091352673736111, -275.8185683224580771, -343.7245871800645887 ) ) ;
#78539 = ORIENTED_EDGE ( 'NONE', *, *, #87659, .T. ) ;
#78540 = FACE_OUTER_BOUND ( 'NONE', #68326, .T. ) ;
#78541 = CARTESIAN_POINT ( 'NONE',  ( -111.5727549941722856, -295.9634691978630485, -290.7448071737853184 ) ) ;
#78542 = CARTESIAN_POINT ( 'NONE',  ( 31.27990846049819140, -289.0910839383534494, -241.3765798627018455 ) ) ;
#78543 = FACE_OUTER_BOUND ( 'NONE', #60076, .T. ) ;
#78544 = CARTESIAN_POINT ( 'NONE',  ( 30.58297040466815275, -288.5662305582638396, -297.5186336925636965 ) ) ;
#78545 = ORIENTED_EDGE ( 'NONE', *, *, #45139, .F. ) ;
#78546 = CARTESIAN_POINT ( 'NONE',  ( -95.71904859990847569, -278.2855413540873428, -220.4921068311262218 ) ) ;
#78547 = CARTESIAN_POINT ( 'NONE',  ( -68.17768083229086074, -296.0980213357907473, -340.8058131758902505 ) ) ;
#78548 = CARTESIAN_POINT ( 'NONE',  ( -56.99372731946348836, -287.4424358860316033, -343.5870827309071842 ) ) ;
#78549 = AXIS2_PLACEMENT_3D ( 'NONE', #84078, #77456, #12119 ) ;
#78550 = CARTESIAN_POINT ( 'NONE',  ( -114.3168621293517475, -296.8948668174932664, -269.6069785302972264 ) ) ;
#78551 = CARTESIAN_POINT ( 'NONE',  ( 27.50336777494408125, -293.4289877681877101, -236.7872493443745725 ) ) ;
#78552 = FACE_OUTER_BOUND ( 'NONE', #21258, .T. ) ;
#78553 = SURFACE_SIDE_STYLE ('',( #63903 ) ) ;
#78554 = CARTESIAN_POINT ( 'NONE',  ( 199.4767649826798674, 41.62711076580291092, 9.000000000000001776 ) ) ;
#78555 = CARTESIAN_POINT ( 'NONE',  ( -45.92834899839301244, -290.6791317570819615, -346.2357759003624551 ) ) ;
#78556 = CARTESIAN_POINT ( 'NONE',  ( 25.22466315766300227, -278.6948066931273047, -320.2154176792147382 ) ) ;
#78557 = CARTESIAN_POINT ( 'NONE',  ( -111.9849665934233087, -278.1329108403559758, -251.8221090231298547 ) ) ;
#78558 = CARTESIAN_POINT ( 'NONE',  ( -74.69023864502166532, -285.5501706050789608, -335.2670175365548175 ) ) ;
#78559 = CARTESIAN_POINT ( 'NONE',  ( 2.449775781553417353, -285.1492393251827480, -205.1288810338072324 ) ) ;
#78560 = CARTESIAN_POINT ( 'NONE',  ( -53.74925661647637298, -287.3441958255147028, -342.9703893254933860 ) ) ;
#78561 = CARTESIAN_POINT ( 'NONE',  ( 19.90280020763823643, -278.0943303123561918, -320.0131364649568582 ) ) ;
#78562 = ORIENTED_EDGE ( 'NONE', *, *, #80612, .T. ) ;
#78564 = CARTESIAN_POINT ( 'NONE',  ( -57.13285038070998922, -279.1385548112180004, -199.9892270064146373 ) ) ;
#78563 = CARTESIAN_POINT ( 'NONE',  ( -110.1586453576392586, -278.6203065851875067, -265.1946407073208434 ) ) ;
#78565 = CARTESIAN_POINT ( 'NONE',  ( 26.66497348911988041, -276.0740402482012428, -228.1161390849143231 ) ) ;
#78566 = CARTESIAN_POINT ( 'NONE',  ( -73.56426780823311162, -278.3773725683269049, -202.8485842138100850 ) ) ;
#78567 = CARTESIAN_POINT ( 'NONE',  ( 183.2361720774044613, 262.7496117309314059, -151.9803302442668951 ) ) ;
#78568 = CARTESIAN_POINT ( 'NONE',  ( -35.54135695043370902, -275.0154406052131435, -193.6044353622344261 ) ) ;
#78569 = CARTESIAN_POINT ( 'NONE',  ( -75.50150854586291871, -298.9792230066044567, -204.1004214932385707 ) ) ;
#78570 = CARTESIAN_POINT ( 'NONE',  ( 10.64812456238590066, -284.9090924074130271, -330.4860931364851808 ) ) ;
#78571 = ORIENTED_EDGE ( 'NONE', *, *, #32103, .T. ) ;
#78572 = CARTESIAN_POINT ( 'NONE',  ( 208.4306832106271088, -74.55766379199613425, 0.000000000000000000 ) ) ;
#78573 = CARTESIAN_POINT ( 'NONE',  ( -44.06636157217130290, -287.0448043071465918, -197.3610837218801635 ) ) ;
#78574 = CARTESIAN_POINT ( 'NONE',  ( -64.21013188906239577, -287.4665165483907003, -199.2692805856398479 ) ) ;
#78575 = CARTESIAN_POINT ( 'NONE',  ( 3.664936194092168531, -287.8330935431459352, -330.9394921323816448 ) ) ;
#78576 = CARTESIAN_POINT ( 'NONE',  ( -71.71687635028065699, -283.0018946269506728, -339.1933354625257948 ) ) ;
#78577 = CARTESIAN_POINT ( 'NONE',  ( -30.16452048410592823, -278.5441904678078799, -196.8600337954603390 ) ) ;
#78578 = CARTESIAN_POINT ( 'NONE',  ( -55.07396886762415278, -287.6822672812605788, -198.2216487374095095 ) ) ;
#78579 = CARTESIAN_POINT ( 'NONE',  ( 36.21306841039208990, -279.9729961450294695, -265.8440640564992918 ) ) ;
#78580 = CARTESIAN_POINT ( 'NONE',  ( -26.93524262507619937, -278.2322350932514041, -343.1137751119311474 ) ) ;
#78581 = CARTESIAN_POINT ( 'NONE',  ( 34.76893079480420568, -276.2033946081338058, -282.4162377614863431 ) ) ;
#78582 = CARTESIAN_POINT ( 'NONE',  ( 18.34556971237548595, -287.0691897059519988, -322.9627975774164383 ) ) ;
#78583 = CARTESIAN_POINT ( 'NONE',  ( 24.13207741950450469, -282.9698058218727965, -316.4602882031379636 ) ) ;
#78584 = CARTESIAN_POINT ( 'NONE',  ( -69.15528092880882127, -283.9518412852310121, -340.4285211352772649 ) ) ;
#78585 = CARTESIAN_POINT ( 'NONE',  ( 0.3981328123779520611, -280.7364921607378960, -207.8149652685710578 ) ) ;
#78586 = ORIENTED_EDGE ( 'NONE', *, *, #41597, .F. ) ;
#78587 = ORIENTED_EDGE ( 'NONE', *, *, #49649, .F. ) ;
#78588 = CARTESIAN_POINT ( 'NONE',  ( 208.0849289532862372, 28.61657807523931396, 11.99999999999999822 ) ) ;
#78589 = CARTESIAN_POINT ( 'NONE',  ( -7.386134101901441262, -290.5239463344674959, -339.9665793633228077 ) ) ;
#78590 = CARTESIAN_POINT ( 'NONE',  ( -19.48551063167111508, -290.9618655087073193, -195.9127275134494255 ) ) ;
#78591 = CARTESIAN_POINT ( 'NONE',  ( -38.07272056362097601, -273.1015159515761184, -197.1294714216506350 ) ) ;
#78592 = CARTESIAN_POINT ( 'NONE',  ( 37.68264218367406215, -293.1127726809691012, -287.2924193020761550 ) ) ;
#78593 = CARTESIAN_POINT ( 'NONE',  ( -109.9566051638406066, -289.1999716456214173, -257.5090153100776433 ) ) ;
#78594 = CARTESIAN_POINT ( 'NONE',  ( 20.99526049813713513, -291.1585681003528521, -224.7909161590257554 ) ) ;
#78595 = CARTESIAN_POINT ( 'NONE',  ( 22.29322579196597331, -289.3521155635723403, -313.1490381937547340 ) ) ;
#78596 = CARTESIAN_POINT ( 'NONE',  ( 31.95455697924148097, -289.6233781216988064, -236.9535640164627637 ) ) ;
#78597 = CARTESIAN_POINT ( 'NONE',  ( -67.23275674053692796, -291.4442404964923981, -339.1472022281287195 ) ) ;
#78598 = CARTESIAN_POINT ( 'NONE',  ( -85.32271174349304488, -289.3912532321893423, -212.4329379963150757 ) ) ;
#78599 = CARTESIAN_POINT ( 'NONE',  ( -3.929301603794604247, -294.4929273803697356, -203.2008337922928547 ) ) ;
#78600 = CARTESIAN_POINT ( 'NONE',  ( -96.77276472027713794, -286.0901515181005266, -227.5453627034338524 ) ) ;
#78601 = CARTESIAN_POINT ( 'NONE',  ( 5.431568940963765080, -294.6298804038204366, -208.5511197839680335 ) ) ;
#78602 = CARTESIAN_POINT ( 'NONE',  ( 201.2509219215139922, 65.09645894978945080, -5.329070518200752656E-14 ) ) ;
#78603 = FACE_OUTER_BOUND ( 'NONE', #50973, .T. ) ;
#78604 = CARTESIAN_POINT ( 'NONE',  ( 95.99055701654010875, -301.6291247887334634, -194.7578621600179929 ) ) ;
#78605 = CARTESIAN_POINT ( 'NONE',  ( -43.11151744647708028, -281.1247050258659783, -345.1903128854513056 ) ) ;
#78606 = CARTESIAN_POINT ( 'NONE',  ( -113.0465804601180935, -295.5807438471168211, -283.8122924865294294 ) ) ;
#78607 = CARTESIAN_POINT ( 'NONE',  ( -3.623301486488966994, -272.7432604246999404, -204.4602919311154778 ) ) ;
#78608 = CARTESIAN_POINT ( 'NONE',  ( -48.85420396401065091, -275.2796166150836825, -343.9579073213237166 ) ) ;
#78609 = CARTESIAN_POINT ( 'NONE',  ( -65.77889535242896102, -298.9873643423164822, -202.5926193527098178 ) ) ;
#78610 = CARTESIAN_POINT ( 'NONE',  ( -109.3595167034088291, -298.1761501539551205, -255.1740218110153364 ) ) ;
#78611 = EDGE_CURVE ( 'NONE', #88883, #62986, #39972, .T. ) ;
#78612 = CYLINDRICAL_SURFACE ( 'NONE', #21781, 0.5000000000000004441 ) ;
#78613 = CARTESIAN_POINT ( 'NONE',  ( -97.30988669899636534, -296.7718875031885659, -312.2707627741876308 ) ) ;
#78614 = CIRCLE ( 'NONE', #37753, 0.5000000000000004441 ) ;
#78615 = CARTESIAN_POINT ( 'NONE',  ( 208.4306832106271088, -134.2391364535880882, 0.000000000000000000 ) ) ;
#78617 = CARTESIAN_POINT ( 'NONE',  ( -69.25753617374633109, -297.6201171569708208, -204.7076381851705378 ) ) ;
#78616 = CARTESIAN_POINT ( 'NONE',  ( 0.7132904829745017050, -284.5769898918645140, -205.3059286568074242 ) ) ;
#78618 = CARTESIAN_POINT ( 'NONE',  ( 23.86143494046273261, -286.9289598736797871, -223.6150281175455063 ) ) ;
#78619 = VECTOR ( 'NONE', #26186, 1000.000000000000000 ) ;
#78620 = CARTESIAN_POINT ( 'NONE',  ( 36.36392197253956482, -287.4982128966321966, -292.6155733824336380 ) ) ;
#78621 = CARTESIAN_POINT ( 'NONE',  ( -112.1451423713069175, -298.6483663263388735, -261.2588198902338945 ) ) ;
#78622 = CARTESIAN_POINT ( 'NONE',  ( -14.25725425521069312, -290.3520520566124787, -199.1772940938574834 ) ) ;
#78623 = CARTESIAN_POINT ( 'NONE',  ( -99.29160707250838414, -278.3545621805811265, -224.8815966733992582 ) ) ;
#78624 = CARTESIAN_POINT ( 'NONE',  ( 31.98288692825982693, -284.6237833571632905, -237.0123917617630980 ) ) ;
#78625 = DIRECTION ( 'NONE',  ( 0.000000000000000000, -1.000000000000000000, 0.000000000000000000 ) ) ;
#78626 = CARTESIAN_POINT ( 'NONE',  ( 34.67077106938914710, -286.5340918236167909, -284.6152590400130293 ) ) ;
#78627 = DIRECTION ( 'NONE',  ( -0.000000000000000000, 1.000000000000000000, -0.000000000000000000 ) ) ;
#78628 = CARTESIAN_POINT ( 'NONE',  ( -72.12226116782585450, -287.5119327589609384, -336.8234529237187758 ) ) ;
#78629 = CARTESIAN_POINT ( 'NONE',  ( -106.0698082391928949, -274.4259209203800651, -243.6278728434055836 ) ) ;
#78630 = CARTESIAN_POINT ( 'NONE',  ( 27.34280263180543713, -282.4395665715327937, -229.5861874555359350 ) ) ;
#78632 = CARTESIAN_POINT ( 'NONE',  ( 34.70355992560354252, -281.7073886536329610, -282.1288919350506603 ) ) ;
#78631 = CARTESIAN_POINT ( 'NONE',  ( -85.36686949053191142, -293.7322676185532941, -328.4299556451662170 ) ) ;
#78633 = CARTESIAN_POINT ( 'NONE',  ( -111.5914549869816170, -296.4633496286864442, -290.7565563919953888 ) ) ;
#78634 = CARTESIAN_POINT ( 'NONE',  ( -35.81677508070058025, -299.5917038824570113, -196.6673763113564348 ) ) ;
#78635 = CARTESIAN_POINT ( 'NONE',  ( -33.77045976182287745, -284.1766139314307793, -194.8855560963399398 ) ) ;
#78636 = EDGE_CURVE ( 'NONE', #48115, #73985, #84893, .T. ) ;
#78637 = CARTESIAN_POINT ( 'NONE',  ( -5.808665093568579962, -282.4668990852031811, -202.3121036303590472 ) ) ;
#78638 = CARTESIAN_POINT ( 'NONE',  ( -104.9749334234064690, -295.9864081889618888, -242.2692294463513178 ) ) ;
#78639 = VERTEX_POINT ( 'NONE', #34724 ) ;
#78640 = CARTESIAN_POINT ( 'NONE',  ( 212.3569123273291268, -147.7221692137691775, -10.75739200365177695 ) ) ;
#78641 = CARTESIAN_POINT ( 'NONE',  ( 22.33984531576784605, -284.1478982837167564, -315.2148254123349034 ) ) ;
#78642 = DIRECTION ( 'NONE',  ( 1.000000000000000000, 0.000000000000000000, 0.000000000000000000 ) ) ;
#78643 = CARTESIAN_POINT ( 'NONE',  ( 10.64812456238590777, -284.1952119285918457, -210.2361428286349110 ) ) ;
#78644 = CARTESIAN_POINT ( 'NONE',  ( 37.78966514558979384, -274.5466797099522864, -254.1918373951729393 ) ) ;
#78645 = CARTESIAN_POINT ( 'NONE',  ( 20.18420522177757093, -292.7517713517248694, -225.3990266266529829 ) ) ;
#78646 = CARTESIAN_POINT ( 'NONE',  ( 17.56660933272043934, -282.3756588339055611, -221.2104790707151665 ) ) ;
#78647 = CARTESIAN_POINT ( 'NONE',  ( 36.15253068161145933, -277.2398576587238495, -277.0721873236410602 ) ) ;
#78648 = CARTESIAN_POINT ( 'NONE',  ( -47.16251540386964791, -284.5998663077435822, -346.1381453669321786 ) ) ;
#78649 = CARTESIAN_POINT ( 'NONE',  ( 31.44779713559346135, -280.0058057405393015, -244.6196081082668172 ) ) ;
#78650 = CARTESIAN_POINT ( 'NONE',  ( -90.48549324443042963, -279.8044037137273676, -323.3568377834724856 ) ) ;
#78651 = CARTESIAN_POINT ( 'NONE',  ( -3.410510378925430963, -298.4659870783543738, -193.3611102151625971 ) ) ;
#78652 = CARTESIAN_POINT ( 'NONE',  ( 37.94583847598392623, -275.1827293055648624, -254.1498913486779827 ) ) ;
#78653 = CARTESIAN_POINT ( 'NONE',  ( 9.146153794915321100, -296.3287442250542654, -328.5668153844217159 ) ) ;
#78654 = FACE_OUTER_BOUND ( 'NONE', #27776, .T. ) ;
#78655 = CARTESIAN_POINT ( 'NONE',  ( 73.43068321062709458, -178.2391364535880882, 4.999999999999990230 ) ) ;
#78656 = CARTESIAN_POINT ( 'NONE',  ( -112.7168167278714606, -294.5941923707146657, -278.0355740972362355 ) ) ;
#78657 = CARTESIAN_POINT ( 'NONE',  ( -48.87897666851846168, -273.4090085141683630, -198.1650496772829513 ) ) ;
#78658 = CARTESIAN_POINT ( 'NONE',  ( 24.33738336087547438, -295.6741859404183970, -315.3097242076204338 ) ) ;
#78659 = CARTESIAN_POINT ( 'NONE',  ( -5.946334098559480807, -295.8536164491032423, -340.2348591996635037 ) ) ;
#78660 = CARTESIAN_POINT ( 'NONE',  ( -10.03188028773695706, -290.6950696752558656, -340.0888085637946006 ) ) ;
#78661 = CARTESIAN_POINT ( 'NONE',  ( -109.9571255299280779, -276.3185844365544312, -288.4979446519641328 ) ) ;
#78662 = CARTESIAN_POINT ( 'NONE',  ( 16.65900263320595442, -278.1965477615525515, -321.5981973212766434 ) ) ;
#78663 = CARTESIAN_POINT ( 'NONE',  ( -85.42656270510117622, -293.8022973010352530, -327.2545164187904447 ) ) ;
#78664 = CARTESIAN_POINT ( 'NONE',  ( 28.20590577343461547, -282.9103457800706565, -232.3635280711608004 ) ) ;
#78665 = CARTESIAN_POINT ( 'NONE',  ( -94.35379629054345685, -284.1217069907488053, -224.2560132696502819 ) ) ;
#78666 = CARTESIAN_POINT ( 'NONE',  ( 195.6954042328585501, 277.0390073305854912, -125.2964528022664723 ) ) ;
#78667 = ORIENTED_EDGE ( 'NONE', *, *, #73884, .F. ) ;
#78668 = CARTESIAN_POINT ( 'NONE',  ( -72.38043005085809511, -285.2416333511620223, -206.2815022803524698 ) ) ;
#78669 = CARTESIAN_POINT ( 'NONE',  ( 37.67940328304122488, -282.4311732373903396, -254.3821097311873700 ) ) ;
#78670 = CARTESIAN_POINT ( 'NONE',  ( -68.32601142235476743, -284.4490657676504384, -200.2898321480615778 ) ) ;
#78671 = CARTESIAN_POINT ( 'NONE',  ( -110.3297187660448344, -279.7954009736042735, -246.4106218731513138 ) ) ;
#78672 = CARTESIAN_POINT ( 'NONE',  ( -64.82710012619783413, -278.9246673186498242, -341.6015836978963875 ) ) ;
#78673 = CIRCLE ( 'NONE', #56035, 1.999999999999992673 ) ;
#78674 = CARTESIAN_POINT ( 'NONE',  ( 27.33386217378598815, -273.4809262143061233, -301.5434626090942629 ) ) ;
#78675 = CARTESIAN_POINT ( 'NONE',  ( -103.3473159737818605, -256.7681506039956503, -326.7728887287452153 ) ) ;
#78676 = ORIENTED_EDGE ( 'NONE', *, *, #60993, .F. ) ;
#78677 = CARTESIAN_POINT ( 'NONE',  ( -108.0467196094137705, -274.8703032242514155, -245.8493117315155985 ) ) ;
#78678 = AXIS2_PLACEMENT_3D ( 'NONE', #72010, #7127, #27980 ) ;
#78679 = CARTESIAN_POINT ( 'NONE',  ( -54.85476745283906297, -277.8461547975692838, -197.7464701284746695 ) ) ;
#78680 = CARTESIAN_POINT ( 'NONE',  ( -66.64564125943893202, -293.4336512280216880, -200.2522522877451081 ) ) ;
#78681 = CARTESIAN_POINT ( 'NONE',  ( 18.55988834123604647, -292.2324456558302472, -223.2558627014914805 ) ) ;
#78682 = CARTESIAN_POINT ( 'NONE',  ( -102.2527158509085865, -289.5168496268728404, -311.7639759952966187 ) ) ;
#78683 = DIRECTION ( 'NONE',  ( 1.000000000000000000, 0.000000000000000000, 0.000000000000000000 ) ) ;
#78685 = CARTESIAN_POINT ( 'NONE',  ( -71.53093684184175061, -283.9924688108109194, -204.9582395309947742 ) ) ;
#78684 = CARTESIAN_POINT ( 'NONE',  ( -27.83924711164970489, -293.5086117438322049, -346.2316098671840905 ) ) ;
#78686 = CARTESIAN_POINT ( 'NONE',  ( -5.533500342538035355, -294.3354709628830506, -203.2717455720560054 ) ) ;
#78687 = CARTESIAN_POINT ( 'NONE',  ( -0.9936351311795564856, -283.8739487287514294, -334.2364782509478687 ) ) ;
#78688 = ORIENTED_EDGE ( 'NONE', *, *, #30078, .F. ) ;
#78689 = CARTESIAN_POINT ( 'NONE',  ( -92.65090200224467765, -292.2250305152729197, -217.0528558285718077 ) ) ;
#78690 = CARTESIAN_POINT ( 'NONE',  ( -19.52561274059026886, -280.7797560442970735, -199.4527658493097704 ) ) ;
#78691 = CARTESIAN_POINT ( 'NONE',  ( 37.96406132851063120, -292.5244393928860518, -284.4694049368013680 ) ) ;
#78692 = CARTESIAN_POINT ( 'NONE',  ( 35.79719336610538960, -288.6518225984476658, -293.9166073397963146 ) ) ;
#78693 = CARTESIAN_POINT ( 'NONE',  ( -36.08155718505700804, -289.5291274786713416, -347.3023591951497338 ) ) ;
#78694 = CARTESIAN_POINT ( 'NONE',  ( 32.66936623805344908, -287.4447295021695936, -249.6421478981004327 ) ) ;
#78695 = ORIENTED_EDGE ( 'NONE', *, *, #88464, .T. ) ;
#78696 = CARTESIAN_POINT ( 'NONE',  ( 195.2251806849246805, 24.84528228517684667, 13.27436667035662232 ) ) ;
#78697 = CARTESIAN_POINT ( 'NONE',  ( 18.63338050518334299, -296.1187078977703209, -321.4972915332950834 ) ) ;
#78698 = CARTESIAN_POINT ( 'NONE',  ( -80.33397150388192642, -296.1681898797301642, -207.0126538561590621 ) ) ;
#78699 = CARTESIAN_POINT ( 'NONE',  ( -108.4032997511616827, -277.3773216427051125, -288.1232286798413611 ) ) ;
#78700 = CARTESIAN_POINT ( 'NONE',  ( -110.0416630628048722, -272.3775680725170787, -245.1769504869315597 ) ) ;
#78701 = CARTESIAN_POINT ( 'NONE',  ( -55.99734827041613983, -293.7765201471142404, -341.7068815860121163 ) ) ;
#78702 = CARTESIAN_POINT ( 'NONE',  ( 23.09551691191135347, -276.7238227006940861, -227.6154611429739134 ) ) ;
#78703 = CARTESIAN_POINT ( 'NONE',  ( -104.3093292422995120, -271.1177815792476054, -238.3267282077571849 ) ) ;
#78704 = CARTESIAN_POINT ( 'NONE',  ( 35.60333806118509870, -294.8698147224025092, -278.9418042655849490 ) ) ;
#78705 = CARTESIAN_POINT ( 'NONE',  ( -61.10040065245200225, -296.4475079153704087, -339.7672783022074441 ) ) ;
#78706 = CARTESIAN_POINT ( 'NONE',  ( -43.47537869213319084, -255.2745817066169423, -444.3374207175232868 ) ) ;
#78707 = CARTESIAN_POINT ( 'NONE',  ( -92.36522679112401590, -293.8367803855977058, -321.5898463016061442 ) ) ;
#78708 = CARTESIAN_POINT ( 'NONE',  ( -114.0206494304582776, -273.4265779991619070, -264.6484528472711872 ) ) ;
#78709 = CARTESIAN_POINT ( 'NONE',  ( 8.331570025339173569, -286.9875060328600398, -328.0614412823993007 ) ) ;
#78710 = CARTESIAN_POINT ( 'NONE',  ( 156.4947056272797852, 21.00000000000000000, 15.00000000000000000 ) ) ;
#78711 = CARTESIAN_POINT ( 'NONE',  ( -78.81366317373289121, -274.0015311204903128, -205.5567725705720079 ) ) ;
#78712 = CARTESIAN_POINT ( 'NONE',  ( -109.0672412583592461, -297.0669115010791757, -256.6001894047518590 ) ) ;
#78713 = CARTESIAN_POINT ( 'NONE',  ( -9.492924349842045473, -282.3941804789812977, -200.3407460104639881 ) ) ;
#78714 = CARTESIAN_POINT ( 'NONE',  ( 22.50013162796342669, -279.5944832560663826, -222.6721243455703814 ) ) ;
#78715 = ORIENTED_EDGE ( 'NONE', *, *, #39228, .T. ) ;
#78716 = CARTESIAN_POINT ( 'NONE',  ( -52.90510366941208531, -282.5950364036022506, -345.7222005599020349 ) ) ;
#78717 = CARTESIAN_POINT ( 'NONE',  ( 35.10214353962329170, -275.2284586123627719, -296.3095383389904214 ) ) ;
#78718 = CARTESIAN_POINT ( 'NONE',  ( -7.827833069119636278, -278.8323497611644370, -200.0947582849837829 ) ) ;
#78719 = CARTESIAN_POINT ( 'NONE',  ( -3.199561070060736867, -278.5018131531216454, -203.3815033874062692 ) ) ;
#78720 = ADVANCED_FACE ( 'NONE', ( #63640 ), #438, .F. ) ;
#78721 = CARTESIAN_POINT ( 'NONE',  ( -6.263764471634402753, -273.0434147924614194, -203.6562693263288963 ) ) ;
#78722 = CARTESIAN_POINT ( 'NONE',  ( 36.27544832617159898, -277.3673985747126380, -255.9597078771451208 ) ) ;
#78723 = CARTESIAN_POINT ( 'NONE',  ( 113.5000000000000568, -212.3147208684173677, -516.1047766808072765 ) ) ;
#78724 = CARTESIAN_POINT ( 'NONE',  ( -4.025340937891983550, -290.5093937367022363, -202.7567480277062657 ) ) ;
#78725 = CARTESIAN_POINT ( 'NONE',  ( -96.57886909800195951, -291.2138277587417861, -221.1476754266053604 ) ) ;
#78726 = CARTESIAN_POINT ( 'NONE',  ( -31.56512130915528047, -278.9796750362481248, -345.3568645040633669 ) ) ;
#78727 = CARTESIAN_POINT ( 'NONE',  ( -5.661632698341396264, -272.4686196240838854, -202.3804296913274072 ) ) ;
#78728 = CARTESIAN_POINT ( 'NONE',  ( -55.80257052418232888, -229.5268262511776527, 22.50000000000000000 ) ) ;
#78729 =( LENGTH_UNIT ( ) NAMED_UNIT ( * ) SI_UNIT ( .MILLI., .METRE. ) );
#78730 = CARTESIAN_POINT ( 'NONE',  ( -33.23510068027243136, -284.1035756449785481, -195.4232692572382746 ) ) ;
#78731 = CARTESIAN_POINT ( 'NONE',  ( 170.8178014930282700, 8.542400036368780647, -9.000000000000001776 ) ) ;
#78732 = CARTESIAN_POINT ( 'NONE',  ( -42.43250118660234449, -293.9127061532680045, -343.5814310777573155 ) ) ;
#78733 = CARTESIAN_POINT ( 'NONE',  ( 32.55457183249233566, -286.0191731522660348, -295.3686497511686184 ) ) ;
#78734 = LINE ( 'NONE', #85819, #29076 ) ;
#78735 = LINE ( 'NONE', #35172, #41256 ) ;
#78736 = CARTESIAN_POINT ( 'NONE',  ( 7.231656944940937137, -292.4450679508937014, -330.7434545395724399 ) ) ;
#78737 = CARTESIAN_POINT ( 'NONE',  ( -110.8290274778271822, -282.7721886963385032, -290.9115552692520055 ) ) ;
#78738 = CARTESIAN_POINT ( 'NONE',  ( -91.90184341310330751, -280.8571202821070756, -220.6657340871182384 ) ) ;
#78739 = CARTESIAN_POINT ( 'NONE',  ( -80.72602444033948643, -286.6833048952634613, -207.1638184653175472 ) ) ;
#78740 = CARTESIAN_POINT ( 'NONE',  ( 34.96037288133486953, -287.6861962870319189, -280.5223947339177357 ) ) ;
#78741 = CARTESIAN_POINT ( 'NONE',  ( -35.08149971586499305, -278.4484910029231628, -343.9156311861027007 ) ) ;
#78742 = CARTESIAN_POINT ( 'NONE',  ( -93.22013547409262912, -280.0248114800314170, -223.1168271366433942 ) ) ;
#78743 = EDGE_CURVE ( 'NONE', #59134, #23299, #29952, .T. ) ;
#78744 = CARTESIAN_POINT ( 'NONE',  ( 4.250369349333530167, -288.5892934095487590, -207.4618369971614413 ) ) ;
#78745 = AXIS2_PLACEMENT_3D ( 'NONE', #77362, #28125, #62721 ) ;
#78746 = EDGE_LOOP ( 'NONE', ( #33494, #55559, #51729, #61798 ) ) ;
#78747 = CARTESIAN_POINT ( 'NONE',  ( -102.3152563265819168, -296.9270779397500064, -229.0399732813357332 ) ) ;
#78749 = CARTESIAN_POINT ( 'NONE',  ( 29.71619581586000791, -289.9663765324426663, -303.1496127807340599 ) ) ;
#78748 = AXIS2_PLACEMENT_3D ( 'NONE', #90682, #80709, #72232 ) ;
#78750 = DIRECTION ( 'NONE',  ( 0.000000000000000000, 0.000000000000000000, 1.000000000000000000 ) ) ;
#78751 = CARTESIAN_POINT ( 'NONE',  ( 25.18497378105907814, -283.4090924074130839, -220.4570493818173702 ) ) ;
#78752 = ORIENTED_EDGE ( 'NONE', *, *, #90146, .F. ) ;
#78753 = CARTESIAN_POINT ( 'NONE',  ( -24.44841109318233308, -272.2160532570519536, -196.2556116564043123 ) ) ;
#78754 = CARTESIAN_POINT ( 'NONE',  ( 21.60350459938456780, -291.2967998708135156, -222.0713337848848994 ) ) ;
#78755 = CARTESIAN_POINT ( 'NONE',  ( -86.53603409076498565, -295.2656914877719032, -324.3787627616300142 ) ) ;
#78756 = CARTESIAN_POINT ( 'NONE',  ( 18.28696722790054352, -288.3896727451667630, -222.0272879884981592 ) ) ;
#78757 = CARTESIAN_POINT ( 'NONE',  ( 34.93475296403097730, -283.5196923001047935, -286.3012668201505448 ) ) ;
#78758 = CARTESIAN_POINT ( 'NONE',  ( -69.09575587127618235, -290.8869152356656969, -339.8756900397437448 ) ) ;
#78759 = CARTESIAN_POINT ( 'NONE',  ( -112.8705217766124775, -291.7138354235013935, -282.5551892247387968 ) ) ;
#78760 = CARTESIAN_POINT ( 'NONE',  ( -112.3170219535684424, -286.5087614312796518, -273.7533198087757569 ) ) ;
#78761 = CARTESIAN_POINT ( 'NONE',  ( -110.6660150258689583, -278.4213414652741108, -294.0390468988787802 ) ) ;
#78762 = CARTESIAN_POINT ( 'NONE',  ( -8.952198915101265086, -292.7637122573524380, -340.4404616936378716 ) ) ;
#78763 = CARTESIAN_POINT ( 'NONE',  ( -8.859138326056228863, -280.2479547456487126, -198.8227109713326115 ) ) ;
#78764 = CARTESIAN_POINT ( 'NONE',  ( -103.1360020772057027, -274.8739466727927834, -235.8698452527687266 ) ) ;
#78765 = EDGE_CURVE ( 'NONE', #64529, #50851, #88127, .T. ) ;
#78766 = CARTESIAN_POINT ( 'NONE',  ( -20.19161114001083490, -291.3376638359845856, -345.3538533559490702 ) ) ;
#78767 = CARTESIAN_POINT ( 'NONE',  ( 25.32177333006835340, -273.2169968841843684, -227.3582471649257570 ) ) ;
#78768 = DIRECTION ( 'NONE',  ( 0.9998346970812741485, 0.000000000000000000, -0.01818181818182024179 ) ) ;
#78769 = CARTESIAN_POINT ( 'NONE',  ( 33.38149988018159320, -281.3022602403335100, -288.7471666906474752 ) ) ;
#78770 = CARTESIAN_POINT ( 'NONE',  ( 35.34827300217931878, -276.4494912237666995, -246.0242691206248082 ) ) ;
#78771 = CARTESIAN_POINT ( 'NONE',  ( -101.7388919048687796, -298.4602637870092394, -234.7468426564614106 ) ) ;
#78772 = CARTESIAN_POINT ( 'NONE',  ( -79.04199218841267793, -282.6586478207116784, -334.8119197978743955 ) ) ;
#78773 = CARTESIAN_POINT ( 'NONE',  ( -104.4848757726212085, -292.7268833308195894, -239.2200201331006610 ) ) ;
#78774 = CARTESIAN_POINT ( 'NONE',  ( -36.96437105546868906, -275.6569558883413151, -194.1491333638721812 ) ) ;
#78775 = CARTESIAN_POINT ( 'NONE',  ( -89.83674463381768760, -274.6452151841528462, -214.6329514324554282 ) ) ;
#78776 = CARTESIAN_POINT ( 'NONE',  ( 140.6539576904058606, 276.0000000000000568, 10.50000000000000000 ) ) ;
#78777 = CARTESIAN_POINT ( 'NONE',  ( 17.52010263984465865, -296.2658354158406837, -321.2552337926327937 ) ) ;
#78778 = CARTESIAN_POINT ( 'NONE',  ( -109.5364183966800908, -282.2975897107580749, -290.1060335739248330 ) ) ;
#78779 = CARTESIAN_POINT ( 'NONE',  ( -114.2303868047341808, -290.1722751346385962, -274.0859203373668720 ) ) ;
#78780 = CARTESIAN_POINT ( 'NONE',  ( 37.28787442950225284, -273.5528023500567656, -268.8533378336859982 ) ) ;
#78781 = CARTESIAN_POINT ( 'NONE',  ( 35.91639016150526942, -288.8845141295504959, -249.2050913817516005 ) ) ;
#78782 = CARTESIAN_POINT ( 'NONE',  ( -101.3870638784975711, -289.9594237387763656, -234.5859267401124271 ) ) ;
#78783 = ORIENTED_EDGE ( 'NONE', *, *, #14703, .F. ) ;
#78784 = CARTESIAN_POINT ( 'NONE',  ( -101.8139284062927601, -288.5840749097957882, -311.4699592090917122 ) ) ;
#78785 = CARTESIAN_POINT ( 'NONE',  ( -107.7473328911050459, -289.9608120914307960, -289.9158785394840265 ) ) ;
#78786 = ORIENTED_EDGE ( 'NONE', *, *, #40401, .F. ) ;
#78787 = CARTESIAN_POINT ( 'NONE',  ( 32.58867012579311506, -289.0355857338158785, -301.8450158519042930 ) ) ;
#78788 = CARTESIAN_POINT ( 'NONE',  ( 18.32728339696601694, -276.5571478352205190, -317.6162950548729214 ) ) ;
#78789 = CARTESIAN_POINT ( 'NONE',  ( 21.12304930792435798, -293.1442356326679715, -319.9934218183161647 ) ) ;
#78790 = CARTESIAN_POINT ( 'NONE',  ( -102.5028351540022271, -285.4222619314238045, -229.3761112896763734 ) ) ;
#78791 = CARTESIAN_POINT ( 'NONE',  ( 34.25225138021647098, -282.0757264132767546, -284.7904662526069046 ) ) ;
#78792 = CARTESIAN_POINT ( 'NONE',  ( 64.77658176787873856, 47.97751566260769351, -318.9316874262945589 ) ) ;
#78793 = CARTESIAN_POINT ( 'NONE',  ( -23.26540662898876732, -107.7375312792409972, -361.8887297295785288 ) ) ;
#78794 = CARTESIAN_POINT ( 'NONE',  ( -106.1534499783927572, -259.7701228362822690, -315.4954753543551078 ) ) ;
#78795 = CARTESIAN_POINT ( 'NONE',  ( -34.02314740851217323, -273.2921226783739712, -197.2749432629602779 ) ) ;
#78796 = CARTESIAN_POINT ( 'NONE',  ( -46.20256731205039102, -272.8574258610898369, -197.5894812963507832 ) ) ;
#78797 = CARTESIAN_POINT ( 'NONE',  ( -95.53906058955573144, -295.3794392362768235, -320.6860038612025505 ) ) ;
#78798 = CARTESIAN_POINT ( 'NONE',  ( -75.91738900125099576, -208.6651993415634081, -353.8496858908021068 ) ) ;
#78799 = CARTESIAN_POINT ( 'NONE',  ( 0.9631155154215390590, -273.2369321440110639, -204.1187490609767963 ) ) ;
#78800 = CARTESIAN_POINT ( 'NONE',  ( -73.46837056570362279, -299.4278360822341938, -205.5095245980904792 ) ) ;
#78801 = CARTESIAN_POINT ( 'NONE',  ( 10.44856727470821234, -289.6915794273643314, -326.2615094317041553 ) ) ;
#78802 = CARTESIAN_POINT ( 'NONE',  ( -110.6773800185677032, -291.6567055389387519, -268.4674349851497368 ) ) ;
#78803 = VERTEX_POINT ( 'NONE', #28108 ) ;
#78804 = CARTESIAN_POINT ( 'NONE',  ( -104.3915305150653410, -297.0060870749479705, -307.8480964781485341 ) ) ;
#78805 = CARTESIAN_POINT ( 'NONE',  ( -35.93856748887137798, -286.5625707395337827, -197.3130539380764503 ) ) ;
#78806 = CARTESIAN_POINT ( 'NONE',  ( 8.817326177506853213, -295.2398443936248782, -331.7899638982167403 ) ) ;
#78807 = CARTESIAN_POINT ( 'NONE',  ( -44.78342606498735989, -295.6361621060548828, -346.9922044147858173 ) ) ;
#78808 = CARTESIAN_POINT ( 'NONE',  ( 27.48556370688076456, -293.2624134424286808, -236.7988494633435153 ) ) ;
#78809 = VERTEX_POINT ( 'NONE', #93409 ) ;
#78810 = CARTESIAN_POINT ( 'NONE',  ( -95.83714058952023152, -275.1268382058628390, -222.5120833378332179 ) ) ;
#78811 = ADVANCED_FACE ( 'NONE', ( #35185 ), #14824, .F. ) ;
#78812 = ORIENTED_EDGE ( 'NONE', *, *, #15031, .F. ) ;
#78813 = CARTESIAN_POINT ( 'NONE',  ( -107.3605141159134604, -278.4691808941695399, -238.3441166582337019 ) ) ;
#78814 = CARTESIAN_POINT ( 'NONE',  ( 34.35897646600415811, -274.1807475357840644, -287.8915151973031925 ) ) ;
#78815 = CARTESIAN_POINT ( 'NONE',  ( 30.50050871200883051, -276.8633059683416491, -298.0794949333244404 ) ) ;
#78816 = CARTESIAN_POINT ( 'NONE',  ( -34.16824712897884808, -275.8516850649032790, -194.4407438300254682 ) ) ;
#78817 = AXIS2_PLACEMENT_3D ( 'NONE', #90028, #82924, #19361 ) ;
#78818 = CARTESIAN_POINT ( 'NONE',  ( 36.34250494505783280, -273.3698105997611947, -254.5188725013404678 ) ) ;
#78819 = CARTESIAN_POINT ( 'NONE',  ( -108.2758702109818785, -297.4370336704475335, -252.6396406791724303 ) ) ;
#78820 = CARTESIAN_POINT ( 'NONE',  ( -97.67680051326463797, -294.5441423895704816, -312.4924671092201152 ) ) ;
#78821 = LINE ( 'NONE', #30027, #85000 ) ;
#78822 = CARTESIAN_POINT ( 'NONE',  ( -99.59627549111229428, -278.4439350502482853, -315.5929721016261169 ) ) ;
#78823 = CARTESIAN_POINT ( 'NONE',  ( -5.064173771200484175, -276.7817252548840088, -335.8514264305433699 ) ) ;
#78824 = CARTESIAN_POINT ( 'NONE',  ( 35.38551671859860903, -285.9343379331483561, -246.4418350914553457 ) ) ;
#78825 = CARTESIAN_POINT ( 'NONE',  ( -34.86135989402453816, -300.0832881303522868, -195.1935993454034133 ) ) ;
#78826 = CARTESIAN_POINT ( 'NONE',  ( 82.64002947064351190, -300.2510188964802182, -197.7678940087098454 ) ) ;
#78827 = CARTESIAN_POINT ( 'NONE',  ( 5.931921739323415821, -287.6457775068022329, -329.4157334304510982 ) ) ;
#78828 = CARTESIAN_POINT ( 'NONE',  ( -6.324579191209457107, -278.7051285722065472, -203.1467440808307572 ) ) ;
#78829 = CARTESIAN_POINT ( 'NONE',  ( -24.75793025553718962, -278.7905718417633807, -197.8557826513423379 ) ) ;
#78830 = CARTESIAN_POINT ( 'NONE',  ( -3.264513540184294182, -284.6023387384749981, -337.1865673937621750 ) ) ;
#78831 = CARTESIAN_POINT ( 'NONE',  ( -71.82724894726753462, -278.7237059831081183, -335.1663219729223897 ) ) ;
#78832 = DIRECTION ( 'NONE',  ( 0.000000000000000000, 0.000000000000000000, 1.000000000000000000 ) ) ;
#78833 = CARTESIAN_POINT ( 'NONE',  ( 35.29383523686740887, -274.2445745864573041, -293.3941251146179070 ) ) ;
#78834 = CARTESIAN_POINT ( 'NONE',  ( 29.17535785020994510, -275.7938614549270255, -239.9175198899723966 ) ) ;
#78835 = CARTESIAN_POINT ( 'NONE',  ( 23.10197250560197091, -282.9439607906085712, -225.6778899466615940 ) ) ;
#78836 = CARTESIAN_POINT ( 'NONE',  ( 175.2296996224750103, 247.0000000000001137, 9.550761578869391144 ) ) ;
#78837 = CARTESIAN_POINT ( 'NONE',  ( 37.54479479385048535, -289.3440152264710719, -260.2949828763424875 ) ) ;
#78838 = CARTESIAN_POINT ( 'NONE',  ( 4.793351120182042457, -292.4833538933152681, -332.4682561183909115 ) ) ;
#78839 = CARTESIAN_POINT ( 'NONE',  ( 164.2231345125756263, 300.2961574867697436, -7.500000000000000000 ) ) ;
#78840 = CARTESIAN_POINT ( 'NONE',  ( -29.92354717195936331, -272.8328310150862990, -197.2433056211007738 ) ) ;
#78841 = CARTESIAN_POINT ( 'NONE',  ( -22.47041274133773570, -290.3841489371648663, -197.6307234492704765 ) ) ;
#78842 = CARTESIAN_POINT ( 'NONE',  ( -49.37856652629597676, -155.6656457446864010, -366.7448178265262868 ) ) ;
#78843 = LINE ( 'NONE', #35763, #15682 ) ;
#78844 = CARTESIAN_POINT ( 'NONE',  ( -54.36593831843376279, -287.7467392801374899, -344.7986921315372797 ) ) ;
#78845 = CARTESIAN_POINT ( 'NONE',  ( -3.914639667600360529, -284.7268310658551513, -202.1074524777421857 ) ) ;
#78846 = CARTESIAN_POINT ( 'NONE',  ( -34.80821971631973355, -284.4450152945685204, -343.9192623047369466 ) ) ;
#78847 = CARTESIAN_POINT ( 'NONE',  ( -89.00108409341792992, -284.6037231211263361, -322.2386801374091760 ) ) ;
#78848 = CARTESIAN_POINT ( 'NONE',  ( -68.95659831317985322, -293.6184361392986943, -201.9445591541790748 ) ) ;
#78849 = CARTESIAN_POINT ( 'NONE',  ( -32.68812320711818842, -274.4425430918141160, -193.5099041309908898 ) ) ;
#78850 = CARTESIAN_POINT ( 'NONE',  ( -109.8434314805830496, -288.9039998675888228, -249.0817112723595415 ) ) ;
#78851 = CARTESIAN_POINT ( 'NONE',  ( -71.57085032350299514, -277.4918688796414017, -339.3347743804868628 ) ) ;
#78852 = CARTESIAN_POINT ( 'NONE',  ( -2.350907528260103074, -296.5666174542132012, -336.2966261577164460 ) ) ;
#78853 = CARTESIAN_POINT ( 'NONE',  ( -48.18343439339133027, -261.1465603064058314, -445.1129026112122347 ) ) ;
#78854 = CARTESIAN_POINT ( 'NONE',  ( 209.1929142650026279, 37.10830422238664283, 12.90287354992391045 ) ) ;
#78855 = CARTESIAN_POINT ( 'NONE',  ( -106.0198643532816760, -283.5839705646019979, -244.1971497086835541 ) ) ;
#78856 = CARTESIAN_POINT ( 'NONE',  ( -66.55920959481436228, -277.6693198048137106, -201.2862470725625883 ) ) ;
#78857 = CARTESIAN_POINT ( 'NONE',  ( -113.6483667957982249, -271.0322748495758560, -270.3418062714382586 ) ) ;
#78858 = CARTESIAN_POINT ( 'NONE',  ( -43.22354951157114300, -276.4769711681833542, -343.2260376357445466 ) ) ;
#78859 = CARTESIAN_POINT ( 'NONE',  ( -5.761906345179846234, -293.9952320767264951, -203.7632424565805991 ) ) ;
#78860 = CARTESIAN_POINT ( 'NONE',  ( 25.04203643358045284, -293.9651293498113773, -231.9024160321915247 ) ) ;
#78861 = ADVANCED_FACE ( 'NONE', ( #42277 ), #87681, .T. ) ;
#78862 = CARTESIAN_POINT ( 'NONE',  ( -58.69750209010320674, -296.6377533089294047, -343.8821592511580434 ) ) ;
#78863 = CARTESIAN_POINT ( 'NONE',  ( -106.8699237221404132, -296.0885254884846631, -292.7694633599614917 ) ) ;
#78864 = CARTESIAN_POINT ( 'NONE',  ( -7.397180472973788667, -290.6598054528595867, -339.1794754100254750 ) ) ;
#78865 = CARTESIAN_POINT ( 'NONE',  ( -97.17105238061110128, -284.0685135171043498, -318.8529486178920251 ) ) ;
#78866 = CARTESIAN_POINT ( 'NONE',  ( -91.27292320571639550, -271.4346562141673189, -217.1471286850362219 ) ) ;
#78867 = CARTESIAN_POINT ( 'NONE',  ( -40.81434760645371540, -285.8430587348753988, -193.3872716976526078 ) ) ;
#78868 = CARTESIAN_POINT ( 'NONE',  ( -48.83680483807923167, -279.1790349570469516, -344.1680478054839796 ) ) ;
#78869 = EDGE_CURVE ( 'NONE', #783, #15111, #65037, .T. ) ;
#78870 = CARTESIAN_POINT ( 'NONE',  ( -33.21344459669982996, -285.1640135841489609, -197.1922896316770561 ) ) ;
#78871 = CARTESIAN_POINT ( 'NONE',  ( -72.26575763000421659, -287.5139771011550920, -336.7480090562880832 ) ) ;
#78872 = CARTESIAN_POINT ( 'NONE',  ( 10.80643407470098794, -61.58976173765800155, -353.1561788127373802 ) ) ;
#78873 = CARTESIAN_POINT ( 'NONE',  ( 30.02093982759445367, -286.6789709701212132, -241.9411504204626056 ) ) ;
#78874 = TOROIDAL_SURFACE ( 'NONE', #38023, 24.00000000000000355, 1.000000000000000000 ) ;
#78875 = CARTESIAN_POINT ( 'NONE',  ( -13.48365126673568959, -283.6910015016651982, -343.3242163065697241 ) ) ;
#78876 = CARTESIAN_POINT ( 'NONE',  ( -107.0417464003678418, -290.0250958174759717, -238.0673917571192533 ) ) ;
#78877 = CARTESIAN_POINT ( 'NONE',  ( -81.78891360139557776, -281.0579529140076147, -208.4669694056055960 ) ) ;
#78878 = CARTESIAN_POINT ( 'NONE',  ( -112.7532461084423971, -280.0296876695396122, -257.4616216287933526 ) ) ;
#78879 = CARTESIAN_POINT ( 'NONE',  ( -3.147213100939972197, -280.3504110376719609, -205.8509164363069885 ) ) ;
#78880 = CARTESIAN_POINT ( 'NONE',  ( -31.22960994268312618, -276.1096044057277936, -195.9540361349819193 ) ) ;
#78881 = CARTESIAN_POINT ( 'NONE',  ( 0.5405028384220336157, -294.5617322281331667, -337.4131433633274355 ) ) ;
#78882 = CARTESIAN_POINT ( 'NONE',  ( -76.75821235114470653, -287.6028049805501041, -333.7502760934303865 ) ) ;
#78883 = TOROIDAL_SURFACE ( 'NONE', #35078, 2.000000000000000000, 1.000000000000000000 ) ;
#78884 = CARTESIAN_POINT ( 'NONE',  ( -71.82861590845720912, -293.2041853916803120, -202.3974742059271250 ) ) ;
#78885 = CARTESIAN_POINT ( 'NONE',  ( -109.4486622139711613, -295.2978827748174808, -283.6523805615703964 ) ) ;
#78886 = ORIENTED_EDGE ( 'NONE', *, *, #24174, .T. ) ;
#78887 = CARTESIAN_POINT ( 'NONE',  ( -1.718459570622664856, -284.4964707525649601, -335.7385166820840254 ) ) ;
#78888 = CARTESIAN_POINT ( 'NONE',  ( -109.8260110367138225, -296.0969714280259382, -279.6043115475146692 ) ) ;
#78889 = CARTESIAN_POINT ( 'NONE',  ( -27.90083520284281349, -293.2488765034984795, -194.2000875221678768 ) ) ;
#78890 = CARTESIAN_POINT ( 'NONE',  ( 9.335259180758857411, -281.3645403619297554, -214.0354353454985414 ) ) ;
#78891 = CARTESIAN_POINT ( 'NONE',  ( -64.80467480614187537, -272.7608827618702776, -198.6629112136309061 ) ) ;
#78892 = CARTESIAN_POINT ( 'NONE',  ( -106.4182938034128796, -290.7677145646187000, -304.2717275767953424 ) ) ;
#78893 = CARTESIAN_POINT ( 'NONE',  ( 0.2348261872157848540, -280.6969583256506553, -336.1659974276649905 ) ) ;
#78894 = CARTESIAN_POINT ( 'NONE',  ( -95.64767900399191092, -291.5644882152136574, -220.0800782025988553 ) ) ;
#78895 = CARTESIAN_POINT ( 'NONE',  ( -8.206155462136184298, -288.9931955268025945, -337.3719334296230841 ) ) ;
#78896 = CARTESIAN_POINT ( 'NONE',  ( 139.6539576904058606, 132.0000000000000568, -10.49999999999999822 ) ) ;
#78897 = DIRECTION ( 'NONE',  ( -1.000000000000000000, 0.000000000000000000, 0.000000000000000000 ) ) ;
#78898 = CARTESIAN_POINT ( 'NONE',  ( 173.5779064319110603, 240.4672869823826886, -177.0707307568671069 ) ) ;
#78899 = CARTESIAN_POINT ( 'NONE',  ( -4.771743288812454686, -277.9809262143061233, -202.8022627189028810 ) ) ;
#78900 = CARTESIAN_POINT ( 'NONE',  ( -110.4418981769703407, -277.7099087781375033, -273.3549068340353188 ) ) ;
#78901 = ORIENTED_EDGE ( 'NONE', *, *, #75967, .F. ) ;
#78902 = CARTESIAN_POINT ( 'NONE',  ( -93.31736081847009245, -278.1426119315385677, -223.0031239198665958 ) ) ;
#78903 = CARTESIAN_POINT ( 'NONE',  ( -24.15905243364050037, -273.8826642618506071, -194.4652750547240032 ) ) ;
#78904 = CARTESIAN_POINT ( 'NONE',  ( -37.52155448479069122, -140.8893142108368295, -362.3101970415223150 ) ) ;
#78905 = CARTESIAN_POINT ( 'NONE',  ( -98.94200552241284186, -277.7322230586455021, -225.1283281292398044 ) ) ;
#78906 = CARTESIAN_POINT ( 'NONE',  ( -26.52888351673109213, -280.9341468423341439, -344.2710678366819934 ) ) ;
#78907 = CARTESIAN_POINT ( 'NONE',  ( -112.6012921497164712, -298.4463838982779862, -259.7802429206159331 ) ) ;
#78908 = CARTESIAN_POINT ( 'NONE',  ( 32.40741619691913655, -294.3324734275357741, -292.1108125454542801 ) ) ;
#78909 = EDGE_LOOP ( 'NONE', ( #26472, #19489, #9245, #89425 ) ) ;
#78910 = CARTESIAN_POINT ( 'NONE',  ( -70.20794647113758913, -288.1794116207494199, -336.1097920166418476 ) ) ;
#78911 = CARTESIAN_POINT ( 'NONE',  ( 32.45704842535066348, -275.7887021480069052, -237.9628780341154766 ) ) ;
#78912 = CARTESIAN_POINT ( 'NONE',  ( -63.08145301655268611, -297.8741905686242148, -201.9961077622904497 ) ) ;
#78913 = VERTEX_POINT ( 'NONE', #13891 ) ;
#78914 = LINE ( 'NONE', #84598, #32604 ) ;
#78915 = DIRECTION ( 'NONE',  ( 0.000000000000000000, 1.000000000000000000, 0.000000000000000000 ) ) ;
#78916 = CARTESIAN_POINT ( 'NONE',  ( 155.4202272374197946, 20.25578850494681760, 12.04866793599625296 ) ) ;
#78917 = CARTESIAN_POINT ( 'NONE',  ( -72.28912095828310669, -280.6578545327106440, -205.9180900315417375 ) ) ;
#78918 = CARTESIAN_POINT ( 'NONE',  ( -1.631734303739330150, -282.2789878187024328, -203.2882295976607736 ) ) ;
#78919 = CARTESIAN_POINT ( 'NONE',  ( -69.12208016560440171, -282.5394972001288352, -336.3553872796270525 ) ) ;
#78920 = CARTESIAN_POINT ( 'NONE',  ( -49.36490895107633747, -281.7576888984771131, -197.1060299160584748 ) ) ;
#78921 = CARTESIAN_POINT ( 'NONE',  ( -9.746533694308324058, -275.1649145764586706, -338.7064619056924926 ) ) ;
#78922 = EDGE_CURVE ( 'NONE', #75154, #35472, #36581, .T. ) ;
#78923 = DIRECTION ( 'NONE',  ( 0.000000000000000000, 1.000000000000000000, 0.000000000000000000 ) ) ;
#78924 = EDGE_CURVE ( 'NONE', #44442, #61882, #71661, .T. ) ;
#78925 = DIRECTION ( 'NONE',  ( 1.000000000000000000, -0.000000000000000000, 0.000000000000000000 ) ) ;
#78926 = CARTESIAN_POINT ( 'NONE',  ( -106.1961321355999104, -278.9143613314565755, -304.5868961496231009 ) ) ;
#78927 = VERTEX_POINT ( 'NONE', #7696 ) ;
#78928 = ORIENTED_EDGE ( 'NONE', *, *, #66277, .F. ) ;
#78929 = DIRECTION ( 'NONE',  ( -0.000000000000000000, -1.000000000000000000, -0.000000000000000000 ) ) ;
#78930 = CARTESIAN_POINT ( 'NONE',  ( -111.8647353856507607, -286.6791702598127358, -258.8482816898892906 ) ) ;
#78931 = CARTESIAN_POINT ( 'NONE',  ( 27.29595319998228220, -293.2164570076552650, -304.7414272618611903 ) ) ;
#78932 = CARTESIAN_POINT ( 'NONE',  ( 14.52882399755339549, -287.6938420228087239, -327.2026394220102929 ) ) ;
#78933 = CARTESIAN_POINT ( 'NONE',  ( -103.1290018275198292, -283.2467187788606111, -236.4493951409342003 ) ) ;
#78935 = CARTESIAN_POINT ( 'NONE',  ( -78.75979019367456146, -287.8580833506096610, -331.7621786844200642 ) ) ;
#78934 = CARTESIAN_POINT ( 'NONE',  ( -109.5612260839293270, -282.9419441419296390, -284.4931733608713103 ) ) ;
#78936 = CARTESIAN_POINT ( 'NONE',  ( 31.73347737416975889, -283.0876891809436984, -295.3257960551916881 ) ) ;
#78937 = CARTESIAN_POINT ( 'NONE',  ( 26.80552617765052403, -273.0300826955864864, -231.4013386424830117 ) ) ;
#78938 = VECTOR ( 'NONE', #41767, 1000.000000000000000 ) ;
#78939 = CARTESIAN_POINT ( 'NONE',  ( -112.6931817981279238, -283.0997274476171128, -258.6738327191150120 ) ) ;
#78940 = CARTESIAN_POINT ( 'NONE',  ( -101.3939463261774421, -298.0292207629465224, -309.3779144189761041 ) ) ;
#78941 = CARTESIAN_POINT ( 'NONE',  ( -43.49028171077085858, -283.9746241944650365, -195.3943532962559289 ) ) ;
#78942 = PRESENTATION_LAYER_ASSIGNMENT (  '', '', ( #53240 ) ) ;
#78943 = CARTESIAN_POINT ( 'NONE',  ( -108.7128739231729355, -279.2767854794305435, -286.8350595912751260 ) ) ;
#78944 = CARTESIAN_POINT ( 'NONE',  ( 36.48463492266933628, -289.3712653640114354, -256.2295688029942085 ) ) ;
#78945 = DIRECTION ( 'NONE',  ( 0.000000000000000000, 0.000000000000000000, 1.000000000000000000 ) ) ;
#78946 = CARTESIAN_POINT ( 'NONE',  ( 115.2448031289451222, -299.5541904835127980, -192.4725777504219764 ) ) ;
#78947 = CARTESIAN_POINT ( 'NONE',  ( 30.87518737893181964, -295.0464627211969741, -237.7469852750401174 ) ) ;
#78948 = CIRCLE ( 'NONE', #47147, 4.000000000000003553 ) ;
#78949 = CARTESIAN_POINT ( 'NONE',  ( -112.3934048168566449, -276.5486602767667819, -270.6202188770992052 ) ) ;
#78950 = CARTESIAN_POINT ( 'NONE',  ( -113.2022639796064283, -289.5961707772405589, -282.5813337224485622 ) ) ;
#78951 = CARTESIAN_POINT ( 'NONE',  ( -35.65251099251693034, -293.4305128756887484, -344.1544198635715475 ) ) ;
#78952 = CARTESIAN_POINT ( 'NONE',  ( -19.39804725191485346, -278.9725256703936793, -199.0394823117002261 ) ) ;
#78953 = CARTESIAN_POINT ( 'NONE',  ( -105.6924020575499981, -271.0221210805106580, -240.7433747872985350 ) ) ;
#78954 = CARTESIAN_POINT ( 'NONE',  ( -47.07625192294526784, -293.2410892646867637, -197.5155142810987172 ) ) ;
#78955 = CARTESIAN_POINT ( 'NONE',  ( 35.78497577281001440, -278.2662352645559167, -287.0191576251351080 ) ) ;
#78956 = CARTESIAN_POINT ( 'NONE',  ( -88.15826690957084111, -294.2278172877752240, -327.3563636301191195 ) ) ;
#78957 = CARTESIAN_POINT ( 'NONE',  ( -75.10797703767903499, -291.1644666894471811, -333.7806064352284352 ) ) ;
#78958 = CARTESIAN_POINT ( 'NONE',  ( -53.15624617916034822, -290.0920747309290846, -195.9845703565227666 ) ) ;
#78959 = CARTESIAN_POINT ( 'NONE',  ( 1.638962253470107822, -289.9450202306061897, -332.7781258969576470 ) ) ;
#78960 = CARTESIAN_POINT ( 'NONE',  ( 73.43068321062709458, -178.2391364535880882, 4.999999999999990230 ) ) ;
#78961 = CARTESIAN_POINT ( 'NONE',  ( -109.9485146625290639, -291.2366339913398292, -279.3529036812778372 ) ) ;
#78962 = CARTESIAN_POINT ( 'NONE',  ( 194.7453183674696220, 20.99999999999998934, 15.62500000000049205 ) ) ;
#78963 = CARTESIAN_POINT ( 'NONE',  ( -98.89473777838313140, -292.3667677402772824, -224.7405391657489702 ) ) ;
#78965 = CARTESIAN_POINT ( 'NONE',  ( -74.97960796736299471, -291.5360538297308608, -207.7530187480938935 ) ) ;
#78964 = CARTESIAN_POINT ( 'NONE',  ( 17.97035896663818377, -278.8599975304961163, -219.1851185104262356 ) ) ;
#78966 = CARTESIAN_POINT ( 'NONE',  ( -73.75938689446978458, -279.9154809110895030, -202.5265839825511591 ) ) ;
#78967 = CARTESIAN_POINT ( 'NONE',  ( 35.58768585597451306, -281.5311615601613653, -295.1651080151920610 ) ) ;
#78968 = CARTESIAN_POINT ( 'NONE',  ( 36.24155671752620833, -285.7391356254493644, -284.9361835682964283 ) ) ;
#78969 = CARTESIAN_POINT ( 'NONE',  ( 60.29495240252358457, -249.1689065933674954, -21.50000000000000000 ) ) ;
#78970 = CARTESIAN_POINT ( 'NONE',  ( 1.731642746028122293, -280.6635912512215327, -333.5411716630344472 ) ) ;
#78971 = CARTESIAN_POINT ( 'NONE',  ( -111.0282782149008227, -282.7348430773326982, -256.1168183383626911 ) ) ;
#78972 = CARTESIAN_POINT ( 'NONE',  ( -113.5175712458702151, -277.0883914838248074, -265.8952014382018660 ) ) ;
#78973 = CARTESIAN_POINT ( 'NONE',  ( -32.31290222346393648, -285.0344713512181443, -193.8221677869262010 ) ) ;
#78974 = CARTESIAN_POINT ( 'NONE',  ( -74.36390285328373295, -274.3494877460457815, -207.1996685218972232 ) ) ;
#78975 = LINE ( 'NONE', #42992, #9505 ) ;
#78976 = CARTESIAN_POINT ( 'NONE',  ( -88.49967645557970286, -292.9208466164516835, -217.0992917846135697 ) ) ;
#78977 = CARTESIAN_POINT ( 'NONE',  ( 37.33373697168995875, -277.1822559437940185, -286.6144554531836661 ) ) ;
#78978 = CARTESIAN_POINT ( 'NONE',  ( -1.463542023603061626, -276.2294975482097357, -334.0174323099013236 ) ) ;
#78979 = CARTESIAN_POINT ( 'NONE',  ( -45.27771372789302973, -297.1527124858308184, -344.9919308154136388 ) ) ;
#78980 = CARTESIAN_POINT ( 'NONE',  ( -47.74549346304473829, -292.0901649240898905, -194.0134106347832130 ) ) ;
#78981 = CARTESIAN_POINT ( 'NONE',  ( 22.61979547779134236, -279.0068178028008674, -224.3624431170859737 ) ) ;
#78982 = CARTESIAN_POINT ( 'NONE',  ( 8.852622518109109606, -292.4991279329794907, -208.6903129998639486 ) ) ;
#78983 = CARTESIAN_POINT ( 'NONE',  ( -64.14660568663879303, -290.7524386144834807, -202.1939988687319953 ) ) ;
#78984 = CARTESIAN_POINT ( 'NONE',  ( -69.96165230614145969, -293.4815471628326691, -337.9099801907603364 ) ) ;
#78985 = EDGE_LOOP ( 'NONE', ( #28045, #56323, #57978, #5736, #40328, #5277, #21730, #69221 ) ) ;
#78986 = CARTESIAN_POINT ( 'NONE',  ( 196.1963538710215857, 305.7026273589066250, 13.99999999999999112 ) ) ;
#78987 = CARTESIAN_POINT ( 'NONE',  ( -28.09234808330295508, -291.6802321888474125, -197.8366215881910648 ) ) ;
#78988 = DIRECTION ( 'NONE',  ( -0.000000000000000000, -0.000000000000000000, 1.000000000000000000 ) ) ;
#78989 = CARTESIAN_POINT ( 'NONE',  ( 7.450504543161054372, -278.1952119285919025, -214.2458315076590907 ) ) ;
#78990 = CARTESIAN_POINT ( 'NONE',  ( -98.09561277386116274, -294.9826697811271288, -317.2842712457926382 ) ) ;
#78991 = CARTESIAN_POINT ( 'NONE',  ( -74.02471211983743160, -284.8438110493802355, -337.5592944692355672 ) ) ;
#78992 = CARTESIAN_POINT ( 'NONE',  ( 33.02983144176683084, -287.1289582087076155, -250.9485563526661736 ) ) ;
#78993 = CARTESIAN_POINT ( 'NONE',  ( 31.91998520578383136, -277.4062370247862646, -295.6794710091879210 ) ) ;
#78994 = CARTESIAN_POINT ( 'NONE',  ( 30.98575699803977912, -291.9676829140881296, -300.4144938733773529 ) ) ;
#78995 = CARTESIAN_POINT ( 'NONE',  ( -42.43742302147538226, -296.8774444451054819, -344.1988293656959286 ) ) ;
#78996 = EDGE_CURVE ( 'NONE', #1023, #44839, #28561, .T. ) ;
#78997 = CARTESIAN_POINT ( 'NONE',  ( 18.60115680843961883, -275.0190396884473785, -317.8745609602932518 ) ) ;
#78998 = EDGE_LOOP ( 'NONE', ( #35731, #10409, #85042, #11599 ) ) ;
#78999 = CARTESIAN_POINT ( 'NONE',  ( 195.4524165401237212, 39.48855364940461499, 14.00000000000000000 ) ) ;
#79000 = CARTESIAN_POINT ( 'NONE',  ( -112.2528006584647216, -296.4405859559370242, -252.6390608506351327 ) ) ;
#79001 = CARTESIAN_POINT ( 'NONE',  ( 35.42338579777820939, -289.6761622161643004, -286.1231115687391480 ) ) ;
#79002 = CARTESIAN_POINT ( 'NONE',  ( -84.44664919488533883, -295.4040081216920726, -211.9331678762224271 ) ) ;
#79003 = CARTESIAN_POINT ( 'NONE',  ( 98.49150853115541793, -300.7950733892176913, -193.6458855816779874 ) ) ;
#79004 = CARTESIAN_POINT ( 'NONE',  ( 35.73227068942294693, -288.2482951890425511, -273.7563026306463030 ) ) ;
#79005 = ORIENTED_EDGE ( 'NONE', *, *, #1254, .F. ) ;
#79006 = CARTESIAN_POINT ( 'NONE',  ( -53.69861665899627923, -278.9060841369510513, -195.3049074928894129 ) ) ;
#79007 = CARTESIAN_POINT ( 'NONE',  ( -27.75230952064942258, -295.5849626746381773, -346.7121539191600164 ) ) ;
#79008 = CARTESIAN_POINT ( 'NONE',  ( -18.06187769216638017, -286.9457734713025161, -343.6318073797739885 ) ) ;
#79009 = CARTESIAN_POINT ( 'NONE',  ( -58.84134463458396880, -295.6560185377389871, -344.3322309400725771 ) ) ;
#79011 = CARTESIAN_POINT ( 'NONE',  ( 23.35646332321589469, -293.3218543279774622, -229.7677633488392814 ) ) ;
#79010 = VECTOR ( 'NONE', #55645, 1000.000000000000000 ) ;
#79012 = CARTESIAN_POINT ( 'NONE',  ( 196.3790618868739273, 71.92834069484581505, -11.42109594865351774 ) ) ;
#79013 = AXIS2_PLACEMENT_3D ( 'NONE', #60063, #24051, #73787 ) ;
#79014 = DIRECTION ( 'NONE',  ( 1.000000000000000000, 0.000000000000000000, 0.000000000000000000 ) ) ;
#79015 = PLANE ( 'NONE',  #35584 ) ;
#79016 = CARTESIAN_POINT ( 'NONE',  ( 19.75497109296140863, -288.3795467302662132, -219.6602438311696801 ) ) ;
#79017 = CARTESIAN_POINT ( 'NONE',  ( -55.63300648810263738, -286.7666405000204577, -350.3538533559490702 ) ) ;
#79018 = ORIENTED_EDGE ( 'NONE', *, *, #40970, .F. ) ;
#79019 = VECTOR ( 'NONE', #55671, 1000.000000000000000 ) ;
#79020 = CARTESIAN_POINT ( 'NONE',  ( -25.40322557732681474, -279.5490952050719784, -194.3954309144580748 ) ) ;
#79021 = CARTESIAN_POINT ( 'NONE',  ( -40.28150681293153212, -285.0893599112288825, -345.1366886295930954 ) ) ;
#79022 = CARTESIAN_POINT ( 'NONE',  ( -113.7514551305627037, -283.1318528975097024, -269.9666160932473531 ) ) ;
#79023 = EDGE_CURVE ( 'NONE', #50851, #89916, #6317, .T. ) ;
#79024 = CARTESIAN_POINT ( 'NONE',  ( 36.17763157261016715, -285.7840312171808250, -282.1136053391057885 ) ) ;
#79025 = CARTESIAN_POINT ( 'NONE',  ( -28.71772082296576301, -278.8044589720365707, -345.6862236181746084 ) ) ;
#79026 = CARTESIAN_POINT ( 'NONE',  ( -110.3630020782395178, -272.9213119432978942, -267.6407032493917768 ) ) ;
#79027 = ORIENTED_EDGE ( 'NONE', *, *, #84489, .T. ) ;
#79029 = CARTESIAN_POINT ( 'NONE',  ( -94.86593167667261639, -278.5360893408447396, -225.2316014027526023 ) ) ;
#79028 = CARTESIAN_POINT ( 'NONE',  ( -68.03742211594335743, -277.4667518209478771, -336.6075814299732087 ) ) ;
#79030 = CARTESIAN_POINT ( 'NONE',  ( 28.23108392948699930, -276.1094184174352222, -230.4890014381589367 ) ) ;
#79031 = CARTESIAN_POINT ( 'NONE',  ( -113.8135618358849257, -277.4033869928183549, -265.8819345132037597 ) ) ;
#79032 = CARTESIAN_POINT ( 'NONE',  ( -71.89434127149799281, -195.1710859107403166, -357.6219360062224268 ) ) ;
#79033 = CARTESIAN_POINT ( 'NONE',  ( -71.30950314752216457, -274.5558265749424436, -201.5206606039367045 ) ) ;
#79034 = ITEM_DEFINED_TRANSFORMATION ( 'NONE', 'NONE', #71888,  #18940 ) ;
#79035 = CARTESIAN_POINT ( 'NONE',  ( -95.13742273932719229, -298.6584553923089516, -220.2995219032252123 ) ) ;
#79036 = CARTESIAN_POINT ( 'NONE',  ( -110.4542110544635705, -280.8376638359844719, -287.0812184334320705 ) ) ;
#79037 = VERTEX_POINT ( 'NONE', #58836 ) ;
#79038 = CARTESIAN_POINT ( 'NONE',  ( 82.68005099394714819, -297.1077358065769545, -194.7517231621825147 ) ) ;
#79039 = CARTESIAN_POINT ( 'NONE',  ( -74.89019309270882729, -286.6190203524091658, -207.3981387827084291 ) ) ;
#79040 = CARTESIAN_POINT ( 'NONE',  ( -112.0068638149089679, -286.4945346981224930, -255.9770754633403556 ) ) ;
#79041 = CARTESIAN_POINT ( 'NONE',  ( 34.10854250403009758, -287.1050116826888257, -285.8715098668070596 ) ) ;
#79042 = CARTESIAN_POINT ( 'NONE',  ( -92.39408616709890509, -283.3219555224582109, -324.1083197198423136 ) ) ;
#79043 = CARTESIAN_POINT ( 'NONE',  ( -11.44352483978653190, -278.7949527497335680, -201.2004479101373988 ) ) ;
#79044 = CARTESIAN_POINT ( 'NONE',  ( -30.43964170806274794, -288.0006417698938321, -196.3958146670315443 ) ) ;
#79045 = CARTESIAN_POINT ( 'NONE',  ( 24.27276458755230948, -279.4757419249573900, -229.8417711537270236 ) ) ;
#79046 = EDGE_CURVE ( 'NONE', #57506, #55010, #64110, .T. ) ;
#79047 = CARTESIAN_POINT ( 'NONE',  ( -32.37058411252477441, -278.3034827085772349, -343.7362568602079591 ) ) ;
#79048 = CARTESIAN_POINT ( 'NONE',  ( 35.41586241191881612, -276.1322549328658624, -277.0188604525927758 ) ) ;
#79049 = CARTESIAN_POINT ( 'NONE',  ( -17.84029575959824854, -287.6010081967024803, -344.4401564830911298 ) ) ;
#79050 = CARTESIAN_POINT ( 'NONE',  ( -18.94712165099068102, -283.6241524709985811, -345.0202402111688116 ) ) ;
#79051 = CARTESIAN_POINT ( 'NONE',  ( -76.72100421368769219, -284.0564177298655864, -336.5197632946659496 ) ) ;
#79052 = CARTESIAN_POINT ( 'NONE',  ( -35.66492747799724583, -280.2404177230881714, -197.3679749760499931 ) ) ;
#79053 = VERTEX_POINT ( 'NONE', #85833 ) ;
#79054 = ORIENTED_EDGE ( 'NONE', *, *, #12440, .T. ) ;
#79055 = CARTESIAN_POINT ( 'NONE',  ( -43.18343439339132317, -486.4924983417995463, -507.6442049081570076 ) ) ;
#79056 = CARTESIAN_POINT ( 'NONE',  ( -3.589367976179181241, -290.4719570152625465, -338.2068158966072815 ) ) ;
#79057 = CARTESIAN_POINT ( 'NONE',  ( -111.5123266642346920, -289.4738570064653231, -251.5462952021527769 ) ) ;
#79058 = CARTESIAN_POINT ( 'NONE',  ( -68.37139696742067940, -272.6930108850667125, -204.0106120328858879 ) ) ;
#79059 = CARTESIAN_POINT ( 'NONE',  ( 4.165289182642732513, -293.8574230422369737, -335.1577442847164434 ) ) ;
#79060 = CARTESIAN_POINT ( 'NONE',  ( -31.83871985894098344, -287.4614679239443262, -343.8998055251485084 ) ) ;
#79061 = CARTESIAN_POINT ( 'NONE',  ( 35.83646968960238155, -291.9405935366683025, -281.7811788958220518 ) ) ;
#79062 = CARTESIAN_POINT ( 'NONE',  ( 19.81478604423949719, -288.1094836800413646, -224.2948569990626879 ) ) ;
#79063 = CARTESIAN_POINT ( 'NONE',  ( -106.6379572354042296, -286.6233781216988064, -303.7686719486574702 ) ) ;
#79064 = CARTESIAN_POINT ( 'NONE',  ( 33.20028212441003745, -289.8843162594131400, -295.9844924791836434 ) ) ;
#79065 = CARTESIAN_POINT ( 'NONE',  ( -110.4847798734278399, -288.3293463769236382, -287.7401912637567420 ) ) ;
#79066 = CARTESIAN_POINT ( 'NONE',  ( -69.38839593716652132, -293.6307019692876565, -202.5386052317078907 ) ) ;
#79067 = CARTESIAN_POINT ( 'NONE',  ( -95.96145803277369168, -286.1076143495420752, -226.4620014548155780 ) ) ;
#79068 = CARTESIAN_POINT ( 'NONE',  ( -1.696263215876659070, -294.5235961217885574, -204.1838465371090763 ) ) ;
#79069 = CARTESIAN_POINT ( 'NONE',  ( 154.5625123364532101, 249.5000000000000568, 13.15740740740741721 ) ) ;
#79070 = CARTESIAN_POINT ( 'NONE',  ( -147.8070425842518034, -211.3363389866113664, -21.49999999999998579 ) ) ;
#79071 = CARTESIAN_POINT ( 'NONE',  ( -108.5558753633842599, -274.8494089183184315, -245.7248023625517703 ) ) ;
#79072 = CARTESIAN_POINT ( 'NONE',  ( 21.13281623876076765, -281.3656235168639341, -314.3514955409482354 ) ) ;
#79073 = CARTESIAN_POINT ( 'NONE',  ( -37.57154704568068837, -281.0549083849263639, -345.3735404960000892 ) ) ;
#79074 = CARTESIAN_POINT ( 'NONE',  ( -66.87185236182260439, -294.6265523897236562, -341.3127909912496989 ) ) ;
#79075 = CARTESIAN_POINT ( 'NONE',  ( 18.05875970769074712, -273.0996638547572388, -221.2059969884263353 ) ) ;
#79076 = CARTESIAN_POINT ( 'NONE',  ( -109.5752345420029457, -276.3985779199023796, -288.4034757575649337 ) ) ;
#79077 = CARTESIAN_POINT ( 'NONE',  ( -77.79732144792812676, -298.8117901221471584, -208.9437320636207858 ) ) ;
#79078 = CIRCLE ( 'NONE', #38214, 4.999999999999990230 ) ;
#79079 = CARTESIAN_POINT ( 'NONE',  ( 34.90629914271126211, -295.1604458767970982, -284.3468793069380354 ) ) ;
#79080 = CARTESIAN_POINT ( 'NONE',  ( 200.3186454232214828, 276.0000000000000568, -3.421094783296261710 ) ) ;
#79081 = CARTESIAN_POINT ( 'NONE',  ( -61.05586080846941144, -296.1707137011913460, -339.6263701201851291 ) ) ;
#79082 = DIRECTION ( 'NONE',  ( -0.000000000000000000, -0.000000000000000000, -1.000000000000000000 ) ) ;
#79083 = AXIS2_PLACEMENT_3D ( 'NONE', #71274, #6401, #35273 ) ;
#79085 = CARTESIAN_POINT ( 'NONE',  ( -86.10028906639864488, -297.3532614223307178, -216.0324882856479007 ) ) ;
#79084 = CARTESIAN_POINT ( 'NONE',  ( 37.71877112819517919, -285.4799834931454257, -263.1404935901517206 ) ) ;
#79086 = CIRCLE ( 'NONE', #91130, 4.000000000000003553 ) ;
#79087 = CARTESIAN_POINT ( 'NONE',  ( -95.33473357636955825, -283.8670801881925740, -321.0149240731760187 ) ) ;
#79088 = CARTESIAN_POINT ( 'NONE',  ( 38.00368735664729058, -287.0207452104713752, -254.5233471232847364 ) ) ;
#79089 = CARTESIAN_POINT ( 'NONE',  ( 5.695741912811828733, -296.4525535926433690, -332.2808796561578788 ) ) ;
#79090 = CARTESIAN_POINT ( 'NONE',  ( 37.45454333412241965, -291.5216695783254295, -268.0051919499569522 ) ) ;
#79091 = AXIS2_PLACEMENT_3D ( 'NONE', #1357, #88458, #39179 ) ;
#79092 = AXIS2_PLACEMENT_3D ( 'NONE', #14628, #56796, #63435 ) ;
#79093 = CARTESIAN_POINT ( 'NONE',  ( -71.15430637165700034, -278.8143139629555094, -201.3620855230111886 ) ) ;
#79094 = CARTESIAN_POINT ( 'NONE',  ( 21.27581636871891391, -285.6952119285919025, -317.1477375740089997 ) ) ;
#79095 = AXIS2_PLACEMENT_3D ( 'NONE', #82199, #89281, #2675 ) ;
#79096 = CARTESIAN_POINT ( 'NONE',  ( -54.94434090351493438, 0.000000000000000000, 54.50000000000000711 ) ) ;
#79097 = CARTESIAN_POINT ( 'NONE',  ( 9.294548659706796556, -285.5046825457539512, -213.6849254267185074 ) ) ;
#79098 = FACE_OUTER_BOUND ( 'NONE', #82749, .T. ) ;
#79099 = FACE_OUTER_BOUND ( 'NONE', #4466, .T. ) ;
#79100 = CARTESIAN_POINT ( 'NONE',  ( -103.2559291042665279, -298.5992459676324415, -237.0545789643600756 ) ) ;
#79101 = CARTESIAN_POINT ( 'NONE',  ( -45.23072790940431531, -281.3794928385150342, -194.3061017038093041 ) ) ;
#79103 = CARTESIAN_POINT ( 'NONE',  ( -18.73563657877088673, -282.8059377833163239, -341.0025749876559757 ) ) ;
#79102 = CARTESIAN_POINT ( 'NONE',  ( -97.75827872194228974, -295.1846231798952545, -225.3035629915742390 ) ) ;
#79104 = CARTESIAN_POINT ( 'NONE',  ( -93.68802243588953615, -296.0032712453432850, -322.8599799035416709 ) ) ;
#79105 = CARTESIAN_POINT ( 'NONE',  ( -44.65699241332127656, -299.4781733326611288, -196.9809026547470978 ) ) ;
#79106 = CARTESIAN_POINT ( 'NONE',  ( 24.38317174045481295, -285.0440647485772843, -226.7572176642513568 ) ) ;
#79107 = CARTESIAN_POINT ( 'NONE',  ( -95.28887016215765016, -281.2091043488537139, -222.7267916886788157 ) ) ;
#79108 = CARTESIAN_POINT ( 'NONE',  ( -98.63795856876178902, -296.1656405682632567, -230.1922296955822560 ) ) ;
#79109 = EDGE_LOOP ( 'NONE', ( #15688, #23913 ) ) ;
#79110 = DIRECTION ( 'NONE',  ( 0.000000000000000000, 1.000000000000000000, 0.000000000000000000 ) ) ;
#79111 = AXIS2_PLACEMENT_3D ( 'NONE', #74271, #59631, #8930 ) ;
#79112 = CARTESIAN_POINT ( 'NONE',  ( -12.96901330259280094, -284.7139131849630758, -340.9695973012406967 ) ) ;
#79113 = FACE_OUTER_BOUND ( 'NONE', #24982, .T. ) ;
#79114 = CARTESIAN_POINT ( 'NONE',  ( -54.49178911615187104, -292.7666405000204009, -345.3538533559490702 ) ) ;
#79115 = CARTESIAN_POINT ( 'NONE',  ( 34.57422617065304138, -274.4062564883361119, -243.3008451689669300 ) ) ;
#79116 = CARTESIAN_POINT ( 'NONE',  ( -46.99236405961787000, -291.7594739362023688, -198.0018429020756798 ) ) ;
#79117 = CARTESIAN_POINT ( 'NONE',  ( -2.841480226516286400, -282.0369403942364102, -205.2281265122227865 ) ) ;
#79118 = CARTESIAN_POINT ( 'NONE',  ( -1.059344518266583934, -278.1625950007542087, -334.6842715454314430 ) ) ;
#79119 = CIRCLE ( 'NONE', #62420, 0.5000000000000004441 ) ;
#79120 = CARTESIAN_POINT ( 'NONE',  ( 15.21663046659259777, -283.9248511803010047, -325.5341394619395601 ) ) ;
#79121 = CARTESIAN_POINT ( 'NONE',  ( 34.03269716037721082, -280.5722925279946480, -287.5266992562808923 ) ) ;
#79122 = CARTESIAN_POINT ( 'NONE',  ( -101.1832053299107486, -281.0817090324558762, -230.9013124160785537 ) ) ;
#79123 = CARTESIAN_POINT ( 'NONE',  ( -114.1811869102184005, -272.7905278953037964, -264.6283571190233488 ) ) ;
#79124 = CARTESIAN_POINT ( 'NONE',  ( 36.58645825288770936, -275.1133394998580002, -248.6427643975326305 ) ) ;
#79125 = CARTESIAN_POINT ( 'NONE',  ( -0.01511613712742478077, -296.4718781068817179, -334.8252405970216046 ) ) ;
#79126 = CARTESIAN_POINT ( 'NONE',  ( 82.64890176555634582, -299.5541904835127980, -195.3611179825600175 ) ) ;
#79127 = DIRECTION ( 'NONE',  ( -1.000000000000000000, 0.000000000000000000, -0.000000000000000000 ) ) ;
#79128 = CARTESIAN_POINT ( 'NONE',  ( -1.314739369625168353, -292.7191797656094536, -337.0268208193561463 ) ) ;
#79129 = CARTESIAN_POINT ( 'NONE',  ( 7.373518244478687755, -274.1886147104881388, -212.5810376143959957 ) ) ;
#79130 = CARTESIAN_POINT ( 'NONE',  ( -50.46630693259032086, -293.4075994641766556, -195.1916265162254831 ) ) ;
#79131 = CARTESIAN_POINT ( 'NONE',  ( -47.70494487000384254, -293.1283933619608888, -194.4089047197740001 ) ) ;
#79132 = CARTESIAN_POINT ( 'NONE',  ( -71.99977451636554804, -291.5116069859776644, -336.6993920046007815 ) ) ;
#79133 = CARTESIAN_POINT ( 'NONE',  ( -98.39585236367773291, -275.9623592486655070, -313.6548391610912745 ) ) ;
#79134 = CARTESIAN_POINT ( 'NONE',  ( -74.71551201268076170, -279.4739139996365793, -334.7390053621615493 ) ) ;
#79135 = CARTESIAN_POINT ( 'NONE',  ( 34.70801452054603686, -291.3897363786066990, -251.6487472191906818 ) ) ;
#79136 = CARTESIAN_POINT ( 'NONE',  ( 5.466522107261644337, -282.4854320657289009, -207.8490264524213273 ) ) ;
#79137 = CARTESIAN_POINT ( 'NONE',  ( -25.07662646889796676, -285.1324192832180415, -198.0337823598655120 ) ) ;
#79138 = ORIENTED_EDGE ( 'NONE', *, *, #23136, .T. ) ;
#79139 = CARTESIAN_POINT ( 'NONE',  ( -70.22824800684831814, -283.1646185734084611, -335.5714386945235788 ) ) ;
#79140 = CARTESIAN_POINT ( 'NONE',  ( -48.08911779156115074, -280.9982872853623803, -194.3734018237312853 ) ) ;
#79141 = AXIS2_PLACEMENT_3D ( 'NONE', #61022, #16983, #23149 ) ;
#79142 = CARTESIAN_POINT ( 'NONE',  ( -83.02670602741321204, -284.2376725254912344, -208.8060475509723517 ) ) ;
#79143 = CARTESIAN_POINT ( 'NONE',  ( -113.9766550460613388, -279.5493691389406195, -265.8997395984927721 ) ) ;
#79144 = EDGE_CURVE ( 'NONE', #24392, #86306, #54891, .T. ) ;
#79145 = CARTESIAN_POINT ( 'NONE',  ( -35.70678016555273615, -278.5521401201835374, -346.6632756690524957 ) ) ;
#79146 = CARTESIAN_POINT ( 'NONE',  ( -67.74223827176244583, -300.1233781216987495, -207.3071070584150277 ) ) ;
#79147 = ORIENTED_EDGE ( 'NONE', *, *, #76386, .F. ) ;
#79148 = CIRCLE ( 'NONE', #91203, 4.103083949679980691 ) ;
#79149 = CARTESIAN_POINT ( 'NONE',  ( -87.45505899282771622, -299.3530998756441477, -214.5610112669792784 ) ) ;
#79150 = AXIS2_PLACEMENT_3D ( 'NONE', #76244, #82862, #11376 ) ;
#79151 = CARTESIAN_POINT ( 'NONE',  ( -110.7450684565213237, -276.7471581634047766, -256.8041152558170666 ) ) ;
#79152 = CARTESIAN_POINT ( 'NONE',  ( -92.09764668828397305, -293.0437876989532811, -217.6007511112921975 ) ) ;
#79153 = CARTESIAN_POINT ( 'NONE',  ( 31.63347452782329938, -293.2242548381822189, -294.7266388817492384 ) ) ;
#79154 = CARTESIAN_POINT ( 'NONE',  ( -111.8639968354835759, -289.8196206036510034, -289.5437691581154240 ) ) ;
#79155 = DIRECTION ( 'NONE',  ( 0.000000000000000000, 0.000000000000000000, 1.000000000000000000 ) ) ;
#79157 = CARTESIAN_POINT ( 'NONE',  ( -92.10128173253971795, -283.6536421092041564, -220.8105176714796301 ) ) ;
#79156 = CARTESIAN_POINT ( 'NONE',  ( 37.77463523503917031, -292.3042784182760556, -284.4368143448964474 ) ) ;
#79158 = CARTESIAN_POINT ( 'NONE',  ( -36.21068021588382635, -293.9268608346539509, -196.1218426852248911 ) ) ;
#79159 = CARTESIAN_POINT ( 'NONE',  ( 15.54038276650088335, -285.2969932414598588, -219.0367274753635058 ) ) ;
#79160 = CARTESIAN_POINT ( 'NONE',  ( -59.07811424488186702, -284.6544381370603105, -340.6198266281787710 ) ) ;
#79161 = CARTESIAN_POINT ( 'NONE',  ( -48.82193415238505452, -290.1360675601515595, -346.3163090201454111 ) ) ;
#79162 = AXIS2_PLACEMENT_3D ( 'NONE', #69868, #55206, #10220 ) ;
#79163 = CARTESIAN_POINT ( 'NONE',  ( 7.174861181162916601, -281.1694834442748743, -212.3638368555477598 ) ) ;
#79164 = CARTESIAN_POINT ( 'NONE',  ( 35.10584442259728633, -292.6642061806714423, -295.4105569810564020 ) ) ;
#79165 = CARTESIAN_POINT ( 'NONE',  ( -62.70069236034566984, -290.1766794308061321, -342.9506861697240652 ) ) ;
#79166 = CARTESIAN_POINT ( 'NONE',  ( -111.4809927416646786, -290.7866492086951666, -290.9254607659004250 ) ) ;
#79167 = CARTESIAN_POINT ( 'NONE',  ( -107.3555660689203535, -284.9943675809792580, -249.5203869174166016 ) ) ;
#79168 = ORIENTED_EDGE ( 'NONE', *, *, #53102, .T. ) ;
#79169 = DIRECTION ( 'NONE',  ( 0.000000000000000000, -1.000000000000000000, 0.000000000000000000 ) ) ;
#79170 = CARTESIAN_POINT ( 'NONE',  ( 10.43801928303763304, -296.2614184942102042, -329.2284366008932466 ) ) ;
#79171 = CIRCLE ( 'NONE', #27810, 0.4999999999999985567 ) ;
#79172 = CARTESIAN_POINT ( 'NONE',  ( -83.89846522891659220, -294.3610253939189079, -331.1384331895002902 ) ) ;
#79173 = EDGE_CURVE ( 'NONE', #83213, #64509, #80134, .T. ) ;
#79174 = CARTESIAN_POINT ( 'NONE',  ( -103.5775531740153070, -278.0331414421972340, -238.9974402746694579 ) ) ;
#79175 = CARTESIAN_POINT ( 'NONE',  ( -102.6634798842978853, -272.5920660887801432, -229.7090332559016019 ) ) ;
#79176 = CARTESIAN_POINT ( 'NONE',  ( -96.16939046213497022, -294.4141897305299267, -314.7667137625541613 ) ) ;
#79177 = CARTESIAN_POINT ( 'NONE',  ( 7.933341928168413659, -276.4407406380216230, -211.8107586522377517 ) ) ;
#79178 = CARTESIAN_POINT ( 'NONE',  ( -72.47168884725178373, -271.7219804956460507, -204.9069881082111806 ) ) ;
#79179 = CARTESIAN_POINT ( 'NONE',  ( 34.33426082907095633, -294.5491481207010906, -254.5015656391188088 ) ) ;
#79180 = CARTESIAN_POINT ( 'NONE',  ( -42.39737519490049067, -296.1970844667483789, -343.4956940975026214 ) ) ;
#79181 = LINE ( 'NONE', #65453, #45958 ) ;
#79182 = AXIS2_PLACEMENT_3D ( 'NONE', #53330, #18285, #76051 ) ;
#79183 = CARTESIAN_POINT ( 'NONE',  ( -104.8552138059868355, -294.9866993970192652, -237.3163923170674536 ) ) ;
#79184 = CARTESIAN_POINT ( 'NONE',  ( -78.15539735354644790, -298.1699746117717496, -205.1878496493273758 ) ) ;
#79185 = CARTESIAN_POINT ( 'NONE',  ( 34.27032864867291551, -286.3486184444865899, -287.3049148862441484 ) ) ;
#79186 = CARTESIAN_POINT ( 'NONE',  ( -108.2041732384576136, -274.8703032238392439, -245.7946662149102508 ) ) ;
#79187 = CARTESIAN_POINT ( 'NONE',  ( -82.68258255700632731, -290.6308873868062506, -327.8729674393077289 ) ) ;
#79188 = CARTESIAN_POINT ( 'NONE',  ( -41.19596605583647886, -274.4973417007616945, -193.4670396566185389 ) ) ;
#79189 = CARTESIAN_POINT ( 'NONE',  ( -86.11756378033236103, -297.6864889449599332, -216.0195812756013254 ) ) ;
#79190 = CARTESIAN_POINT ( 'NONE',  ( -107.1235865821047923, -280.1629335888137007, -298.8021995940503643 ) ) ;
#79191 = CARTESIAN_POINT ( 'NONE',  ( -5.136241568587593065, -279.1521010794865560, -200.9629428362322301 ) ) ;
#79192 = VECTOR ( 'NONE', #36946, 1000.000000000000000 ) ;
#79193 = ORIENTED_EDGE ( 'NONE', *, *, #52823, .T. ) ;
#79194 = CARTESIAN_POINT ( 'NONE',  ( -10.74508538605319252, -282.0629559478086890, -342.5698375703375405 ) ) ;
#79195 = CARTESIAN_POINT ( 'NONE',  ( 37.18848437168953325, -274.6634824389688561, -251.4253215798912890 ) ) ;
#79196 = CARTESIAN_POINT ( 'NONE',  ( -112.4445264367236206, -277.1148561300767028, -257.4767904211815903 ) ) ;
#79197 = CARTESIAN_POINT ( 'NONE',  ( -91.72920324885171794, -277.2794066225720826, -218.4020228094826166 ) ) ;
#79198 = CARTESIAN_POINT ( 'NONE',  ( -82.23219027768399769, -296.1101563351843424, -212.1065338035345462 ) ) ;
#79199 = CARTESIAN_POINT ( 'NONE',  ( 22.14554948011263136, -278.1781031353681897, -316.0573655045046735 ) ) ;
#79200 = CARTESIAN_POINT ( 'NONE',  ( 170.2305261370685798, 214.9910457053126720, -24.90909090909089940 ) ) ;
#79201 = CARTESIAN_POINT ( 'NONE',  ( -63.78743207815339389, -289.7293003644548435, -199.7439107473451543 ) ) ;
#79202 = CARTESIAN_POINT ( 'NONE',  ( -108.3671355284131153, -290.9304081750996716, -240.6224642438094179 ) ) ;
#79203 = CARTESIAN_POINT ( 'NONE',  ( -30.04286117087120545, -276.1444902713843703, -195.5496524448937237 ) ) ;
#79204 = CARTESIAN_POINT ( 'NONE',  ( 10.41666703503159752, -296.6511620856778109, -195.5441041681855836 ) ) ;
#79205 = CARTESIAN_POINT ( 'NONE',  ( -36.55679133239928547, -285.2589399554745455, -193.5135908881578359 ) ) ;
#79206 = FACE_OUTER_BOUND ( 'NONE', #33367, .T. ) ;
#79207 = CARTESIAN_POINT ( 'NONE',  ( -109.9508466224932448, -282.3100271914942141, -289.1971549417632446 ) ) ;
#79208 = LINE ( 'NONE', #44116, #39096 ) ;
#79209 = CARTESIAN_POINT ( 'NONE',  ( 18.79011748054693953, -291.6788726799870233, -223.0710602766620525 ) ) ;
#79210 = CARTESIAN_POINT ( 'NONE',  ( -27.65226149678700196, -284.3161051638186336, -196.7609803617324644 ) ) ;
#79211 = CARTESIAN_POINT ( 'NONE',  ( 156.1449889021179160, 249.5000000000000568, 16.91223866672558529 ) ) ;
#79212 = DIRECTION ( 'NONE',  ( -1.000000000000000000, 0.000000000000000000, 0.000000000000000000 ) ) ;
#79213 = CARTESIAN_POINT ( 'NONE',  ( -38.39525521212431869, -293.0652040535756555, -345.3537221148486083 ) ) ;
#79214 = CARTESIAN_POINT ( 'NONE',  ( -110.0310385852859412, -282.7370229505635848, -293.6199233642132640 ) ) ;
#79215 = CARTESIAN_POINT ( 'NONE',  ( -92.82318459905957297, -280.8394905825547312, -221.6772668069955898 ) ) ;
#79216 = CARTESIAN_POINT ( 'NONE',  ( -112.1340618130393381, -285.5490890516229570, -286.9174265703881588 ) ) ;
#79217 = CARTESIAN_POINT ( 'NONE',  ( -11.82819930766667937, -278.6195267798581767, -198.7304837180949733 ) ) ;
#79218 = CARTESIAN_POINT ( 'NONE',  ( 29.96176989014811198, -287.1712389254042819, -241.9593260917929740 ) ) ;
#79219 = CARTESIAN_POINT ( 'NONE',  ( -74.29357734612666775, -278.9791120927117731, -334.0002072866249136 ) ) ;
#79220 = CARTESIAN_POINT ( 'NONE',  ( -85.59834137066741278, -280.1668156007853554, -215.3711343266621441 ) ) ;
#79221 = CARTESIAN_POINT ( 'NONE',  ( 1.863285120913890758, -288.5538547089687995, -206.0075948949304063 ) ) ;
#79222 = ORIENTED_EDGE ( 'NONE', *, *, #92101, .T. ) ;
#79223 = VECTOR ( 'NONE', #71373, 1000.000000000000000 ) ;
#79224 = CARTESIAN_POINT ( 'NONE',  ( -87.46065125704886611, -297.2089218747166797, -211.8349436728260571 ) ) ;
#79225 = CARTESIAN_POINT ( 'NONE',  ( 37.30014109282085855, -289.5406304514935982, -271.0262034806245310 ) ) ;
#79226 = DIRECTION ( 'NONE',  ( 0.9951408606192336803, 1.205805641958489930E-17, 0.09846150276128748380 ) ) ;
#79227 = CARTESIAN_POINT ( 'NONE',  ( 36.57525178469696669, -283.6233781216987495, -234.7283546768995564 ) ) ;
#79228 = ORIENTED_EDGE ( 'NONE', *, *, #60782, .T. ) ;
#79229 = CARTESIAN_POINT ( 'NONE',  ( -10.96646584678391179, -272.3948899111013588, -199.9184127489230889 ) ) ;
#79230 = CARTESIAN_POINT ( 'NONE',  ( 30.19937651941408419, -291.4908078802423574, -234.9679656265668939 ) ) ;
#79231 = VECTOR ( 'NONE', #57318, 1000.000000000000000 ) ;
#79232 = CARTESIAN_POINT ( 'NONE',  ( 35.20763525599286226, -289.2413003401826472, -283.2956333914979723 ) ) ;
#79233 = CARTESIAN_POINT ( 'NONE',  ( 21.30532312359792968, -282.6853001640905063, -225.1907700664478114 ) ) ;
#79234 = CARTESIAN_POINT ( 'NONE',  ( 32.16840943306019796, -288.5671842924766111, -238.5013208956435449 ) ) ;
#79235 = CARTESIAN_POINT ( 'NONE',  ( 35.48350285086903000, -289.1640813842440707, -293.8086782746200356 ) ) ;
#79236 = CARTESIAN_POINT ( 'NONE',  ( -111.9875524087367467, -286.6523929854164408, -262.5668472399709117 ) ) ;
#79237 = CARTESIAN_POINT ( 'NONE',  ( -104.9745736888721126, -278.2425155916996005, -307.1686500703929141 ) ) ;
#79238 = ORIENTED_EDGE ( 'NONE', *, *, #74086, .F. ) ;
#79239 = CARTESIAN_POINT ( 'NONE',  ( 37.18190053272848417, -291.7919480627124926, -282.9112189660622221 ) ) ;
#79240 = CARTESIAN_POINT ( 'NONE',  ( 22.87664135533223231, -280.7427912518157882, -222.3531636890328969 ) ) ;
#79241 = CIRCLE ( 'NONE', #14230, 35.00000000000003553 ) ;
#79242 = CARTESIAN_POINT ( 'NONE',  ( -81.82987380639806929, -275.2996919761560548, -210.8687624162998588 ) ) ;
#79243 = CARTESIAN_POINT ( 'NONE',  ( 35.78497577281001440, -284.2662352645559167, -287.0191576251351080 ) ) ;
#79244 = CARTESIAN_POINT ( 'NONE',  ( -8.060068942809543557, -272.6701934210207128, -200.1870704116645925 ) ) ;
#79245 = DIRECTION ( 'NONE',  ( 0.000000000000000000, 0.000000000000000000, 1.000000000000000000 ) ) ;
#79246 = CARTESIAN_POINT ( 'NONE',  ( -79.08489616690248170, -278.9795500921525218, -210.3986795233574298 ) ) ;
#79247 = AXIS2_PLACEMENT_3D ( 'NONE', #57189, #49132, #36316 ) ;
#79248 = CARTESIAN_POINT ( 'NONE',  ( 10.29121740237822813, -277.6169604270226614, -330.4214784075297757 ) ) ;
#79249 = CARTESIAN_POINT ( 'NONE',  ( -84.46597058586647222, -298.8141453474012224, -213.7730891900556571 ) ) ;
#79250 = CARTESIAN_POINT ( 'NONE',  ( -111.2681219997007815, -283.3509651492554440, -291.0421325272392323 ) ) ;
#79251 = CARTESIAN_POINT ( 'NONE',  ( -111.2590721523700523, -292.3730280653362570, -265.6937478498151677 ) ) ;
#79252 = CARTESIAN_POINT ( 'NONE',  ( -89.62888855191683035, -274.9301236646655298, -214.8589935751236339 ) ) ;
#79253 = CARTESIAN_POINT ( 'NONE',  ( -101.2270568954744334, -298.3163578548013106, -228.0682072674906635 ) ) ;
#79254 = CARTESIAN_POINT ( 'NONE',  ( 35.23007647460011071, -295.7873720894159533, -288.6194221403023903 ) ) ;
#79255 = CARTESIAN_POINT ( 'NONE',  ( -64.74997717118750984, -281.4107401076751671, -339.9945494405054660 ) ) ;
#79256 = CARTESIAN_POINT ( 'NONE',  ( -112.6183988753795262, -290.4210039483884316, -254.2004064992852079 ) ) ;
#79257 = CARTESIAN_POINT ( 'NONE',  ( -13.51712384418907220, -272.3831178840140979, -199.6204905742507663 ) ) ;
#79258 = CARTESIAN_POINT ( 'NONE',  ( 11.54852554760831751, -288.3171162900156901, -211.8441302997285334 ) ) ;
#79259 = TOROIDAL_SURFACE ( 'NONE', #62637, 1.500000000000001776, 0.5000000000000000000 ) ;
#79260 = CARTESIAN_POINT ( 'NONE',  ( -90.02896461324502297, -290.2059925061471404, -219.3878089412581858 ) ) ;
#79261 = VERTEX_POINT ( 'NONE', #44132 ) ;
#79262 = CARTESIAN_POINT ( 'NONE',  ( -113.5986427952308162, -289.1879564377489942, -265.5149868868106751 ) ) ;
#79263 = CARTESIAN_POINT ( 'NONE',  ( 29.44267672351397991, -287.6176442639592210, -300.0150900073157914 ) ) ;
#79264 = ORIENTED_EDGE ( 'NONE', *, *, #49823, .F. ) ;
#79265 = CARTESIAN_POINT ( 'NONE',  ( -36.58235796575990406, -287.1411389333542843, -193.6610016213380732 ) ) ;
#79266 = CARTESIAN_POINT ( 'NONE',  ( -71.66036869292177869, -277.8520523299818592, -334.8292086342329981 ) ) ;
#79267 = CARTESIAN_POINT ( 'NONE',  ( 21.97893736620609317, -291.8171726277817584, -221.7550023347215529 ) ) ;
#79268 = CARTESIAN_POINT ( 'NONE',  ( -111.0079393896297830, -284.9258550523901476, -292.4657919527791705 ) ) ;
#79269 = EDGE_CURVE ( 'NONE', #93327, #59332, #77224, .T. ) ;
#79270 = CARTESIAN_POINT ( 'NONE',  ( -73.60680702994881131, -285.9179544681879861, -202.4007802720128950 ) ) ;
#79271 = CARTESIAN_POINT ( 'NONE',  ( -54.50187413213997445, -280.1589559689548992, -199.3327404989723561 ) ) ;
#79272 = CARTESIAN_POINT ( 'NONE',  ( 168.3298383987194882, 232.4948596809232981, -192.7828393143454662 ) ) ;
#79273 = CARTESIAN_POINT ( 'NONE',  ( -104.9900673867532390, -255.0990985645446472, -326.1467328686887868 ) ) ;
#79274 = CARTESIAN_POINT ( 'NONE',  ( -107.0431942798137328, -259.6916240115564278, -315.7347989823788907 ) ) ;
#79275 = CARTESIAN_POINT ( 'NONE',  ( -32.67053191954658331, -273.3096596052347422, -197.3363601573703932 ) ) ;
#79276 = CARTESIAN_POINT ( 'NONE',  ( 31.41297026965077066, -274.1347254352875780, -244.9245031990116956 ) ) ;
#79277 = CARTESIAN_POINT ( 'NONE',  ( -27.76171907815665563, -294.4413865408643574, -346.7540745993601945 ) ) ;
#79278 = CARTESIAN_POINT ( 'NONE',  ( -110.4136115702177534, -272.0207119292052766, -270.3543514753225168 ) ) ;
#79279 = CARTESIAN_POINT ( 'NONE',  ( -57.97242737162893889, -272.4760277047526529, -196.6333199867409860 ) ) ;
#79280 = CARTESIAN_POINT ( 'NONE',  ( -96.28402587452860928, -299.0370821061700326, -225.2109424934774324 ) ) ;
#79281 = CARTESIAN_POINT ( 'NONE',  ( 36.12372930229673784, -288.9119491651757698, -273.7660875163248306 ) ) ;
#79282 = ORIENTED_EDGE ( 'NONE', *, *, #1109, .T. ) ;
#79283 = CARTESIAN_POINT ( 'NONE',  ( -113.7079270744290085, -297.3954088188022524, -278.1726219702486560 ) ) ;
#79284 = CARTESIAN_POINT ( 'NONE',  ( 22.03793322046877989, -287.4489908733972925, -227.7076796636168297 ) ) ;
#79285 = CARTESIAN_POINT ( 'NONE',  ( -89.94081171471141545, -272.2507554532513154, -214.4779847718323822 ) ) ;
#79286 = CARTESIAN_POINT ( 'NONE',  ( 36.54606754633113042, -294.0895197576217583, -249.2239446446268687 ) ) ;
#79287 = CARTESIAN_POINT ( 'NONE',  ( -79.43804899968603195, -296.0967265333636647, -334.7616173191334497 ) ) ;
#79288 = CARTESIAN_POINT ( 'NONE',  ( -37.55208115942573954, -292.2161625842783224, -197.3489774290588059 ) ) ;
#79289 = ORIENTED_EDGE ( 'NONE', *, *, #41709, .F. ) ;
#79290 = CARTESIAN_POINT ( 'NONE',  ( 1.653509048599000053, -276.4894406914506249, -205.6410449075851830 ) ) ;
#79291 = CARTESIAN_POINT ( 'NONE',  ( 37.20189734825071781, -274.5695240603387219, -288.0601536754574568 ) ) ;
#79292 = ADVANCED_FACE ( 'NONE', ( #43228 ), #2470, .F. ) ;
#79293 = ORIENTED_EDGE ( 'NONE', *, *, #68252, .F. ) ;
#79294 = CARTESIAN_POINT ( 'NONE',  ( -95.85492304601467595, -278.7343735814407637, -220.3836064735843649 ) ) ;
#79295 = CARTESIAN_POINT ( 'NONE',  ( 34.61832745809518741, -273.7376640446825036, -253.9278914373810494 ) ) ;
#79296 = CARTESIAN_POINT ( 'NONE',  ( -39.19364753710746641, -299.2335101995858508, -196.9749353761709472 ) ) ;
#79297 = AXIS2_PLACEMENT_3D ( 'NONE', #1151, #37131, #37578 ) ;
#79298 = CARTESIAN_POINT ( 'NONE',  ( 3.049753577997755372, -275.5501753835582690, -209.2109191504288788 ) ) ;
#79299 = CARTESIAN_POINT ( 'NONE',  ( 21.95335451253598436, -276.6670157383317701, -222.8213331975953224 ) ) ;
#79300 = CARTESIAN_POINT ( 'NONE',  ( -5.992532915547622352, -274.6622623917905912, -338.8858326596716211 ) ) ;
#79301 = CARTESIAN_POINT ( 'NONE',  ( -10.44478960713967730, -295.3430996826278943, -338.3350017373052765 ) ) ;
#79302 = CARTESIAN_POINT ( 'NONE',  ( 18.40703316846486715, -292.8057323675732277, -318.4162873627262229 ) ) ;
#79303 = CARTESIAN_POINT ( 'NONE',  ( 204.6539576904058606, 300.2961574867697436, 4.888549259831427740 ) ) ;
#79304 = CARTESIAN_POINT ( 'NONE',  ( -113.7043659784540779, -278.9216275648375927, -280.1778724609583264 ) ) ;
#79305 = CARTESIAN_POINT ( 'NONE',  ( -7.505709589569036666, -276.8163995321488642, -336.9855404799735084 ) ) ;
#79306 = AXIS2_PLACEMENT_3D ( 'NONE', #3730, #68594, #83243 ) ;
#79307 = CARTESIAN_POINT ( 'NONE',  ( -7.519800223873003731, -285.1197312858404302, -199.8494956847380877 ) ) ;
#79308 = CARTESIAN_POINT ( 'NONE',  ( -110.8077760466121617, -298.3486259274380359, -286.2596751496527645 ) ) ;
#79309 = CARTESIAN_POINT ( 'NONE',  ( 82.61719680589260406, -302.0442921925621818, -195.6390021813133160 ) ) ;
#79310 = AXIS2_PLACEMENT_3D ( 'NONE', #50546, #79443, #70936 ) ;
#79311 = CARTESIAN_POINT ( 'NONE',  ( 34.44060564382931489, -286.9362699305750084, -284.5645155065549261 ) ) ;
#79312 = CIRCLE ( 'NONE', #56607, 4.000000000000003553 ) ;
#79313 = CARTESIAN_POINT ( 'NONE',  ( -73.35440364028322335, -275.7765358487981757, -335.0368119225725536 ) ) ;
#79314 = CARTESIAN_POINT ( 'NONE',  ( -70.73628142453387113, -276.0763636839209312, -335.9368517470212510 ) ) ;
#79315 = CARTESIAN_POINT ( 'NONE',  ( 2.749136002822625269, -284.5149216349033736, -333.8072594197521994 ) ) ;
#79316 = CARTESIAN_POINT ( 'NONE',  ( -24.24375094371539063, -278.0864058131802494, -342.6317827543850854 ) ) ;
#79317 = DIRECTION ( 'NONE',  ( -0.000000000000000000, -0.000000000000000000, 1.000000000000000000 ) ) ;
#79319 = CARTESIAN_POINT ( 'NONE',  ( 13.44660569223658797, -273.1485362273969599, -213.4840009222043875 ) ) ;
#79318 = AXIS2_PLACEMENT_3D ( 'NONE', #63011, #4742, #69613 ) ;
#79320 = CARTESIAN_POINT ( 'NONE',  ( 35.80096514414278630, -276.2196051627906854, -271.5783972681992395 ) ) ;
#79321 = CARTESIAN_POINT ( 'NONE',  ( 10.34954366717665408, -284.3963923765912227, -328.5281780728930698 ) ) ;
#79322 = DIRECTION ( 'NONE',  ( -0.000000000000000000, 1.000000000000000000, -0.000000000000000000 ) ) ;
#79323 = CARTESIAN_POINT ( 'NONE',  ( -12.67036102426736299, -290.6541716096697883, -341.8347116628407321 ) ) ;
#79324 = CARTESIAN_POINT ( 'NONE',  ( 25.67196727737569972, -291.0028610460252025, -229.5940249424465947 ) ) ;
#79325 = VECTOR ( 'NONE', #58850, 1000.000000000000000 ) ;
#79326 = FACE_OUTER_BOUND ( 'NONE', #21978, .T. ) ;
#79327 = CARTESIAN_POINT ( 'NONE',  ( -105.8700488886609321, -271.5910814826529531, -243.6669348667808492 ) ) ;
#79328 = CARTESIAN_POINT ( 'NONE',  ( 9.648728131138632591, -290.8458101595338690, -212.8247370813005830 ) ) ;
#79329 = CARTESIAN_POINT ( 'NONE',  ( -71.74250447947856912, -195.9422791308210492, -360.7315132586310824 ) ) ;
#79330 = CARTESIAN_POINT ( 'NONE',  ( 209.4418336267437439, 29.74545085957678481, 14.26380412667039010 ) ) ;
#79331 = CARTESIAN_POINT ( 'NONE',  ( -99.31855673999471890, -288.4364252299862983, -314.8984196397925643 ) ) ;
#79332 = CARTESIAN_POINT ( 'NONE',  ( -106.9212331156635827, -285.8266585589992133, -295.1125431093550446 ) ) ;
#79333 = CARTESIAN_POINT ( 'NONE',  ( -111.5405219295187322, -282.5843521073865077, -286.7473579667551462 ) ) ;
#79334 = TOROIDAL_SURFACE ( 'NONE', #91387, 24.50000000000001066, 0.5000000000000000000 ) ;
#79335 = CARTESIAN_POINT ( 'NONE',  ( -26.63928815698761454, -284.3387630025928274, -343.2196550639237671 ) ) ;
#79336 = CARTESIAN_POINT ( 'NONE',  ( -107.5439860226457682, -285.0825507067057742, -291.0029320709091962 ) ) ;
#79337 = CARTESIAN_POINT ( 'NONE',  ( -112.5479154642533075, -292.5925726325560845, -265.6248773695701857 ) ) ;
#79338 = CARTESIAN_POINT ( 'NONE',  ( 24.46036004656913576, -275.2750418548525886, -224.4672224215528900 ) ) ;
#79339 = CARTESIAN_POINT ( 'NONE',  ( -109.0562938438775973, -288.9391456062112979, -246.3998300853839680 ) ) ;
#79340 = CARTESIAN_POINT ( 'NONE',  ( -48.49398732360806008, -277.1902394656632964, -346.6031117644668598 ) ) ;
#79341 = CARTESIAN_POINT ( 'NONE',  ( 34.19837377620675767, -295.2542288733499163, -248.8791137200036019 ) ) ;
#79342 = DIRECTION ( 'NONE',  ( -1.000000000000000000, 0.000000000000000000, 0.000000000000000000 ) ) ;
#79343 = CARTESIAN_POINT ( 'NONE',  ( 209.5577655351089561, 36.99254819693167917, 12.09245862089555423 ) ) ;
#79344 = CARTESIAN_POINT ( 'NONE',  ( -110.8125350698461062, -283.1939605091968133, -273.6435707378785764 ) ) ;
#79345 = CARTESIAN_POINT ( 'NONE',  ( 7.375061520024341455, -278.6611978120652680, -210.0851517577858090 ) ) ;
#79346 = CARTESIAN_POINT ( 'NONE',  ( -26.33290810456523801, -296.5876796138260829, -194.1640512332339767 ) ) ;
#79347 = CARTESIAN_POINT ( 'NONE',  ( 29.18224716367678084, -274.4912446551933272, -239.9325772984570904 ) ) ;
#79348 = CARTESIAN_POINT ( 'NONE',  ( 28.09337909425091340, -294.6156375422528413, -236.4648326735461694 ) ) ;
#79349 = CARTESIAN_POINT ( 'NONE',  ( 35.52818187999859134, -294.3908957125574375, -262.5649926542702133 ) ) ;
#79350 = CARTESIAN_POINT ( 'NONE',  ( 10.90041765718997091, -295.7162643014032142, -329.8095014548617314 ) ) ;
#79351 = CARTESIAN_POINT ( 'NONE',  ( -77.95150399151039267, -295.4477271009009200, -331.0838915039066137 ) ) ;
#79352 = CARTESIAN_POINT ( 'NONE',  ( -108.8515009288287700, -292.2585448295339461, -293.1457307293347867 ) ) ;
#79353 = CARTESIAN_POINT ( 'NONE',  ( -47.25425948742065430, -283.3414768375047288, -346.7204079965562755 ) ) ;
#79354 = CARTESIAN_POINT ( 'NONE',  ( 6.539205181120335553, -272.7806781962858054, -208.5328814618266620 ) ) ;
#79355 = CARTESIAN_POINT ( 'NONE',  ( 33.86023690505374617, -287.0113946112132339, -240.9082656323979279 ) ) ;
#79356 = CARTESIAN_POINT ( 'NONE',  ( -111.1138814072980949, -280.3852289015279666, -281.7414550896880314 ) ) ;
#79357 = EDGE_CURVE ( 'NONE', #44839, #35945, #17051, .T. ) ;
#79358 = CARTESIAN_POINT ( 'NONE',  ( -9.392535180193947397, -285.4853726225501305, -202.6552273925655356 ) ) ;
#79359 = CARTESIAN_POINT ( 'NONE',  ( -68.54896417137751996, -287.4620365862920721, -338.5741968564388458 ) ) ;
#79360 = CARTESIAN_POINT ( 'NONE',  ( -94.07136297056315755, -227.2831051785662737, -345.8935872616412439 ) ) ;
#79361 = CARTESIAN_POINT ( 'NONE',  ( -108.7236849902738811, -284.2658687704948761, -254.7270880068594465 ) ) ;
#79362 = CARTESIAN_POINT ( 'NONE',  ( 38.48044124476435002, -282.8943667953496970, -281.2703615932797447 ) ) ;
#79363 = CARTESIAN_POINT ( 'NONE',  ( -15.03212033496614453, -287.8289575683895123, -343.8680599547374186 ) ) ;
#79364 = CARTESIAN_POINT ( 'NONE',  ( -112.9262887534446804, -280.2795032123980832, -260.2939720749303660 ) ) ;
#79365 = CARTESIAN_POINT ( 'NONE',  ( -103.1728610879883519, -279.3550290190643750, -309.4464600763727162 ) ) ;
#79366 = CARTESIAN_POINT ( 'NONE',  ( -4.345669664768961660, -280.3329431615647422, -205.2299327592702127 ) ) ;
#79367 = CARTESIAN_POINT ( 'NONE',  ( 14.62405027875340835, -276.7680307453410933, -216.7756014152288060 ) ) ;
#79368 = CARTESIAN_POINT ( 'NONE',  ( 17.48960558643630492, -292.8090164105687450, -216.2256281858508657 ) ) ;
#79369 = CARTESIAN_POINT ( 'NONE',  ( 32.93976373489518750, -285.8997161556771403, -295.5079396244279906 ) ) ;
#79370 = CARTESIAN_POINT ( 'NONE',  ( -95.97647708291485458, -292.8136972994762459, -221.6747022778889118 ) ) ;
#79371 = CARTESIAN_POINT ( 'NONE',  ( -100.4395064246689344, -294.9606411727545492, -307.7825840145277425 ) ) ;
#79372 = CARTESIAN_POINT ( 'NONE',  ( -21.04970008677109661, -284.7617937203186216, -343.0494474300388106 ) ) ;
#79373 = CARTESIAN_POINT ( 'NONE',  ( -61.02403558633059077, -295.0347830011712063, -339.4888322163977818 ) ) ;
#79374 = CARTESIAN_POINT ( 'NONE',  ( -61.60387747519136070, -292.8239548325258852, -197.5532807902221180 ) ) ;
#79375 = TOROIDAL_SURFACE ( 'NONE', #62762, 5.654241149514405151, 1.000000000000000000 ) ;
#79376 = CARTESIAN_POINT ( 'NONE',  ( 34.16316661659890741, -282.0026176563101785, -255.1045770131308927 ) ) ;
#79377 = CARTESIAN_POINT ( 'NONE',  ( -68.73683545235036263, -272.7082355036955619, -200.2956032055256514 ) ) ;
#79378 = CARTESIAN_POINT ( 'NONE',  ( -14.97396002511934299, -289.4213663311979303, -343.9898697297467720 ) ) ;
#79379 = CARTESIAN_POINT ( 'NONE',  ( -69.96016351343914152, -281.6167039092179039, -338.7591289979116596 ) ) ;
#79380 = CARTESIAN_POINT ( 'NONE',  ( -87.36747178958346183, -290.0606781802754881, -328.9389609374773613 ) ) ;
#79381 = CARTESIAN_POINT ( 'NONE',  ( 16.90347899137946186, -287.1855028478344138, -221.4594488146300080 ) ) ;
#79382 = CARTESIAN_POINT ( 'NONE',  ( 195.3599902543797953, 284.4457220976750023, -111.0290403122453853 ) ) ;
#79383 = CARTESIAN_POINT ( 'NONE',  ( -47.65177483170455019, -155.1274943976620193, -361.2761651912329626 ) ) ;
#79384 = VECTOR ( 'NONE', #20206, 1000.000000000000000 ) ;
#79385 = CARTESIAN_POINT ( 'NONE',  ( -104.5864771384207188, -278.1356585658369340, -241.5385280345304579 ) ) ;
#79386 = CARTESIAN_POINT ( 'NONE',  ( -36.99311476855296377, -278.9769453226023188, -197.0528335737728298 ) ) ;
#79387 = CARTESIAN_POINT ( 'NONE',  ( -5.119248141194297830, -274.1315397973618246, -200.4507619572238752 ) ) ;
#79388 = CARTESIAN_POINT ( 'NONE',  ( 104.7727649842400837, 114.2745951806146110, -280.7604989259197623 ) ) ;
#79389 = CARTESIAN_POINT ( 'NONE',  ( -109.0469055283881517, -277.4648587663873514, -243.8082740606749894 ) ) ;
#79390 = CARTESIAN_POINT ( 'NONE',  ( -21.05331540121727230, -280.8623749884079643, -343.2602689546508259 ) ) ;
#79391 = CARTESIAN_POINT ( 'NONE',  ( -113.3248995114598188, -298.3214972268601173, -269.6348792102214702 ) ) ;
#79392 = CIRCLE ( 'NONE', #17327, 1.499999999999998002 ) ;
#79393 = CARTESIAN_POINT ( 'NONE',  ( -103.6147698734461642, -291.4592933310277658, -239.6061400442966374 ) ) ;
#79394 = CARTESIAN_POINT ( 'NONE',  ( -64.01539613199562950, -288.0921720306158136, -338.8974781640059177 ) ) ;
#79395 = CARTESIAN_POINT ( 'NONE',  ( 28.41107721460962665, -275.6812292215259390, -230.3859765899375986 ) ) ;
#79396 = CARTESIAN_POINT ( 'NONE',  ( 94.40783104291642758, -299.9133832367027139, -197.3573954632416019 ) ) ;
#79397 = ORIENTED_EDGE ( 'NONE', *, *, #35999, .T. ) ;
#79398 = DIRECTION ( 'NONE',  ( 1.000000000000000000, 0.000000000000000000, 0.000000000000000000 ) ) ;
#79399 = CARTESIAN_POINT ( 'NONE',  ( 208.6208076322478746, 32.98517505407394168, 15.00000000000000000 ) ) ;
#79400 = CARTESIAN_POINT ( 'NONE',  ( -64.25276690779156752, -281.6240354246907032, -199.7006295994097513 ) ) ;
#79401 = CARTESIAN_POINT ( 'NONE',  ( 33.40830374475189757, -282.3786859598549199, -251.1125251686990794 ) ) ;
#79402 = CARTESIAN_POINT ( 'NONE',  ( 19.35742575148746880, -282.6170543035222522, -219.7531905657830009 ) ) ;
#79403 = CARTESIAN_POINT ( 'NONE',  ( -87.09745701662976103, -282.8241301725437893, -324.1685124379164904 ) ) ;
#79404 = CARTESIAN_POINT ( 'NONE',  ( -101.6410646100322879, -279.9110861967631081, -307.5649388899048517 ) ) ;
#79405 = CARTESIAN_POINT ( 'NONE',  ( 17.81726478191379925, -273.3396443488283580, -221.4163044101814251 ) ) ;
#79406 = CARTESIAN_POINT ( 'NONE',  ( 208.4611680579919266, 29.54524714476348279, 14.80559097128782220 ) ) ;
#79407 = CARTESIAN_POINT ( 'NONE',  ( 143.6449502718966755, 0.000000000000000000, 21.50000000000000000 ) ) ;
#79408 = CARTESIAN_POINT ( 'NONE',  ( -39.94721566163005377, -277.8869032648578923, -347.1684933255999113 ) ) ;
#79409 = EDGE_CURVE ( 'NONE', #29328, #41863, #440, .T. ) ;
#79410 = VERTEX_POINT ( 'NONE', #88147 ) ;
#79411 = CARTESIAN_POINT ( 'NONE',  ( -45.60408299473439087, -275.7295098113027052, -346.3765204302799248 ) ) ;
#79412 = ORIENTED_EDGE ( 'NONE', *, *, #80614, .F. ) ;
#79413 = CARTESIAN_POINT ( 'NONE',  ( -74.94434090351494149, -280.8906705383787994, 22.50000000000000000 ) ) ;
#79414 = CARTESIAN_POINT ( 'NONE',  ( -82.86897144359556933, -285.6508145197346948, -330.4739166430243813 ) ) ;
#79415 = CARTESIAN_POINT ( 'NONE',  ( 34.22339607592780197, -292.9501780530105179, -285.6211290345370344 ) ) ;
#79416 = EDGE_CURVE ( 'NONE', #7995, #63355, #17132, .T. ) ;
#79417 = CARTESIAN_POINT ( 'NONE',  ( -1.855147741623635715, -287.9431019466036332, -338.5814770159034879 ) ) ;
#79418 = CARTESIAN_POINT ( 'NONE',  ( -92.25824581259320212, -283.4936551033919727, -220.6658124200015152 ) ) ;
#79419 = CARTESIAN_POINT ( 'NONE',  ( -106.1091574582985544, -283.4738900177623009, -244.1616575211198210 ) ) ;
#79420 = CARTESIAN_POINT ( 'NONE',  ( -45.66936229887300414, -284.3649897682299184, -343.3355026143385658 ) ) ;
#79421 = CARTESIAN_POINT ( 'NONE',  ( -62.85223850573094495, -271.7198730222474410, -199.8330166344707379 ) ) ;
#79422 = CARTESIAN_POINT ( 'NONE',  ( -109.9297475123722876, -282.6570294379390020, -293.5864144319137381 ) ) ;
#79423 = CARTESIAN_POINT ( 'NONE',  ( -111.6669986347971104, -298.4185626549921722, -280.7779907369480270 ) ) ;
#79424 = CARTESIAN_POINT ( 'NONE',  ( -59.93403078015445828, -283.7600525545510095, -198.6157637118226376 ) ) ;
#79425 = CARTESIAN_POINT ( 'NONE',  ( -100.7806809583330647, -278.9920702566289492, -307.0539792679182938 ) ) ;
#79426 = CARTESIAN_POINT ( 'NONE',  ( 198.4647887804454456, 289.5778437905237297, -6.693278644409265787 ) ) ;
#79427 = DIRECTION ( 'NONE',  ( 0.000000000000000000, -0.000000000000000000, 1.000000000000000000 ) ) ;
#79428 = CARTESIAN_POINT ( 'NONE',  ( 22.05517302192838969, -296.1089529876000483, -317.0865489651146163 ) ) ;
#79429 = PRODUCT_DEFINITION ( 'UNKNOWN', '', #28085, #76941 ) ;
#79430 = CARTESIAN_POINT ( 'NONE',  ( -92.45437388432198134, -275.8402696378829546, -321.3050878038019960 ) ) ;
#79431 = CARTESIAN_POINT ( 'NONE',  ( -113.6544393155528638, -289.6313493334585019, -279.7743230404922770 ) ) ;
#79432 = CARTESIAN_POINT ( 'NONE',  ( -67.64210029969706284, -293.8563418431681384, -337.6678152533099819 ) ) ;
#79433 = CARTESIAN_POINT ( 'NONE',  ( 5.222301536452737203, -279.3264045942776193, -210.4482709534483718 ) ) ;
#79434 = CARTESIAN_POINT ( 'NONE',  ( 53.58861941461584877, -297.3417089811084111, -196.1551220140682119 ) ) ;
#79435 = CARTESIAN_POINT ( 'NONE',  ( -37.56817119584607667, -293.3644705745486476, -196.8557868307845808 ) ) ;
#79436 = CARTESIAN_POINT ( 'NONE',  ( 175.2296996224750103, 20.99999999999998934, 0.000000000000000000 ) ) ;
#79437 = CARTESIAN_POINT ( 'NONE',  ( -90.24546155566609684, -294.2636173749046407, -325.4238810970804252 ) ) ;
#79438 = CARTESIAN_POINT ( 'NONE',  ( -61.49784179577256538, -290.9713933351055744, -340.0957667172688161 ) ) ;
#79439 = CARTESIAN_POINT ( 'NONE',  ( -41.96955562042941068, -290.2344377489041563, -194.5155052682038672 ) ) ;
#79440 = CARTESIAN_POINT ( 'NONE',  ( -53.52055227643713664, -290.6890838165340938, -342.1498333811127281 ) ) ;
#79441 = FACE_OUTER_BOUND ( 'NONE', #56591, .T. ) ;
#79442 = CARTESIAN_POINT ( 'NONE',  ( -8.144672649333537962, -289.4626710412791795, -337.4983290247773198 ) ) ;
#79443 = DIRECTION ( 'NONE',  ( -0.000000000000000000, -0.000000000000000000, 1.000000000000000000 ) ) ;
#79444 = CARTESIAN_POINT ( 'NONE',  ( -1.970357320849683846, -289.7992907308917552, -338.3087215288892367 ) ) ;
#79445 = CARTESIAN_POINT ( 'NONE',  ( -103.3406084486018273, -277.0536025502447046, -233.9942250622320046 ) ) ;
#79446 = CARTESIAN_POINT ( 'NONE',  ( -97.68296764298989387, -279.5252143768838664, -222.5628363568824284 ) ) ;
#79447 = CARTESIAN_POINT ( 'NONE',  ( 15.73588368284072025, -281.9917530765306424, -326.1151706447361676 ) ) ;
#79448 = CARTESIAN_POINT ( 'NONE',  ( 34.96402272740579065, -285.2957740353498934, -250.4391930447644654 ) ) ;
#79449 = CYLINDRICAL_SURFACE ( 'NONE', #58022, 6.154241149514405151 ) ;
#79450 = CARTESIAN_POINT ( 'NONE',  ( 26.61131017849629643, -280.2020895726905678, -308.1571762069452234 ) ) ;
#79451 = CARTESIAN_POINT ( 'NONE',  ( -97.71862719584134993, -283.1599014484700660, -225.7826997122473358 ) ) ;
#79452 = CARTESIAN_POINT ( 'NONE',  ( 155.4526335419784573, 18.61728136335971229, 8.651974842893862316 ) ) ;
#79453 = CARTESIAN_POINT ( 'NONE',  ( -111.0561816299742048, -277.2817698509196589, -250.5906054077842668 ) ) ;
#79454 = AXIS2_PLACEMENT_3D ( 'NONE', #61463, #26394, #38713 ) ;
#79455 = CARTESIAN_POINT ( 'NONE',  ( -112.8351764029676048, -283.2993139312862354, -284.1521504859274501 ) ) ;
#79456 = CARTESIAN_POINT ( 'NONE',  ( -92.14588786008734189, -274.0459058516042887, -221.8935748811241240 ) ) ;
#79457 = CARTESIAN_POINT ( 'NONE',  ( 151.0890045490263560, 131.0000000000000568, -11.50000000000000178 ) ) ;
#79458 = CARTESIAN_POINT ( 'NONE',  ( -105.4491481205933212, -292.5309694333656125, -241.8059414365591238 ) ) ;
#79459 = CARTESIAN_POINT ( 'NONE',  ( -38.36784355044866857, -275.4647907885492373, -193.9572350653712647 ) ) ;
#79460 = CARTESIAN_POINT ( 'NONE',  ( 33.26155244526208321, -275.4648697051891872, -288.9962518138122505 ) ) ;
#79461 = CARTESIAN_POINT ( 'NONE',  ( -81.30715076739113556, -297.6500928128484702, -331.1232755813418862 ) ) ;
#79462 = CARTESIAN_POINT ( 'NONE',  ( -14.95021994006125610, -288.9367112076967601, -344.0892635359948599 ) ) ;
#79463 = CARTESIAN_POINT ( 'NONE',  ( 37.44249742371568601, -279.7696412526656218, -281.1610251400859397 ) ) ;
#79464 = CARTESIAN_POINT ( 'NONE',  ( 23.97651662818807949, -292.7646071751225918, -223.7660767972780320 ) ) ;
#79465 = CARTESIAN_POINT ( 'NONE',  ( -72.73016753408175816, -290.6303589779037111, -206.1865495274964246 ) ) ;
#79466 = CARTESIAN_POINT ( 'NONE',  ( -39.08749757054280138, -293.0739058145688887, -345.3408008541252343 ) ) ;
#79467 = VERTEX_POINT ( 'NONE', #9070 ) ;
#79468 = CARTESIAN_POINT ( 'NONE',  ( 197.1180234003297755, 72.74234001486334478, 12.08831112423764509 ) ) ;
#79469 = CARTESIAN_POINT ( 'NONE',  ( -67.82115183211701037, -291.1486429749041918, -203.9471358221020409 ) ) ;
#79470 = FACE_OUTER_BOUND ( 'NONE', #64171, .T. ) ;
#79471 = CARTESIAN_POINT ( 'NONE',  ( 2.608298161699547535, -287.5153819974877933, -204.8110009010750332 ) ) ;
#79472 = CARTESIAN_POINT ( 'NONE',  ( 90.32002540683689062, -302.2645883696979467, -200.3030568020284647 ) ) ;
#79473 = CARTESIAN_POINT ( 'NONE',  ( -30.62351921889639073, -294.0279162252280685, -346.8312837867644589 ) ) ;
#79474 = CARTESIAN_POINT ( 'NONE',  ( -89.56195626523414433, -286.6499411597344533, -214.3753366125651496 ) ) ;
#79475 = CARTESIAN_POINT ( 'NONE',  ( -100.9902799089257144, -284.8758363197011363, -234.5103852853930562 ) ) ;
#79476 = CARTESIAN_POINT ( 'NONE',  ( 35.52432281150923643, -276.9272797100709909, -259.2649807279888137 ) ) ;
#79477 = CARTESIAN_POINT ( 'NONE',  ( 17.34743313830938760, -292.2864250787960145, -321.1641248401943471 ) ) ;
#79478 = CARTESIAN_POINT ( 'NONE',  ( -31.50032385928852463, -296.7376799605291353, -344.1943929307040548 ) ) ;
#79479 = CARTESIAN_POINT ( 'NONE',  ( 13.99816718743864286, -275.1072423954169608, -322.8851838525761195 ) ) ;
#79480 = EDGE_LOOP ( 'NONE', ( #34055, #90355, #70886, #9965 ) ) ;
#79481 = DIRECTION ( 'NONE',  ( 1.000000000000000000, 0.000000000000000000, 0.000000000000000000 ) ) ;
#79482 = CARTESIAN_POINT ( 'NONE',  ( -5.810244013500115656, -294.3155083128707474, -340.5858398895014147 ) ) ;
#79483 = CARTESIAN_POINT ( 'NONE',  ( 36.41967353032591603, -289.3377154872188157, -259.9568605048786480 ) ) ;
#79484 = CARTESIAN_POINT ( 'NONE',  ( -11.03739043055442082, -296.3812685058572356, -195.3700774844024579 ) ) ;
#79485 = CARTESIAN_POINT ( 'NONE',  ( 30.43485240474585041, -299.9617133597211023, -193.6581076686333063 ) ) ;
#79486 = CARTESIAN_POINT ( 'NONE',  ( -60.01811337110007116, -286.4017656522879065, -200.8652695422702266 ) ) ;
#79487 = ORIENTED_EDGE ( 'NONE', *, *, #19203, .F. ) ;
#79488 = CARTESIAN_POINT ( 'NONE',  ( -97.50499473779819937, -278.2508875643740112, -222.6830496920694600 ) ) ;
#79489 = CARTESIAN_POINT ( 'NONE',  ( -33.43171266986855272, -295.6555849904203228, -347.1728187782676969 ) ) ;
#79490 = CARTESIAN_POINT ( 'NONE',  ( -40.31440192102420639, -287.2287054857509929, -346.0804525038054180 ) ) ;
#79491 = CARTESIAN_POINT ( 'NONE',  ( -113.5814117173243858, -297.0197540410792385, -259.6237987697339804 ) ) ;
#79492 = CARTESIAN_POINT ( 'NONE',  ( 4.512289767942923469, -292.9673261411324461, -210.4632696967629784 ) ) ;
#79493 = DIRECTION ( 'NONE',  ( 0.000000000000000000, 0.000000000000000000, 1.000000000000000000 ) ) ;
#79494 = FACE_OUTER_BOUND ( 'NONE', #60534, .T. ) ;
#79495 = CARTESIAN_POINT ( 'NONE',  ( 38.91249631477773363, -289.1228280746155406, -274.3670598194632362 ) ) ;
#79496 = CARTESIAN_POINT ( 'NONE',  ( -72.02372285203398405, -289.1237833571631768, -198.2697987213421698 ) ) ;
#79497 = VERTEX_POINT ( 'NONE', #59777 ) ;
#79498 = CARTESIAN_POINT ( 'NONE',  ( -79.84752079386599632, -278.8425664068086007, -206.2147377848810947 ) ) ;
#79499 = CARTESIAN_POINT ( 'NONE',  ( -97.37770050020036194, -285.9409996979936750, -315.0344555408725000 ) ) ;
#79500 = CARTESIAN_POINT ( 'NONE',  ( -107.3787279982790608, -283.5208898756325766, -239.6769524679706365 ) ) ;
#79501 = CARTESIAN_POINT ( 'NONE',  ( -0.2956276393937394831, -286.6357093279124229, -334.9874812043945553 ) ) ;
#79502 = CARTESIAN_POINT ( 'NONE',  ( 36.39530495606224036, -277.6345195464417657, -287.8285537934423814 ) ) ;
#79503 = CARTESIAN_POINT ( 'NONE',  ( -41.87842166316425363, -298.4857907140830093, -197.4405680706571786 ) ) ;
#79504 = EDGE_LOOP ( 'NONE', ( #65039, #55876, #29734, #64968 ) ) ;
#79505 = CARTESIAN_POINT ( 'NONE',  ( 19.20185852387434622, -292.8984066857074140, -317.3086360680122766 ) ) ;
#79507 = CARTESIAN_POINT ( 'NONE',  ( -103.4585046167218394, -278.3229335873307946, -239.0578632570020545 ) ) ;
#79506 = CARTESIAN_POINT ( 'NONE',  ( -107.6183121957091231, -278.8138106119273516, -250.5613630033358561 ) ) ;
#79508 = CARTESIAN_POINT ( 'NONE',  ( -49.68310194708145389, -274.9780957396689587, -194.6161652946820197 ) ) ;
#79509 = CARTESIAN_POINT ( 'NONE',  ( -42.38849121500016537, -278.7847612117595872, -193.9246174181442939 ) ) ;
#79510 = CARTESIAN_POINT ( 'NONE',  ( -57.17162103437372878, -168.6543081016745020, -361.5809719840890466 ) ) ;
#79511 = CARTESIAN_POINT ( 'NONE',  ( -104.7424857350691951, -298.4474415156828400, -234.2524315420578205 ) ) ;
#79512 = CARTESIAN_POINT ( 'NONE',  ( 157.1811243746104196, 250.0348692542015954, 16.89756558802390529 ) ) ;
#79513 = ORIENTED_EDGE ( 'NONE', *, *, #32042, .F. ) ;
#79514 = CARTESIAN_POINT ( 'NONE',  ( 82.68073018288104947, -297.0543924324409204, -195.4120394483015559 ) ) ;
#79515 = CARTESIAN_POINT ( 'NONE',  ( -19.75495865843054943, -287.3633154671680359, -199.1927781317019708 ) ) ;
#79516 = CARTESIAN_POINT ( 'NONE',  ( -89.21112516047233498, -287.0948367177936689, -214.7599300756371576 ) ) ;
#79517 = CARTESIAN_POINT ( 'NONE',  ( 21.25021873354771174, -287.5134888657170791, -314.0956793298481671 ) ) ;
#79518 = CARTESIAN_POINT ( 'NONE',  ( 0.8323737669285214968, -282.0648062477305302, -337.1765393366437138 ) ) ;
#79519 = CARTESIAN_POINT ( 'NONE',  ( -101.2860737566626881, -276.4510990783794000, -307.3088494285454999 ) ) ;
#79520 = CARTESIAN_POINT ( 'NONE',  ( -111.5525416636177596, -286.3690393845018889, -273.7172119853556183 ) ) ;
#79521 = CARTESIAN_POINT ( 'NONE',  ( -83.86055731133599522, -277.8801077595737183, -213.1400002179955777 ) ) ;
#79522 = CARTESIAN_POINT ( 'NONE',  ( -102.2849350589290225, -279.4018251965210879, -304.7648926796004503 ) ) ;
#79523 = CARTESIAN_POINT ( 'NONE',  ( 13.53501927138226613, -275.2807254340241911, -217.9249866920037562 ) ) ;
#79524 = CARTESIAN_POINT ( 'NONE',  ( -3.251298052482054057, -287.4069614254707972, -338.9748915458093279 ) ) ;
#79525 = CARTESIAN_POINT ( 'NONE',  ( -88.20697334313787508, -284.5456590274911264, -328.0245384175451022 ) ) ;
#79526 = CARTESIAN_POINT ( 'NONE',  ( 37.13381725701844260, -282.2863879334347530, -289.6723637645936265 ) ) ;
#79527 = ORIENTED_EDGE ( 'NONE', *, *, #23558, .F. ) ;
#79528 = ORIENTED_EDGE ( 'NONE', *, *, #5542, .F. ) ;
#79529 = PLANE ( 'NONE',  #92713 ) ;
#79530 = CARTESIAN_POINT ( 'NONE',  ( -82.10351036824796722, -291.5158110587657347, -331.4895550801701916 ) ) ;
#79531 = CARTESIAN_POINT ( 'NONE',  ( -108.3470402139863893, -288.8731267976909862, -298.8486582580608797 ) ) ;
#79532 = CARTESIAN_POINT ( 'NONE',  ( -89.40103400258027477, -272.3551393946534631, -218.8515634852495282 ) ) ;
#79533 = CARTESIAN_POINT ( 'NONE',  ( -2.021693309433206132, -293.9454070276229345, -338.6678519497706361 ) ) ;
#79534 = CARTESIAN_POINT ( 'NONE',  ( -69.07390035720762000, -287.9571776946671093, -336.8725848386332018 ) ) ;
#79535 = CARTESIAN_POINT ( 'NONE',  ( 35.21425320698516970, -291.6018483156392449, -255.7457954937454190 ) ) ;
#79536 = CARTESIAN_POINT ( 'NONE',  ( 18.13568770314636680, -289.4390346597742223, -318.4933462508482194 ) ) ;
#79537 = CARTESIAN_POINT ( 'NONE',  ( 21.31550574532285580, -296.6948066931273615, -317.0979686699210447 ) ) ;
#79538 = CARTESIAN_POINT ( 'NONE',  ( 20.86940451829296350, -290.2038471250402836, -317.6726484382376157 ) ) ;
#79539 = CARTESIAN_POINT ( 'NONE',  ( -80.84802470311109346, -289.4629772922522193, -209.0648852606259425 ) ) ;
#79540 = CARTESIAN_POINT ( 'NONE',  ( -110.1219492398727624, -292.7855442334407030, -252.1975282590965719 ) ) ;
#79541 = CARTESIAN_POINT ( 'NONE',  ( -97.55621111271682366, -286.0725461758831329, -228.6541632731328377 ) ) ;
#79542 = CARTESIAN_POINT ( 'NONE',  ( -41.96721188365903998, -293.9941322660226888, -195.3369014338937575 ) ) ;
#79543 = CARTESIAN_POINT ( 'NONE',  ( 121.3887860922853150, -299.5541904835127980, -197.6024395396064222 ) ) ;
#79544 = CARTESIAN_POINT ( 'NONE',  ( -112.5415345926156050, -274.6034480829973745, -264.7738583930552636 ) ) ;
#79545 = CARTESIAN_POINT ( 'NONE',  ( 20.30189504774060794, -281.3829770374169357, -315.4146157683587148 ) ) ;
#79546 = CARTESIAN_POINT ( 'NONE',  ( -2.720183057619603773, -280.5943139236004527, -336.9063337629759758 ) ) ;
#79547 = CARTESIAN_POINT ( 'NONE',  ( -95.46606251925892650, -295.0690040304389186, -320.6176331570524098 ) ) ;
#79548 = CARTESIAN_POINT ( 'NONE',  ( 35.37319440412365879, -273.6124190639771996, -256.5582875287274192 ) ) ;
#79549 = CARTESIAN_POINT ( 'NONE',  ( -88.09483948869231540, -275.8489468249696870, -324.8169077653797672 ) ) ;
#79550 = CARTESIAN_POINT ( 'NONE',  ( -109.8467178981870518, -297.7099477150993607, -282.3721910716241723 ) ) ;
#79551 = CARTESIAN_POINT ( 'NONE',  ( 32.10208298100891255, -295.3006056983235226, -294.8640815932949408 ) ) ;
#79552 = DIRECTION ( 'NONE',  ( -0.000000000000000000, 1.000000000000000000, -0.000000000000000000 ) ) ;
#79553 = CARTESIAN_POINT ( 'NONE',  ( 18.96390443441587337, -295.0160705867976958, -317.0760044998428953 ) ) ;
#79554 = LINE ( 'NONE', #21313, #11217 ) ;
#79556 = CARTESIAN_POINT ( 'NONE',  ( -77.51197591391908759, -297.4968279394936985, -209.3467125891144747 ) ) ;
#79555 = CARTESIAN_POINT ( 'NONE',  ( -24.05069231370500660, -284.2410579614560788, -196.1342339643691162 ) ) ;
#79557 = CARTESIAN_POINT ( 'NONE',  ( -113.8196391722676992, -284.6640998759768308, -261.4098700498012136 ) ) ;
#79558 = CARTESIAN_POINT ( 'NONE',  ( 23.26818510146473429, -287.8535928152922452, -317.8395440983318281 ) ) ;
#79559 = CARTESIAN_POINT ( 'NONE',  ( 24.87940633120200218, -290.9887891372476361, -228.7851352809141190 ) ) ;
#79560 = CARTESIAN_POINT ( 'NONE',  ( -97.56395413642863446, -278.3892845631813202, -222.6385976849548456 ) ) ;
#79561 = CARTESIAN_POINT ( 'NONE',  ( -69.85430415644619018, -277.1237833571632905, -202.7746430608542312 ) ) ;
#79562 = CARTESIAN_POINT ( 'NONE',  ( 154.7381521964376816, 128.4861308677327258, 12.50226176572442860 ) ) ;
#79563 = CARTESIAN_POINT ( 'NONE',  ( 35.35151333689758957, -286.4813149617853583, -280.5928645412478772 ) ) ;
#79565 = CARTESIAN_POINT ( 'NONE',  ( 197.2511406043087163, 71.96799660027704704, -11.91673342594003060 ) ) ;
#79564 = CARTESIAN_POINT ( 'NONE',  ( -89.29222824684700299, -288.6836798894306071, -326.7759665353119658 ) ) ;
#79566 = DIRECTION ( 'NONE',  ( -0.8660254037844413721, 0.4999999999999951705, 0.000000000000000000 ) ) ;
#79567 = CARTESIAN_POINT ( 'NONE',  ( -111.1842766871718311, -298.1374858967251384, -271.4955286000169963 ) ) ;
#79568 = CARTESIAN_POINT ( 'NONE',  ( 1.062004353205869611, -281.9791353082589467, -204.2421091608420625 ) ) ;
#79570 = CARTESIAN_POINT ( 'NONE',  ( 20.19500995666101772, -281.8524524261554802, -315.3234853523587162 ) ) ;
#79569 = CARTESIAN_POINT ( 'NONE',  ( -92.50301739849227545, -293.8570454071830227, -321.7185741260280452 ) ) ;
#79571 = CARTESIAN_POINT ( 'NONE',  ( -1.965589941400027074, -294.7633679942503591, -338.7535944151754279 ) ) ;
#79572 = CARTESIAN_POINT ( 'NONE',  ( 20.99431466043375494, -284.9745315258292635, -222.3379612728367078 ) ) ;
#79573 = CARTESIAN_POINT ( 'NONE',  ( -45.09268746682259632, -281.9542883499210006, -195.7110931146172277 ) ) ;
#79574 = CARTESIAN_POINT ( 'NONE',  ( -95.46853083156980802, -296.2358674631373674, -225.7909410050751546 ) ) ;
#79575 = CARTESIAN_POINT ( 'NONE',  ( 186.6539576904058890, 276.0000000000000568, -11.60392986742922439 ) ) ;
#79576 = CARTESIAN_POINT ( 'NONE',  ( -56.72219377252064021, -285.2831572637023783, -342.4460905212382613 ) ) ;
#79577 = LINE ( 'NONE', #92832, #23200 ) ;
#79578 = CARTESIAN_POINT ( 'NONE',  ( -20.25526795762938548, -292.3380690714490129, -345.3683826091709648 ) ) ;
#79579 = CARTESIAN_POINT ( 'NONE',  ( 14.76615024828351785, -275.5377154271676545, -326.9041442237817137 ) ) ;
#79580 = EDGE_CURVE ( 'NONE', #557, #24392, #8619, .T. ) ;
#79581 = EDGE_CURVE ( 'NONE', #6151, #59355, #76057, .T. ) ;
#79582 = CARTESIAN_POINT ( 'NONE',  ( -22.73855337868598170, -292.0776122451333094, -198.8366598615854741 ) ) ;
#79583 = CARTESIAN_POINT ( 'NONE',  ( 19.90275384531025438, -283.7229086799844708, -316.7898524526663664 ) ) ;
#79584 = VECTOR ( 'NONE', #16011, 1000.000000000000000 ) ;
#79585 = CARTESIAN_POINT ( 'NONE',  ( -91.72570709149921697, -274.8606373358587120, -220.4543281199715068 ) ) ;
#79586 = CARTESIAN_POINT ( 'NONE',  ( -31.67523405404176629, -284.5819051385494163, -346.3632708633675179 ) ) ;
#79587 = CARTESIAN_POINT ( 'NONE',  ( 31.72304525629968808, -280.6779260165739629, -295.3546399174426824 ) ) ;
#79588 = CARTESIAN_POINT ( 'NONE',  ( -94.22740690673346364, -279.8749314897559657, -319.2386896866080974 ) ) ;
#79589 = CARTESIAN_POINT ( 'NONE',  ( -96.02906609762931112, -273.3909868535999408, -220.4931173927418513 ) ) ;
#79590 = CARTESIAN_POINT ( 'NONE',  ( 36.49285885468430735, -275.6601306437435142, -292.2584432589188168 ) ) ;
#79591 = CARTESIAN_POINT ( 'NONE',  ( 37.05982424243434536, -295.4413531459576348, -267.9679263101124889 ) ) ;
#79592 = DIRECTION ( 'NONE',  ( 0.000000000000000000, -1.000000000000000000, 0.000000000000000000 ) ) ;
#79593 = CYLINDRICAL_SURFACE ( 'NONE', #55702, 1.000000000000000888 ) ;
#79594 = CARTESIAN_POINT ( 'NONE',  ( -55.79277367233232354, -293.4268250844205568, -343.8448805623857538 ) ) ;
#79595 = CARTESIAN_POINT ( 'NONE',  ( -83.22436863694792919, -272.9113761493084098, -213.5036719270056267 ) ) ;
#79596 = CARTESIAN_POINT ( 'NONE',  ( 19.84612272703604319, -294.3817145478230941, -219.8214794834491670 ) ) ;
#79598 = CARTESIAN_POINT ( 'NONE',  ( 20.99802122446750730, -294.0842113561472502, -220.6974977267844338 ) ) ;
#79597 = CARTESIAN_POINT ( 'NONE',  ( -20.19161114001083490, -279.3376638359844719, -345.3538533559490702 ) ) ;
#79599 = CARTESIAN_POINT ( 'NONE',  ( 24.27352756056665939, -290.1295099026854132, -312.8524350575557378 ) ) ;
#79600 = CARTESIAN_POINT ( 'NONE',  ( -97.58364759989588322, -275.9448053341776586, -314.7778331508105794 ) ) ;
#79601 = CARTESIAN_POINT ( 'NONE',  ( -40.54370668040117209, -279.0128535269700478, -344.7449340695518458 ) ) ;
#79602 = CARTESIAN_POINT ( 'NONE',  ( 35.63289677954256973, -291.4418613509101306, -255.6634172456244016 ) ) ;
#79603 = CARTESIAN_POINT ( 'NONE',  ( 36.93930066030053183, -283.6022140628785451, -285.2821905059549863 ) ) ;
#79604 = VERTEX_POINT ( 'NONE', #74414 ) ;
#79605 = CARTESIAN_POINT ( 'NONE',  ( 13.93650831662567136, -281.9753456912669094, -322.4191590847545399 ) ) ;
#79606 = CARTESIAN_POINT ( 'NONE',  ( -22.63896580860269836, -281.3156362531685772, -195.0387478172308136 ) ) ;
#79607 = CARTESIAN_POINT ( 'NONE',  ( -94.11523753974346107, -282.6446987398844612, -321.8079452693061739 ) ) ;
#79608 = CARTESIAN_POINT ( 'NONE',  ( -67.28177619227146522, -280.6102570590668392, -199.6758149938056590 ) ) ;
#79609 = CARTESIAN_POINT ( 'NONE',  ( 0.000000000000000000, 0.000000000000000000, 0.000000000000000000 ) ) ;
#79610 = CARTESIAN_POINT ( 'NONE',  ( 37.26339210323240536, -276.8692583411929604, -254.2748135917506431 ) ) ;
#79611 = CARTESIAN_POINT ( 'NONE',  ( -37.37352853689063181, -294.5519495502701375, -200.3611179825600459 ) ) ;
#79612 = ORIENTED_EDGE ( 'NONE', *, *, #2190, .T. ) ;
#79613 = CARTESIAN_POINT ( 'NONE',  ( -96.06687529340298681, -275.1907627728191983, -223.9781228983767676 ) ) ;
#79614 = CARTESIAN_POINT ( 'NONE',  ( -109.7741328044625675, -276.3388494539403268, -288.4524396009228440 ) ) ;
#79615 = CARTESIAN_POINT ( 'NONE',  ( -96.68640816631436508, -292.9564122111787583, -222.9039831579609086 ) ) ;
#79616 = CARTESIAN_POINT ( 'NONE',  ( 24.93905780996364285, -292.3727207543104214, -231.9896871885923417 ) ) ;
#79617 = CARTESIAN_POINT ( 'NONE',  ( -78.10912060702612791, -289.0919170742120627, -335.6731290785575084 ) ) ;
#79618 = CARTESIAN_POINT ( 'NONE',  ( 208.4455020912638190, 36.83759663588386246, 13.33594775738876592 ) ) ;
#79620 = CARTESIAN_POINT ( 'NONE',  ( -86.24114712889522139, -283.7605477729562153, -215.0182048886497057 ) ) ;
#79619 = CARTESIAN_POINT ( 'NONE',  ( 38.02209382081370848, -292.2867499065621928, -283.0460330747451962 ) ) ;
#79621 = CARTESIAN_POINT ( 'NONE',  ( -92.60832229505459168, -293.1102152680060158, -220.7793498180965912 ) ) ;
#79622 = CARTESIAN_POINT ( 'NONE',  ( -42.70545745607833510, -284.4631602039098652, -196.8504959044786062 ) ) ;
#79623 = CARTESIAN_POINT ( 'NONE',  ( -40.23713293684328818, -284.4044841459769941, -343.7972122950033054 ) ) ;
#79624 = EDGE_LOOP ( 'NONE', ( #10573, #79744, #59684, #36471 ) ) ;
#79625 = CARTESIAN_POINT ( 'NONE',  ( -89.32332170511958225, -290.7042778291437344, -326.8476759466742010 ) ) ;
#79626 = CARTESIAN_POINT ( 'NONE',  ( 33.51372565921600000, -281.8089371671240428, -252.4918588979496121 ) ) ;
#79627 = CARTESIAN_POINT ( 'NONE',  ( 0.3317800932513300660, -293.3568510374392417, -337.0749254412979212 ) ) ;
#79628 = CARTESIAN_POINT ( 'NONE',  ( 28.77002472021120383, -288.8662186069650488, -309.5197525057987491 ) ) ;
#79629 = CARTESIAN_POINT ( 'NONE',  ( 37.44608017412164003, -288.2712568113029192, -288.4809795075651664 ) ) ;
#79630 = CARTESIAN_POINT ( 'NONE',  ( -25.14390984947545249, -286.3785701115285178, -198.3361171684697695 ) ) ;
#79631 = ORIENTED_EDGE ( 'NONE', *, *, #61955, .F. ) ;
#79632 = CARTESIAN_POINT ( 'NONE',  ( 37.14728970841045452, -295.5894356295896159, -284.2767623477607799 ) ) ;
#79633 = CARTESIAN_POINT ( 'NONE',  ( -65.43808186185871989, -294.0966975383515205, -341.5362761815433714 ) ) ;
#79634 = CARTESIAN_POINT ( 'NONE',  ( -108.9974715653428206, -277.4119744527378089, -285.4892001009048954 ) ) ;
#79635 = CARTESIAN_POINT ( 'NONE',  ( -113.4824750946428367, -272.2026622434643741, -258.9476367018966130 ) ) ;
#79636 = CARTESIAN_POINT ( 'NONE',  ( -73.66080764165454298, -294.0235084408667490, -334.4831125120363708 ) ) ;
#79637 = CARTESIAN_POINT ( 'NONE',  ( 12.44570241331270211, -278.1078145747293320, -325.1955301150332502 ) ) ;
#79638 = CARTESIAN_POINT ( 'NONE',  ( -107.4655436004293705, -271.0103491353746108, -245.9990151154011926 ) ) ;
#79639 = CARTESIAN_POINT ( 'NONE',  ( 4.718694414574347462, -293.8389803564352860, -210.1485648752665725 ) ) ;
#79640 = CARTESIAN_POINT ( 'NONE',  ( -108.2651507527501451, -297.3873591156042266, -288.9603827133764753 ) ) ;
#79641 = DIRECTION ( 'NONE',  ( 0.000000000000000000, -0.000000000000000000, 1.000000000000000000 ) ) ;
#79642 = CARTESIAN_POINT ( 'NONE',  ( -84.05664340632368692, -295.4115979760393316, -211.4735768728311029 ) ) ;
#79643 = CARTESIAN_POINT ( 'NONE',  ( -62.81910683683614138, -298.3804075915904832, -197.8062109545585656 ) ) ;
#79644 = CARTESIAN_POINT ( 'NONE',  ( -67.89496029504422836, -275.6512994793333746, -201.8525297004382253 ) ) ;
#79645 = CARTESIAN_POINT ( 'NONE',  ( -61.32077575071903652, -290.3126231363195302, -339.5594733111145160 ) ) ;
#79646 = CARTESIAN_POINT ( 'NONE',  ( -67.30000412886899142, -295.7894387049378224, -336.9675262229276314 ) ) ;
#79647 = CARTESIAN_POINT ( 'NONE',  ( -112.1305238194655658, -280.4089327076480913, -279.9947798280949200 ) ) ;
#79648 = CARTESIAN_POINT ( 'NONE',  ( -45.20591423952502197, -278.6394883062625354, -194.2068746254713290 ) ) ;
#79649 = ORIENTED_EDGE ( 'NONE', *, *, #82838, .T. ) ;
#79650 = CARTESIAN_POINT ( 'NONE',  ( 4.483289176046659996, -281.8527107205018751, -334.9529805667808091 ) ) ;
#79651 = CARTESIAN_POINT ( 'NONE',  ( 25.24876753940065655, -274.3079567936619014, -225.6648140162351126 ) ) ;
#79652 = CARTESIAN_POINT ( 'NONE',  ( -109.8331002845297917, -282.4124491934122148, -287.3376217508055106 ) ) ;
#79653 = CARTESIAN_POINT ( 'NONE',  ( -73.36922729722932957, -277.9823837530858555, -203.2012746820324196 ) ) ;
#79654 = CARTESIAN_POINT ( 'NONE',  ( 15.94192959134534782, -278.8044777035839843, -217.2703431897868711 ) ) ;
#79655 = CARTESIAN_POINT ( 'NONE',  ( -88.45678501247394365, -296.0024583026014398, -217.4839132598680465 ) ) ;
#79656 = CARTESIAN_POINT ( 'NONE',  ( 33.83537121001608483, -277.8596818949843055, -294.1609525081875063 ) ) ;
#79657 = CARTESIAN_POINT ( 'NONE',  ( 196.0143093133015384, 24.42324672360809856, 11.99999999999998934 ) ) ;
#79658 = CARTESIAN_POINT ( 'NONE',  ( -1.562116348872140792, -290.5441865549014437, -204.0419790453083237 ) ) ;
#79659 = CARTESIAN_POINT ( 'NONE',  ( -71.90646914995376449, -289.4964572090494244, -339.1671986910600367 ) ) ;
#79660 = CARTESIAN_POINT ( 'NONE',  ( 32.01191956623917179, -277.1731482208267607, -241.2422513616602373 ) ) ;
#79661 = CIRCLE ( 'NONE', #35639, 4.999999999999990230 ) ;
#79662 = CARTESIAN_POINT ( 'NONE',  ( -85.22895706849492115, -295.3892637488935975, -212.7883595114597597 ) ) ;
#79663 = CARTESIAN_POINT ( 'NONE',  ( -113.7443915820733196, -283.6469002057568787, -278.5334835406822549 ) ) ;
#79664 = CARTESIAN_POINT ( 'NONE',  ( 209.6607606054017197, 36.26300151376644010, 14.77867248455306104 ) ) ;
#79665 = CARTESIAN_POINT ( 'NONE',  ( -98.71588300517325365, -283.1375780708503953, -227.2320419190264715 ) ) ;
#79666 = DIRECTION ( 'NONE',  ( 0.000000000000000000, 1.000000000000000000, 0.000000000000000000 ) ) ;
#79667 = CARTESIAN_POINT ( 'NONE',  ( 20.50527407133458269, -291.7135437508745781, -225.1649086648845639 ) ) ;
#79668 = CARTESIAN_POINT ( 'NONE',  ( -68.03717204446434152, -283.7843552954169013, -202.7693027462782425 ) ) ;
#79669 = CARTESIAN_POINT ( 'NONE',  ( 196.0528114083369928, 24.85032509642524090, 13.83578131212104623 ) ) ;
#79670 = LINE ( 'NONE', #43666, #38230 ) ;
#79671 = CARTESIAN_POINT ( 'NONE',  ( 27.98889783105205353, -291.0600120228335754, -233.4187056126531843 ) ) ;
#79672 = CARTESIAN_POINT ( 'NONE',  ( -100.8529238652530466, -282.4692202936761873, -312.7529145065806233 ) ) ;
#79673 = CARTESIAN_POINT ( 'NONE',  ( -99.84187348620854152, -279.6150634911273301, -309.7015187993507652 ) ) ;
#79674 = CARTESIAN_POINT ( 'NONE',  ( -111.3416731436633142, -286.0086781676909595, -250.3622879153004703 ) ) ;
#79675 = CARTESIAN_POINT ( 'NONE',  ( -109.0564216407767191, -279.7607273861166277, -286.9206501410660621 ) ) ;
#79676 = CARTESIAN_POINT ( 'NONE',  ( -108.4490203671141870, -279.5816148581252492, -253.1462774101656521 ) ) ;
#79677 = CARTESIAN_POINT ( 'NONE',  ( -108.3234055418421633, -286.2390008515696422, -294.5809062667544254 ) ) ;
#79678 = EDGE_LOOP ( 'NONE', ( #66123, #33006 ) ) ;
#79679 = CARTESIAN_POINT ( 'NONE',  ( -39.10996669591111186, -294.9070896768083685, -347.3408116548110343 ) ) ;
#79680 = CARTESIAN_POINT ( 'NONE',  ( -70.68500753923009938, -291.4739437208638151, -337.1590468390009505 ) ) ;
#79681 = CARTESIAN_POINT ( 'NONE',  ( 197.1933712184921603, 24.89666632552609826, 12.64285714285713702 ) ) ;
#79682 = CARTESIAN_POINT ( 'NONE',  ( -2.602324593224680793, -285.1233781216987495, -342.4248175857292154 ) ) ;
#79683 = ORIENTED_EDGE ( 'NONE', *, *, #1655, .F. ) ;
#79684 = EDGE_CURVE ( 'NONE', #66468, #13665, #9450, .T. ) ;
#79685 = CARTESIAN_POINT ( 'NONE',  ( 37.28295724486097384, -292.1468308549264634, -285.7754272365852444 ) ) ;
#79686 = CARTESIAN_POINT ( 'NONE',  ( 30.59348526301799254, -288.6911162329827789, -241.6717684374915507 ) ) ;
#79687 = CARTESIAN_POINT ( 'NONE',  ( 36.57909759969555807, -283.3604410048124009, -274.0610740006311516 ) ) ;
#79688 = CARTESIAN_POINT ( 'NONE',  ( 26.95885546823513579, -289.5242205595983478, -311.7387908025423258 ) ) ;
#79689 = CARTESIAN_POINT ( 'NONE',  ( -20.58797924134459123, -290.1566842959712176, -345.0653617365445029 ) ) ;
#79690 = CARTESIAN_POINT ( 'NONE',  ( -110.8952605595844858, -286.7405253282360036, -255.7025232408682314 ) ) ;
#79691 = CARTESIAN_POINT ( 'NONE',  ( -104.7946081182136595, -279.1998291917834081, -233.2248121867210102 ) ) ;
#79692 = ORIENTED_EDGE ( 'NONE', *, *, #69946, .T. ) ;
#79693 = CARTESIAN_POINT ( 'NONE',  ( -3.888736827723339395, -292.6942914037786068, -338.1265609784634876 ) ) ;
#79694 = CARTESIAN_POINT ( 'NONE',  ( 33.17379529137194538, -280.9910436776739857, -239.4327344128597872 ) ) ;
#79695 = CARTESIAN_POINT ( 'NONE',  ( -34.00852999388171582, -275.9549408356749041, -196.2007818257683027 ) ) ;
#79696 = CARTESIAN_POINT ( 'NONE',  ( 199.5134772723581307, 299.2165499503948922, -6.035833136898175688 ) ) ;
#79697 = CARTESIAN_POINT ( 'NONE',  ( -114.2704648735229114, -287.0519495502703080, -270.3937649182068981 ) ) ;
#79698 = CARTESIAN_POINT ( 'NONE',  ( -78.27654851829649374, -271.7494057031277066, -206.3430564706237647 ) ) ;
#79699 = DIRECTION ( 'NONE',  ( 0.000000000000000000, 0.000000000000000000, 1.000000000000000000 ) ) ;
#79700 = CARTESIAN_POINT ( 'NONE',  ( -32.95305800079159297, -279.6165842382140454, -197.4315062872732369 ) ) ;
#79701 = CARTESIAN_POINT ( 'NONE',  ( 3.303890688361111660, -277.7242947534754194, -335.3538718953298599 ) ) ;
#79702 = CARTESIAN_POINT ( 'NONE',  ( -94.92363777879110387, -298.6193093539531560, -224.5386848785209395 ) ) ;
#79703 = CARTESIAN_POINT ( 'NONE',  ( -44.40952714796666356, -282.1981054541017215, -346.8529550229571896 ) ) ;
#79704 = CARTESIAN_POINT ( 'NONE',  ( -89.35752196413908166, -291.5571509469536977, -323.0140219024945054 ) ) ;
#79705 = CARTESIAN_POINT ( 'NONE',  ( -101.7417216877868356, -298.6136080055156299, -229.4301397984350785 ) ) ;
#79706 = CARTESIAN_POINT ( 'NONE',  ( -37.26944708758045977, -299.2581092072196043, -193.7574132542464440 ) ) ;
#79707 = CARTESIAN_POINT ( 'NONE',  ( 34.51761467832923103, -295.8223644798799796, -291.2942432471122629 ) ) ;
#79708 = CARTESIAN_POINT ( 'NONE',  ( -40.33250351514033127, -281.0896855109197077, -345.1346662736161193 ) ) ;
#79709 = CARTESIAN_POINT ( 'NONE',  ( -113.1132439323231011, -290.0480570382330825, -284.0156331628174371 ) ) ;
#79710 = CARTESIAN_POINT ( 'NONE',  ( -63.86818523615091436, -271.7246719120348644, -200.5748896092077018 ) ) ;
#79711 = CARTESIAN_POINT ( 'NONE',  ( -21.17378137699595086, -287.8563610831972710, -195.8961005807035747 ) ) ;
#79712 = CARTESIAN_POINT ( 'NONE',  ( -97.61084208874066803, -288.8932017728215556, -312.1187333311298744 ) ) ;
#79713 = CARTESIAN_POINT ( 'NONE',  ( 175.4127752309341304, 242.4573000288498577, -179.5786504745925924 ) ) ;
#79714 = VERTEX_POINT ( 'NONE', #66857 ) ;
#79715 = CARTESIAN_POINT ( 'NONE',  ( -97.87028991636330488, -289.7542429649195697, -223.7041719871709233 ) ) ;
#79716 = CARTESIAN_POINT ( 'NONE',  ( -21.12877183614458687, -288.5050673808910915, -341.5596323131114787 ) ) ;
#79717 = ORIENTED_EDGE ( 'NONE', *, *, #92592, .F. ) ;
#79718 = CARTESIAN_POINT ( 'NONE',  ( -67.08192969538106354, -286.7509719706591227, -199.6715766379703325 ) ) ;
#79719 = CARTESIAN_POINT ( 'NONE',  ( -53.95461655067646234, -277.6044974271193269, -341.5195211759166227 ) ) ;
#79720 = CARTESIAN_POINT ( 'NONE',  ( 13.08560285237687637, -291.6580343960332016, -212.5806747248830675 ) ) ;
#79721 = CARTESIAN_POINT ( 'NONE',  ( -31.63556441068186231, -283.6333430740610879, -347.0604349262638948 ) ) ;
#79722 = CARTESIAN_POINT ( 'NONE',  ( -1.938475530984976380, -284.1119793342703019, -337.9578593420944230 ) ) ;
#79723 = CARTESIAN_POINT ( 'NONE',  ( -66.56429172319867860, -283.7578368697517135, -341.5917613937901365 ) ) ;
#79724 = CARTESIAN_POINT ( 'NONE',  ( 26.47526072909369432, -281.4003472818442901, -234.8719225330882807 ) ) ;
#79725 = CARTESIAN_POINT ( 'NONE',  ( -90.05876305092316159, -230.6096148880447174, -347.9243686835410472 ) ) ;
#79726 = CARTESIAN_POINT ( 'NONE',  ( 178.7692323741149778, 254.2009183757706978, -166.1924330971562824 ) ) ;
#79727 = CARTESIAN_POINT ( 'NONE',  ( -48.59893405485766493, -154.6077932284252370, -361.6058154342690614 ) ) ;
#79728 = CARTESIAN_POINT ( 'NONE',  ( -89.34979084111495240, -272.4935364899786236, -218.9047264724705997 ) ) ;
#79729 = CARTESIAN_POINT ( 'NONE',  ( -58.84014220375144077, -294.8305230767922467, -344.2904846600839619 ) ) ;
#79730 = CARTESIAN_POINT ( 'NONE',  ( -97.18990753655256754, -247.1757387921193470, -331.6343048592842706 ) ) ;
#79731 = CARTESIAN_POINT ( 'NONE',  ( -71.16958532213601529, -272.2997657850657447, -201.7391648030283022 ) ) ;
#79732 = CARTESIAN_POINT ( 'NONE',  ( -109.9928112981043284, -298.6112232705164615, -255.0459997793538207 ) ) ;
#79733 = CARTESIAN_POINT ( 'NONE',  ( 18.20921659388077885, -289.5491151505507901, -318.5553062109909774 ) ) ;
#79734 = ORIENTED_EDGE ( 'NONE', *, *, #10105, .T. ) ;
#79735 = CARTESIAN_POINT ( 'NONE',  ( -69.41864491853944230, -296.4052712470773940, -340.1170989780540594 ) ) ;
#79736 = CARTESIAN_POINT ( 'NONE',  ( -25.13770793834681072, -286.7041848474858625, -198.2747092675330975 ) ) ;
#79737 = CARTESIAN_POINT ( 'NONE',  ( -15.85074699759223016, -273.2440056286607728, -196.6878516768029499 ) ) ;
#79738 = CARTESIAN_POINT ( 'NONE',  ( 38.44870992035536261, -294.5144949775105374, -283.0889303090206113 ) ) ;
#79739 = CARTESIAN_POINT ( 'NONE',  ( 6.456049935955877395, -293.1223099108862016, -207.1054147423439531 ) ) ;
#79740 = CARTESIAN_POINT ( 'NONE',  ( -32.15940456283966853, -292.2859856728004502, -197.5326764645921003 ) ) ;
#79741 = ORIENTED_EDGE ( 'NONE', *, *, #40562, .T. ) ;
#79742 = CARTESIAN_POINT ( 'NONE',  ( -101.5093032186467497, -275.0041785203033555, -230.4633372124957020 ) ) ;
#79743 = CARTESIAN_POINT ( 'NONE',  ( 22.45806013025439896, -273.7022788889118488, -222.4655018231010501 ) ) ;
#79744 = ORIENTED_EDGE ( 'NONE', *, *, #42294, .T. ) ;
#79745 = CARTESIAN_POINT ( 'NONE',  ( -102.0486346453794226, -277.5121535851188241, -312.0821310875710424 ) ) ;
#79746 = CARTESIAN_POINT ( 'NONE',  ( 24.47460512389315213, -273.3994820393477880, -230.0475368970224679 ) ) ;
#79747 = CARTESIAN_POINT ( 'NONE',  ( -35.39584491339906691, -275.1567852680404371, -197.0652755013672675 ) ) ;
#79748 = CARTESIAN_POINT ( 'NONE',  ( 32.74504452628131190, -276.7742972642525388, -291.6474169475393410 ) ) ;
#79749 = CARTESIAN_POINT ( 'NONE',  ( -15.12129468388211073, -299.9260740170659005, -194.1551783861579565 ) ) ;
#79750 = CARTESIAN_POINT ( 'NONE',  ( 37.97816042962453764, -273.6186377233868825, -273.9904382731602936 ) ) ;
#79751 = CARTESIAN_POINT ( 'NONE',  ( -39.68400421170134962, -295.7337232914933338, -343.4379640680119223 ) ) ;
#79752 = CARTESIAN_POINT ( 'NONE',  ( -23.42505242796522325, -293.4456092923480242, -342.6744807516273568 ) ) ;
#79753 = CARTESIAN_POINT ( 'NONE',  ( 175.2296996224750103, 276.0000000000000568, 0.000000000000000000 ) ) ;
#79754 = CARTESIAN_POINT ( 'NONE',  ( -95.16040015187419954, -278.3570321874347542, -321.1205981897799688 ) ) ;
#79755 = CARTESIAN_POINT ( 'NONE',  ( 34.62529726240596517, -275.5564234584599035, -258.0495930198588894 ) ) ;
#79756 = CARTESIAN_POINT ( 'NONE',  ( -97.18412775178586571, -283.8793110427347415, -222.6937063541520843 ) ) ;
#79757 = CARTESIAN_POINT ( 'NONE',  ( -109.8173961340521885, -298.2965337850353649, -290.2935517826441583 ) ) ;
#79758 = DIRECTION ( 'NONE',  ( 1.000000000000000000, 0.000000000000000000, 0.000000000000000000 ) ) ;
#79759 = CARTESIAN_POINT ( 'NONE',  ( -33.21935644195431081, -285.3024106417127541, -197.2659417829366362 ) ) ;
#79760 = CARTESIAN_POINT ( 'NONE',  ( -110.2885886290011115, -276.6281456993712027, -282.9551644455639803 ) ) ;
#79761 = CARTESIAN_POINT ( 'NONE',  ( -69.52536840240330207, -276.0589442887876999, -336.5535117712911415 ) ) ;
#79762 = CARTESIAN_POINT ( 'NONE',  ( 13.73331525455091295, -284.3369713028795900, -325.3524440498138119 ) ) ;
#79763 = CARTESIAN_POINT ( 'NONE',  ( 3.367019751394966676, -277.6963936503413493, -331.4342759974665569 ) ) ;
#79764 = DIRECTION ( 'NONE',  ( 0.000000000000000000, 0.000000000000000000, 1.000000000000000000 ) ) ;
#79765 = CARTESIAN_POINT ( 'NONE',  ( 9.039699025572616620, -273.0767756364499519, -209.9028164353674129 ) ) ;
#79766 = CARTESIAN_POINT ( 'NONE',  ( -58.80364107911314875, -281.7753311520498301, -198.3235339397816119 ) ) ;
#79767 = DIRECTION ( 'NONE',  ( 0.000000000000000000, 0.000000000000000000, 1.000000000000000000 ) ) ;
#79768 = CARTESIAN_POINT ( 'NONE',  ( 21.30328137218328877, -290.1238536654252016, -318.0268497199367630 ) ) ;
#79769 = CARTESIAN_POINT ( 'NONE',  ( 37.05764643777325773, -291.4252642714020567, -260.4914267720184853 ) ) ;
#79770 = DIRECTION ( 'NONE',  ( -1.000000000000000000, 0.000000000000000000, 0.000000000000000000 ) ) ;
#79771 = CARTESIAN_POINT ( 'NONE',  ( -33.77254241633748677, -296.8927315211543032, -196.9647934452050322 ) ) ;
#79772 = CARTESIAN_POINT ( 'NONE',  ( -111.0182778151683181, -288.5738149002780233, -279.4510783813382773 ) ) ;
#79773 = CARTESIAN_POINT ( 'NONE',  ( 193.6056169066500274, 279.7126221763799094, -126.0203154767880989 ) ) ;
#79774 = CARTESIAN_POINT ( 'NONE',  ( 210.1640492649794396, 37.84931640281016030, 12.09245862095555601 ) ) ;
#79775 = CARTESIAN_POINT ( 'NONE',  ( -96.76248456181804158, -288.3842634174589534, -318.2552941413810572 ) ) ;
#79776 = CARTESIAN_POINT ( 'NONE',  ( 19.98623883188853156, -283.8029021379052210, -316.8562824770722841 ) ) ;
#79777 = EDGE_CURVE ( 'NONE', #52563, #56772, #53336, .T. ) ;
#79778 = CARTESIAN_POINT ( 'NONE',  ( -101.6488117861491389, -283.3291769756244207, -229.8818714122986933 ) ) ;
#79779 = CARTESIAN_POINT ( 'NONE',  ( -51.11048966926350090, -284.6567262805410223, -342.7027715736420532 ) ) ;
#79780 = CARTESIAN_POINT ( 'NONE',  ( -107.1368458063448372, -285.0648642145199005, -292.2982865964136181 ) ) ;
#79781 = EDGE_CURVE ( 'NONE', #91332, #11243, #42808, .T. ) ;
#79782 = CARTESIAN_POINT ( 'NONE',  ( -15.40641620089360586, -290.7496314182230321, -342.5076401081882409 ) ) ;
#79783 = CARTESIAN_POINT ( 'NONE',  ( 20.01727652225171283, -275.1882505973370030, -218.9437967455579326 ) ) ;
#79784 = CARTESIAN_POINT ( 'NONE',  ( -91.75774017248153314, -289.3640858728285252, -217.8633471467662446 ) ) ;
#79785 = CARTESIAN_POINT ( 'NONE',  ( -41.38444542250103098, -277.1017034222018083, -347.2681250818313856 ) ) ;
#79786 = CARTESIAN_POINT ( 'NONE',  ( 27.22781193056925275, -296.0345058290855604, -307.8127523001895156 ) ) ;
#79787 = DIRECTION ( 'NONE',  ( 1.000000000000000000, 0.000000000000000000, 0.000000000000000000 ) ) ;
#79788 = CARTESIAN_POINT ( 'NONE',  ( -110.4683760289727132, -293.2662352645559167, -253.7030783399848985 ) ) ;
#79789 = CARTESIAN_POINT ( 'NONE',  ( -2.207541027192220007, -281.2616653458595692, -334.9265235211501590 ) ) ;
#79790 = CARTESIAN_POINT ( 'NONE',  ( -94.76549965371945916, -275.8824393019547756, -318.8839378697941243 ) ) ;
#79791 = CARTESIAN_POINT ( 'NONE',  ( -85.35681618659506853, -271.8820720181499837, -211.0546564393862639 ) ) ;
#79792 = CARTESIAN_POINT ( 'NONE',  ( 23.14132724935378249, -274.3303027134767831, -229.2814322489235792 ) ) ;
#79793 = CARTESIAN_POINT ( 'NONE',  ( -52.53140921108406047, -293.3743172515387982, -198.1978309387543788 ) ) ;
#79794 = CARTESIAN_POINT ( 'NONE',  ( 21.52271486849027227, -295.1023256204480845, -313.9316251609185429 ) ) ;
#79795 = CARTESIAN_POINT ( 'NONE',  ( 36.13254401663373727, -294.7118589412373808, -249.3339273290943936 ) ) ;
#79796 = CARTESIAN_POINT ( 'NONE',  ( 27.69559526689053897, -295.3987680965234404, -310.7527222208510125 ) ) ;
#79797 = CARTESIAN_POINT ( 'NONE',  ( -55.80535979649476275, -295.1297442824593418, -341.0399364581667214 ) ) ;
#79798 = CARTESIAN_POINT ( 'NONE',  ( -111.7712605082640067, -292.4337688317439756, -279.5937335224062394 ) ) ;
#79799 = CARTESIAN_POINT ( 'NONE',  ( -88.31994807486660193, -283.9096088846833368, -328.1403525627566182 ) ) ;
#79800 = CARTESIAN_POINT ( 'NONE',  ( -85.01238711376386448, -271.5418328090391356, -211.4729945612091058 ) ) ;
#79801 = CARTESIAN_POINT ( 'NONE',  ( -15.41142531185276354, -286.1615850034717710, -196.4947296879393548 ) ) ;
#79802 = CARTESIAN_POINT ( 'NONE',  ( -57.00981470030789211, -279.2868446704456460, -342.4218210285545183 ) ) ;
#79803 = ADVANCED_FACE ( 'NONE', ( #74903, #67794 ), #1521, .F. ) ;
#79804 = CARTESIAN_POINT ( 'NONE',  ( -93.54934186181309030, -284.0137589679008556, -223.1612078487472672 ) ) ;
#79805 = CARTESIAN_POINT ( 'NONE',  ( -97.44214906301210988, -287.9389745432378618, -315.2481274849307056 ) ) ;
#79806 = CARTESIAN_POINT ( 'NONE',  ( -33.94653134347471735, -278.2340269338157555, -194.6724245655335324 ) ) ;
#79807 = CARTESIAN_POINT ( 'NONE',  ( 188.7508426036948208, 279.9709457756753181, -124.8390596414617590 ) ) ;
#79808 = CARTESIAN_POINT ( 'NONE',  ( -79.33953777290703613, -284.9759729142399465, -210.5146487365948644 ) ) ;
#79809 = CARTESIAN_POINT ( 'NONE',  ( 37.28715798272640569, -282.5393574549117375, -253.0251618483688105 ) ) ;
#79810 = CARTESIAN_POINT ( 'NONE',  ( -43.17640360332320881, -288.1828827333312120, -346.9037626215624641 ) ) ;
#79811 = CARTESIAN_POINT ( 'NONE',  ( -92.73824779070713475, -279.4296111807388456, -322.7594912745115039 ) ) ;
#79812 = CARTESIAN_POINT ( 'NONE',  ( -77.54143906954840304, -278.8944476439708637, -335.5170619407300592 ) ) ;
#79813 = CARTESIAN_POINT ( 'NONE',  ( -108.6062910400219010, -278.5948870703792863, -254.4811943813358823 ) ) ;
#79814 = CARTESIAN_POINT ( 'NONE',  ( -16.19838241306328541, -276.3066017305691844, -198.7194715564970693 ) ) ;
#79815 = CARTESIAN_POINT ( 'NONE',  ( 23.10807104604907991, -292.9140081826763549, -222.6449212539245650 ) ) ;
#79816 = CARTESIAN_POINT ( 'NONE',  ( -67.00535508885486990, -287.4628433758500137, -338.9139115621897531 ) ) ;
#79817 = CARTESIAN_POINT ( 'NONE',  ( -76.77291679176552464, -293.1340749037259457, -205.0958116347061093 ) ) ;
#79818 = CARTESIAN_POINT ( 'NONE',  ( -92.97002897682892808, -296.1495177474625962, -222.5954517256548684 ) ) ;
#79819 = CARTESIAN_POINT ( 'NONE',  ( 35.55607470134342663, -293.1523756714088336, -265.3191091150566194 ) ) ;
#79820 = CARTESIAN_POINT ( 'NONE',  ( -114.0599762162293587, -291.6567426951565949, -268.3764867220202746 ) ) ;
#79821 = CARTESIAN_POINT ( 'NONE',  ( 35.24202269008107891, -282.3234664588486567, -279.4627077061001046 ) ) ;
#79822 = CARTESIAN_POINT ( 'NONE',  ( -101.0066746986631756, -272.1787837492568656, -227.3760495772780246 ) ) ;
#79823 = CARTESIAN_POINT ( 'NONE',  ( -57.25649096048846332, -289.9538607843977616, -344.6907327782436710 ) ) ;
#79824 = CARTESIAN_POINT ( 'NONE',  ( -60.87094439978719862, -281.4937416184585004, -342.4345254973252395 ) ) ;
#79825 = CARTESIAN_POINT ( 'NONE',  ( -73.16026383770426378, -289.8470415543192757, -338.5137800806448922 ) ) ;
#79827 = CARTESIAN_POINT ( 'NONE',  ( -62.57416165117810181, -286.0479747758561757, -201.7841284922041609 ) ) ;
#79826 = CIRCLE ( 'NONE', #16356, 2.999999999999997335 ) ;
#79828 = CARTESIAN_POINT ( 'NONE',  ( 138.5464852711123740, 180.7133914995600605, -241.3450704663493980 ) ) ;
#79829 = CARTESIAN_POINT ( 'NONE',  ( 201.2091094121765309, 294.9047486845406070, -68.44675130712812461 ) ) ;
#79830 = CARTESIAN_POINT ( 'NONE',  ( -70.05943696497188000, -195.9697670439899468, -356.6292458268069367 ) ) ;
#79831 = CARTESIAN_POINT ( 'NONE',  ( -69.80275346352172505, -278.8105541970789432, -204.7813850437195242 ) ) ;
#79832 = CARTESIAN_POINT ( 'NONE',  ( 5.113308282586055853, -279.5618692936172920, -210.5965939430733158 ) ) ;
#79833 = CARTESIAN_POINT ( 'NONE',  ( -7.694797567457321463, -274.0968230335276985, -199.2636629006667306 ) ) ;
#79834 = CARTESIAN_POINT ( 'NONE',  ( -68.71647568833768105, -197.0276430710098055, -358.0455354867054325 ) ) ;
#79835 = CARTESIAN_POINT ( 'NONE',  ( -92.63473493410921833, -277.8542020889144624, -217.5476352127069788 ) ) ;
#79836 = CARTESIAN_POINT ( 'NONE',  ( -10.40523634634057970, -280.7191817187670040, -340.0310800157167819 ) ) ;
#79837 = CARTESIAN_POINT ( 'NONE',  ( 1.274034075506777386, -296.3039225032662216, -335.8042160562505387 ) ) ;
#79838 = CARTESIAN_POINT ( 'NONE',  ( -67.83258378651797216, -292.1331780359816435, -203.9523832654658690 ) ) ;
#79839 = CARTESIAN_POINT ( 'NONE',  ( -95.35008102488841075, -288.6052747018987361, -315.5065186471342145 ) ) ;
#79840 = CARTESIAN_POINT ( 'NONE',  ( 7.169222101908442113, -275.2921030056748464, -207.5893910037138426 ) ) ;
#79841 = CARTESIAN_POINT ( 'NONE',  ( -96.40716397846081520, -296.1182186694284155, -313.2808328441833510 ) ) ;
#79842 = ORIENTED_EDGE ( 'NONE', *, *, #89540, .T. ) ;
#79843 = FACE_OUTER_BOUND ( 'NONE', #84614, .T. ) ;
#79844 = CARTESIAN_POINT ( 'NONE',  ( 196.8803347170859865, 24.42324672360810212, 12.49999999999998757 ) ) ;
#79845 = CARTESIAN_POINT ( 'NONE',  ( -83.70304457559441857, -281.3421346610602427, -210.6296572334624102 ) ) ;
#79846 = CARTESIAN_POINT ( 'NONE',  ( -51.90214896488578233, -280.9412415782480252, -198.4605801171763915 ) ) ;
#79847 = CARTESIAN_POINT ( 'NONE',  ( -76.98325603881406209, -281.2893712374980737, -205.4733405268882223 ) ) ;
#79849 = CIRCLE ( 'NONE', #35991, 2.395975569037533948 ) ;
#79848 = CARTESIAN_POINT ( 'NONE',  ( -3.523351928541757605, -281.6530512183750261, -335.3345990390674842 ) ) ;
#79850 = CARTESIAN_POINT ( 'NONE',  ( -13.82604475682353673, -272.8428140176880561, -200.5204299557864545 ) ) ;
#79851 = CARTESIAN_POINT ( 'NONE',  ( 113.5000000000000568, -298.0521521680024080, -540.3336712212508246 ) ) ;
#79852 = CARTESIAN_POINT ( 'NONE',  ( 152.4536156746142410, 250.0000000000000568, 12.00000000000000000 ) ) ;
#79853 = CARTESIAN_POINT ( 'NONE',  ( 26.79014666220401963, -275.7972460815495310, -228.0377787043189244 ) ) ;
#79854 = CARTESIAN_POINT ( 'NONE',  ( 165.2424497756046549, 214.5000000000000568, 22.91843887563435800 ) ) ;
#79855 = CARTESIAN_POINT ( 'NONE',  ( 11.42402705322856704, -278.3760872167123921, -327.3427334237465516 ) ) ;
#79856 = CARTESIAN_POINT ( 'NONE',  ( -112.4894782852300352, -276.9516129134252083, -284.2684767926167524 ) ) ;
#79857 = ORIENTED_EDGE ( 'NONE', *, *, #70067, .T. ) ;
#79858 = CARTESIAN_POINT ( 'NONE',  ( 201.2104617360081704, 41.21457449016152452, 9.000000000000000000 ) ) ;
#79859 = CARTESIAN_POINT ( 'NONE',  ( -69.73960393270914437, -285.4563899947398227, -338.4104262511389720 ) ) ;
#79860 = ADVANCED_FACE ( 'NONE', ( #60697 ), #37949, .T. ) ;
#79861 = CARTESIAN_POINT ( 'NONE',  ( -44.30541898871909012, -291.1591296860802345, -197.4808783274968391 ) ) ;
#79862 = CARTESIAN_POINT ( 'NONE',  ( -29.46512029369100816, -285.4980330182161765, -193.8675085985707653 ) ) ;
#79863 = CARTESIAN_POINT ( 'NONE',  ( -76.68450266871816723, -281.8260202464169311, -333.1123927796631961 ) ) ;
#79864 = CARTESIAN_POINT ( 'NONE',  ( -4.581021098104332445, -281.1864790698703018, -336.2558281527755071 ) ) ;
#79865 = CARTESIAN_POINT ( 'NONE',  ( 21.33654561775109570, -283.3732071112323752, -314.4726392767776133 ) ) ;
#79866 = CARTESIAN_POINT ( 'NONE',  ( -68.00251869574032071, -271.6494982643052936, -201.9006614263446977 ) ) ;
#79867 = CARTESIAN_POINT ( 'NONE',  ( -87.21083404300115660, -283.7709606333540933, -212.6760917204390182 ) ) ;
#79868 = CARTESIAN_POINT ( 'NONE',  ( -108.8841400751690855, -298.2614116142880221, -292.9136088955336845 ) ) ;
#79869 = CARTESIAN_POINT ( 'NONE',  ( -94.13055417397667668, -280.1458524817245461, -224.1179076155090968 ) ) ;
#79870 = CARTESIAN_POINT ( 'NONE',  ( -36.60950086985666729, -288.0614788464633875, -195.1852852343108964 ) ) ;
#79871 = CARTESIAN_POINT ( 'NONE',  ( 41.08708295871279859, -293.9068999365417199, -472.6442049081569508 ) ) ;
#79872 = DIRECTION ( 'NONE',  ( -1.000000000000000000, 0.000000000000000000, 0.000000000000000000 ) ) ;
#79873 = CARTESIAN_POINT ( 'NONE',  ( 31.99315808284682561, -295.0822804223934668, -240.3279424557018160 ) ) ;
#79874 = CARTESIAN_POINT ( 'NONE',  ( -73.83689859351970597, -275.5365553437517860, -335.8976569923572129 ) ) ;
#79875 = CARTESIAN_POINT ( 'NONE',  ( -54.47557780599484545, -288.4639132481751176, -345.3195820339592501 ) ) ;
#79876 = CARTESIAN_POINT ( 'NONE',  ( 26.94130282669514287, -291.4599797080752523, -234.0057103104477392 ) ) ;
#79877 = CARTESIAN_POINT ( 'NONE',  ( -39.18681828117371424, -275.7606134426038125, -343.8311051767138338 ) ) ;
#79878 = CARTESIAN_POINT ( 'NONE',  ( -89.38440831716744128, -293.9336602493576152, -323.3712896321620178 ) ) ;
#79879 = CARTESIAN_POINT ( 'NONE',  ( -108.2319702859349917, -292.1217337316521139, -250.9752190893022146 ) ) ;
#79880 = CARTESIAN_POINT ( 'NONE',  ( 21.31550574532285580, -284.6948066931273615, -317.0979686699210447 ) ) ;
#79881 = CARTESIAN_POINT ( 'NONE',  ( -32.07982067835222040, -293.4668207671824689, -346.4992843907436963 ) ) ;
#79882 = CARTESIAN_POINT ( 'NONE',  ( -7.880600594848340634, -290.2598379940407085, -338.0802540273634236 ) ) ;
#79883 = CARTESIAN_POINT ( 'NONE',  ( -111.8784507633417320, -288.6039563654632047, -285.2003459329209250 ) ) ;
#79884 = CARTESIAN_POINT ( 'NONE',  ( -7.966734408126454170, -290.0850101629147275, -337.8877160459251741 ) ) ;
#79885 = CARTESIAN_POINT ( 'NONE',  ( 140.6539576904058606, 250.5000000000000568, 10.50000000000000000 ) ) ;
#79886 = CARTESIAN_POINT ( 'NONE',  ( -66.38374255004870861, -290.2451184653572227, -337.5655399012031808 ) ) ;
#79887 = ADVANCED_FACE ( 'NONE', ( #73955 ), #53584, .F. ) ;
#79888 = DIRECTION ( 'NONE',  ( 0.000000000000000000, 0.000000000000000000, -1.000000000000000000 ) ) ;
#79889 = CIRCLE ( 'NONE', #58747, 1.895975569037589015 ) ;
#79890 = CARTESIAN_POINT ( 'NONE',  ( -12.33875515447740057, -289.9392085087940814, -342.8243124132956723 ) ) ;
#79891 = CARTESIAN_POINT ( 'NONE',  ( -98.89066618633617622, -277.1601291171922981, -226.8854744426099046 ) ) ;
#79892 = CARTESIAN_POINT ( 'NONE',  ( -111.7117015696642284, -279.1348734310820419, -250.4394553235269711 ) ) ;
#79893 = CARTESIAN_POINT ( 'NONE',  ( -18.92756791313701470, -282.4882215368415928, -345.1600497893560942 ) ) ;
#79894 = CARTESIAN_POINT ( 'NONE',  ( 23.57156966168662748, -286.1473971553756428, -314.1169657524922627 ) ) ;
#79895 = CARTESIAN_POINT ( 'NONE',  ( 207.6243754364163294, 29.64962331212859681, 14.86901082953205666 ) ) ;
#79896 = CARTESIAN_POINT ( 'NONE',  ( 35.78791346908104032, -279.5261541726940777, -257.5969064170384968 ) ) ;
#79897 = CARTESIAN_POINT ( 'NONE',  ( -112.3259607959232369, -282.5929181911311616, -267.1733319830004234 ) ) ;
#79898 = CYLINDRICAL_SURFACE ( 'NONE', #9433, 1.000000000000000888 ) ;
#79899 = CARTESIAN_POINT ( 'NONE',  ( -110.6656060873578866, -277.2993212123437274, -249.2350069280225284 ) ) ;
#79900 = CARTESIAN_POINT ( 'NONE',  ( -107.9479561542274269, -283.0883590823062832, -300.4344498108670791 ) ) ;
#79901 = CARTESIAN_POINT ( 'NONE',  ( -63.37371358197463422, -274.5069477677270129, -201.9740901222407672 ) ) ;
#79902 = CARTESIAN_POINT ( 'NONE',  ( -36.21412570704001155, -293.6666153956381891, -196.5571161702578422 ) ) ;
#79903 = CARTESIAN_POINT ( 'NONE',  ( -20.66061182921227868, -299.5720516418535908, -193.8506246229822807 ) ) ;
#79904 = CARTESIAN_POINT ( 'NONE',  ( 34.72732613703151827, -275.3778995498079780, -282.4199555964726756 ) ) ;
#79905 = CARTESIAN_POINT ( 'NONE',  ( -85.75008630428908418, -297.7219809968311210, -327.7147881947425390 ) ) ;
#79906 = CARTESIAN_POINT ( 'NONE',  ( -4.331139422035541031, -288.7956889184557667, -339.9406958813351594 ) ) ;
#79907 = CARTESIAN_POINT ( 'NONE',  ( 36.28009133020469079, -279.4146336464697811, -253.2998946405561469 ) ) ;
#79908 = CARTESIAN_POINT ( 'NONE',  ( -22.19171153026570309, -292.0742309712779274, -194.8119053491355146 ) ) ;
#79909 = EDGE_CURVE ( 'NONE', #93327, #51424, #90011, .T. ) ;
#79910 = CARTESIAN_POINT ( 'NONE',  ( -25.35882353113471765, -291.2672470410496430, -198.0611564523699144 ) ) ;
#79911 = CARTESIAN_POINT ( 'NONE',  ( -82.98867488528608760, -293.6761491365228949, -329.9358940420221984 ) ) ;
#79912 = ORIENTED_EDGE ( 'NONE', *, *, #86325, .F. ) ;
#79913 = CARTESIAN_POINT ( 'NONE',  ( 196.8803347170859865, 73.40565171261609123, 12.49999999999999289 ) ) ;
#79914 = CARTESIAN_POINT ( 'NONE',  ( -109.6847675829058062, -289.9239003186769423, -280.6719363891194234 ) ) ;
#79915 = DIRECTION ( 'NONE',  ( -0.000000000000000000, 1.000000000000000000, -0.000000000000000000 ) ) ;
#79916 = CARTESIAN_POINT ( 'NONE',  ( -21.04563713393467239, -287.1975907259961218, -195.3460625391977885 ) ) ;
#79917 = CARTESIAN_POINT ( 'NONE',  ( -37.30987171927208124, -285.5519495502701375, -340.3611179825599606 ) ) ;
#79918 = CARTESIAN_POINT ( 'NONE',  ( -41.94347497937574332, -294.1674237464262660, -347.0400035895781343 ) ) ;
#79919 = CARTESIAN_POINT ( 'NONE',  ( 29.34035161715986817, -283.3583025725668563, -307.9764932696696746 ) ) ;
#79920 = CARTESIAN_POINT ( 'NONE',  ( -108.9285500315818211, -284.5740352333848477, -256.0669609447368202 ) ) ;
#79921 = CARTESIAN_POINT ( 'NONE',  ( 36.07867515015146864, -276.8114173546283041, -266.0937540317375465 ) ) ;
#79922 = CARTESIAN_POINT ( 'NONE',  ( -23.23209896148750175, -292.8910786604667464, -343.7130360337502566 ) ) ;
#79923 = CARTESIAN_POINT ( 'NONE',  ( -8.597239220105997504, -275.4623156698458502, -337.9090681178068962 ) ) ;
#79924 = VERTEX_POINT ( 'NONE', #77707 ) ;
#79925 = LINE ( 'NONE', #22170, #65251 ) ;
#79926 = CARTESIAN_POINT ( 'NONE',  ( -58.84948391120601485, -294.9895634868346406, -344.3298648438227474 ) ) ;
#79927 = CARTESIAN_POINT ( 'NONE',  ( 11.06995656023202379, -290.2964621124732503, -326.9768459337045670 ) ) ;
#79928 = CARTESIAN_POINT ( 'NONE',  ( -99.67834943728260555, -298.2261617960509170, -225.6885910435495646 ) ) ;
#79929 = EDGE_CURVE ( 'NONE', #40890, #60407, #6525, .T. ) ;
#79930 = CARTESIAN_POINT ( 'NONE',  ( 11.19555105210906554, -287.3967987892851284, -215.6302564566073556 ) ) ;
#79931 = CARTESIAN_POINT ( 'NONE',  ( -77.70142338315010022, -276.6383853776532646, -335.7215389375089671 ) ) ;
#79932 = CARTESIAN_POINT ( 'NONE',  ( 1.724805285077424921, -295.1953733679792435, -336.5964630889572504 ) ) ;
#79933 = CARTESIAN_POINT ( 'NONE',  ( -2.391919785929478515, -286.7342947079240503, -337.5832745760851594 ) ) ;
#79934 = CARTESIAN_POINT ( 'NONE',  ( -113.3693350731649048, -297.0373969254639519, -258.2134636440722488 ) ) ;
#79935 = CARTESIAN_POINT ( 'NONE',  ( -106.5926890010002097, -291.1929369843527411, -247.2010655887430346 ) ) ;
#79936 = CARTESIAN_POINT ( 'NONE',  ( 139.6925840978351516, 0.000000000000000000, 21.50000000000000000 ) ) ;
#79937 = DIRECTION ( 'NONE',  ( 0.000000000000000000, 0.000000000000000000, 1.000000000000000000 ) ) ;
#79938 = CARTESIAN_POINT ( 'NONE',  ( -104.9195836729417977, -260.6502345264940459, -315.6181490027205427 ) ) ;
#79939 = CARTESIAN_POINT ( 'NONE',  ( 38.40479664784151481, -289.1941171461741646, -280.0160790089450984 ) ) ;
#79940 = CARTESIAN_POINT ( 'NONE',  ( -88.47809603358389552, -282.9094976428776249, -206.1857440867352693 ) ) ;
#79941 = ORIENTED_EDGE ( 'NONE', *, *, #73162, .T. ) ;
#79942 = CARTESIAN_POINT ( 'NONE',  ( -109.5076500699411071, -278.2385931900018932, -243.6482815798421484 ) ) ;
#79943 = CARTESIAN_POINT ( 'NONE',  ( -45.82256336789456697, -285.1599463812947306, -344.7646078431207002 ) ) ;
#79944 = CARTESIAN_POINT ( 'NONE',  ( -107.6918058678267585, -282.7428138117067533, -300.3205173699818147 ) ) ;
#79945 = CARTESIAN_POINT ( 'NONE',  ( -23.54174446356137906, -286.9543820970414458, -343.5635115681350271 ) ) ;
#79946 = CARTESIAN_POINT ( 'NONE',  ( 8.740004514686489756, -276.5367630015933855, -210.2214307949028580 ) ) ;
#79947 = CARTESIAN_POINT ( 'NONE',  ( -69.29010129422182729, -298.1123846191018743, -204.6550444062928875 ) ) ;
#79948 = CARTESIAN_POINT ( 'NONE',  ( -20.75303642919150704, -293.5196797168992475, -342.0100779569017391 ) ) ;
#79949 = CARTESIAN_POINT ( 'NONE',  ( -94.89102175147579032, -279.8954836203067202, -219.3573106007924309 ) ) ;
#79951 = CARTESIAN_POINT ( 'NONE',  ( -109.2308386884985225, -278.0754224500493592, -257.1004835535222810 ) ) ;
#79950 = CARTESIAN_POINT ( 'NONE',  ( 18.30841142094000062, -276.2239205521714211, -317.6058540341190337 ) ) ;
#79952 = CARTESIAN_POINT ( 'NONE',  ( 36.28519919539937888, -276.3594897275684161, -248.7147107484173603 ) ) ;
#79953 = CARTESIAN_POINT ( 'NONE',  ( -8.015609246350436479, -275.5972297308974817, -341.2376958474231401 ) ) ;
#79954 = CARTESIAN_POINT ( 'NONE',  ( 175.2296996224750103, 160.0000000000000568, 0.000000000000000000 ) ) ;
#79955 = CARTESIAN_POINT ( 'NONE',  ( -6.903917639956217656, -274.6525737147940731, -338.9208695825799964 ) ) ;
#79956 = CARTESIAN_POINT ( 'NONE',  ( -107.2414162518167444, -298.3757202813615663, -239.3654275940185698 ) ) ;
#79957 = CARTESIAN_POINT ( 'NONE',  ( 201.2104617360081704, 15.00000000000000000, -9.000000000000001776 ) ) ;
#79958 = CIRCLE ( 'NONE', #67929, 0.5000000000000004441 ) ;
#79959 = B_SPLINE_CURVE_WITH_KNOTS ( 'NONE', 3,
 ( #89405, #24559, #53444, #39211, #82327, #17477, #68126, #89882 ),
 .UNSPECIFIED., .F., .F.,
 ( 4, 2, 2, 4 ),
 ( 0.000000000000000000, 0.001862880473700167768, 0.002794320710550249158, 0.003725760947400331199 ),
 .UNSPECIFIED. ) ;
#79960 = CARTESIAN_POINT ( 'NONE',  ( -43.18343439339132317, -296.0521521680024080, -430.6442049081568939 ) ) ;
#79961 = CARTESIAN_POINT ( 'NONE',  ( -52.16481256535811895, -286.9375687067379204, -198.5662615489234497 ) ) ;
#79962 = CARTESIAN_POINT ( 'NONE',  ( -21.22108779242348220, -288.0163481712660882, -196.1041326598771377 ) ) ;
#79963 = CARTESIAN_POINT ( 'NONE',  ( 23.62365487127207331, -286.3407795619510239, -229.9319036039915432 ) ) ;
#79964 = CARTESIAN_POINT ( 'NONE',  ( -92.79625131606731259, -277.6397508784987735, -221.6465908577899881 ) ) ;
#79965 = CARTESIAN_POINT ( 'NONE',  ( -95.09774491985504596, -287.0613183289924564, -223.7029439125718113 ) ) ;
#79966 = CARTESIAN_POINT ( 'NONE',  ( -81.68983269541402592, -277.9161220652369479, -211.4417152010780967 ) ) ;
#79967 = CARTESIAN_POINT ( 'NONE',  ( 5.699065214431824344, -277.7707387009219815, -329.9952397558817552 ) ) ;
#79968 = CARTESIAN_POINT ( 'NONE',  ( 35.08068306358324406, -275.9174022139249587, -260.7181488081261023 ) ) ;
#79969 = CARTESIAN_POINT ( 'NONE',  ( 37.43397358022727417, -286.5569129268970414, -287.0524653630985199 ) ) ;
#79970 = CARTESIAN_POINT ( 'NONE',  ( 37.03807558136119837, -282.5968231149676058, -289.6434359555658489 ) ) ;
#79971 = CARTESIAN_POINT ( 'NONE',  ( 38.08645936024664991, -282.2343665800169106, -285.5308134196599212 ) ) ;
#79972 = ORIENTED_EDGE ( 'NONE', *, *, #43878, .T. ) ;
#79973 = ORIENTED_EDGE ( 'NONE', *, *, #16723, .F. ) ;
#79974 = CARTESIAN_POINT ( 'NONE',  ( 123.4306832106270946, -134.2641364535880939, -4.999999999999990230 ) ) ;
#79975 = CARTESIAN_POINT ( 'NONE',  ( 22.32953270403515234, -290.0469348575391564, -317.0687316798927782 ) ) ;
#79976 = CARTESIAN_POINT ( 'NONE',  ( -72.95923524778829972, -288.1988528254501034, -338.0861162919775325 ) ) ;
#79977 = CARTESIAN_POINT ( 'NONE',  ( -3.564872984653602916, -296.2140040951331343, -338.6805230108923865 ) ) ;
#79978 = EDGE_CURVE ( 'NONE', #90108, #51697, #3465, .T. ) ;
#79979 = CARTESIAN_POINT ( 'NONE',  ( -63.37920834285855420, -272.7631445555286405, -201.8971866738182825 ) ) ;
#79980 = CARTESIAN_POINT ( 'NONE',  ( -37.78610623516770062, -291.3953133248352287, -193.4643346273714428 ) ) ;
#79981 = CARTESIAN_POINT ( 'NONE',  ( 26.98192819670782328, -285.5435407426504639, -234.2958712719755283 ) ) ;
#79982 = CARTESIAN_POINT ( 'NONE',  ( 34.91528106421958455, -288.9263050095711947, -283.2475129211538842 ) ) ;
#79983 = CARTESIAN_POINT ( 'NONE',  ( -95.95921662488163406, -298.4090924074130271, -317.1477375740089997 ) ) ;
#79984 = CARTESIAN_POINT ( 'NONE',  ( 21.72843739972778820, -290.1866567700773771, -316.5956507077469269 ) ) ;
#79985 = CARTESIAN_POINT ( 'NONE',  ( -48.61969054578635507, -287.1951287119247809, -344.7295616695670901 ) ) ;
#79986 = CARTESIAN_POINT ( 'NONE',  ( -65.06310639938220675, -291.4143486903820417, -340.1041648955310848 ) ) ;
#79987 = CARTESIAN_POINT ( 'NONE',  ( -109.4267519983705625, -285.6643402697250735, -257.3617106583516261 ) ) ;
#79988 = CARTESIAN_POINT ( 'NONE',  ( -50.27652232133611676, -293.8875607083857062, -196.3157346106499972 ) ) ;
#79989 = DIRECTION ( 'NONE',  ( 0.000000000000000000, 0.000000000000000000, 1.000000000000000000 ) ) ;
#79990 = CARTESIAN_POINT ( 'NONE',  ( 152.4536156746142410, 250.0000000000000568, 12.50000000000000000 ) ) ;
#79991 = CARTESIAN_POINT ( 'NONE',  ( -23.70910264812068391, -300.1416918350858509, -194.7966907522588258 ) ) ;
#79992 = CARTESIAN_POINT ( 'NONE',  ( 34.38697248441357601, -280.9397964164568293, -284.8324262705728529 ) ) ;
#79993 = CARTESIAN_POINT ( 'NONE',  ( -72.36480030478240622, -281.5155043536400399, -336.6814248679848447 ) ) ;
#79994 = CARTESIAN_POINT ( 'NONE',  ( -108.2300332706132053, -295.3698936014358196, -300.1468560865658901 ) ) ;
#79995 = CARTESIAN_POINT ( 'NONE',  ( 35.11795074634553515, -273.5949247230411743, -255.2136346269770399 ) ) ;
#79996 = CARTESIAN_POINT ( 'NONE',  ( -110.5438000832981800, -276.8068866377743689, -256.8419921949972604 ) ) ;
#79997 = CARTESIAN_POINT ( 'NONE',  ( -58.05973178621965047, -299.0939771850914894, -199.8486606356547952 ) ) ;
#79998 = DIRECTION ( 'NONE',  ( 0.000000000000000000, 1.000000000000000000, 0.000000000000000000 ) ) ;
#79999 = CARTESIAN_POINT ( 'NONE',  ( -93.91235873392774636, -294.0943731290846586, -321.1124987588493127 ) ) ;
#80000 = CARTESIAN_POINT ( 'NONE',  ( 18.43077764739624058, -295.6558161930612414, -318.3887286531371501 ) ) ;
#80001 = LINE ( 'NONE', #15139, #49003 ) ;
#80002 = CARTESIAN_POINT ( 'NONE',  ( -12.94477971193989063, -295.5298057413509696, -339.3883471459948282 ) ) ;
#80003 = CARTESIAN_POINT ( 'NONE',  ( 175.2296996224750103, 20.00000000000000000, 0.000000000000000000 ) ) ;
#80005 = CARTESIAN_POINT ( 'NONE',  ( -101.2145643573273333, -297.0352209466540216, -235.0162850482779220 ) ) ;
#80004 = CARTESIAN_POINT ( 'NONE',  ( -79.98617567928744165, -283.4988497948511394, -208.1704121334990418 ) ) ;
#80006 = CARTESIAN_POINT ( 'NONE',  ( -102.5184744938278811, -285.0890344761562005, -229.3612633087130348 ) ) ;
#80007 = CARTESIAN_POINT ( 'NONE',  ( 6.117149482042417041, -284.3880909399846360, -332.2364601830437891 ) ) ;
#80008 = CARTESIAN_POINT ( 'NONE',  ( 25.83192350677454741, -287.8013541471643748, -314.4394225964033467 ) ) ;
#80009 = CARTESIAN_POINT ( 'NONE',  ( -5.232458347296809364, -290.4755195702724109, -202.7524236615331006 ) ) ;
#80010 = CARTESIAN_POINT ( 'NONE',  ( -90.93819492506491997, -278.5121184660077915, -215.2272153831272874 ) ) ;
#80011 = CARTESIAN_POINT ( 'NONE',  ( 10.64812456238590599, -272.1952119285918457, -210.2361428286349394 ) ) ;
#80012 = CARTESIAN_POINT ( 'NONE',  ( -43.49048823363975202, -253.6564221937692594, -491.6618016576409218 ) ) ;
#80013 = CARTESIAN_POINT ( 'NONE',  ( 36.05209293348595878, -286.3561750816983817, -271.0551234927905284 ) ) ;
#80015 = CARTESIAN_POINT ( 'NONE',  ( 199.7104933562245321, 66.88149622424963070, -10.01660547250589950 ) ) ;
#80014 = CARTESIAN_POINT ( 'NONE',  ( -91.39047781611820653, -288.7194067818076064, -324.8437593957765444 ) ) ;
#80016 = DIRECTION ( 'NONE',  ( 0.000000000000000000, -1.000000000000000000, -0.000000000000000000 ) ) ;
#80017 = CARTESIAN_POINT ( 'NONE',  ( -106.7325017251612849, -297.8194117279311968, -295.6380863095468499 ) ) ;
#80018 = CARTESIAN_POINT ( 'NONE',  ( -113.7886835724599877, -279.9975413868086775, -268.7648085828665216 ) ) ;
#80020 = CARTESIAN_POINT ( 'NONE',  ( -3.135430944350504401, -280.1838368289979826, -205.8332268616105978 ) ) ;
#80019 = CARTESIAN_POINT ( 'NONE',  ( -91.53207783417578014, -293.8393373403799842, -322.7234113468590522 ) ) ;
#80021 = CARTESIAN_POINT ( 'NONE',  ( -3.226874230951582323, -294.7807877499909068, -339.4059955904979802 ) ) ;
#80022 = CARTESIAN_POINT ( 'NONE',  ( 36.32137750142408805, -285.4169195126616501, -253.4790698470454799 ) ) ;
#80023 = CARTESIAN_POINT ( 'NONE',  ( -42.32332224370642138, -281.9894799687002660, -195.5267402488123878 ) ) ;
#80025 = CARTESIAN_POINT ( 'NONE',  ( -108.0597480763344578, -295.8620961743175712, -251.2769069749305402 ) ) ;
#80024 = CIRCLE ( 'NONE', #81485, 2.888540232138026020 ) ;
#80026 = ORIENTED_EDGE ( 'NONE', *, *, #58451, .T. ) ;
#80027 = CARTESIAN_POINT ( 'NONE',  ( 19.76871431689382419, -284.1999257070568774, -318.4460008600389074 ) ) ;
#80028 = CYLINDRICAL_SURFACE ( 'NONE', #8060, 7.500000000000007105 ) ;
#80029 = CARTESIAN_POINT ( 'NONE',  ( 21.31550574532286291, -284.4094976428775681, -223.6242672951989618 ) ) ;
#80030 = CARTESIAN_POINT ( 'NONE',  ( -66.15715898127736239, -272.8816433292671491, -199.1161694326408451 ) ) ;
#80031 = CARTESIAN_POINT ( 'NONE',  ( -87.92906026335599279, -291.1543227752288203, -217.6612417906548558 ) ) ;
#80032 = CARTESIAN_POINT ( 'NONE',  ( 11.75345746763725430, -282.2689564493453531, -215.4031954281252297 ) ) ;
#80033 = CARTESIAN_POINT ( 'NONE',  ( -54.41618812260297489, -275.4292610621345148, -198.5634698823040480 ) ) ;
#80034 = CARTESIAN_POINT ( 'NONE',  ( 36.77505886944704372, -283.3765655310703551, -288.1127834550392777 ) ) ;
#80035 = CARTESIAN_POINT ( 'NONE',  ( 17.36898165654053727, -279.6509012852746991, -221.4339087422084731 ) ) ;
#80036 = CARTESIAN_POINT ( 'NONE',  ( -102.3027338737512508, -280.0508082347383265, -307.9495553102573240 ) ) ;
#80037 = CARTESIAN_POINT ( 'NONE',  ( -106.8441332339289715, -273.1437039252710406, -237.2188217909673256 ) ) ;
#80038 = ORIENTED_EDGE ( 'NONE', *, *, #1524, .T. ) ;
#80039 = CARTESIAN_POINT ( 'NONE',  ( -49.71714681559193139, -273.7319449527918778, -194.3083106230838553 ) ) ;
#80040 = CARTESIAN_POINT ( 'NONE',  ( 13.35309030582427248, -296.2569560945738090, -324.9419021120316415 ) ) ;
#80041 = DIRECTION ( 'NONE',  ( 0.000000000000000000, 1.000000000000000000, 0.000000000000000000 ) ) ;
#80042 = ADVANCED_FACE ( 'NONE', ( #63524 ), #1974, .T. ) ;
#80043 = FACE_OUTER_BOUND ( 'NONE', #65531, .T. ) ;
#80044 = CARTESIAN_POINT ( 'NONE',  ( 34.31040194425124668, -292.0089716057115083, -295.1445308390067908 ) ) ;
#80045 = CARTESIAN_POINT ( 'NONE',  ( -91.16362954964095877, -272.7684995182736998, -220.9342165796247741 ) ) ;
#80046 = CARTESIAN_POINT ( 'NONE',  ( 18.89151087673606710, -294.3641074791419214, -218.7807560890122431 ) ) ;
#80048 = CARTESIAN_POINT ( 'NONE',  ( -68.18305035320545926, -292.8611357790121019, -200.2267849081509894 ) ) ;
#80047 = CARTESIAN_POINT ( 'NONE',  ( -4.771743288812468897, -285.1233781216987495, -337.9199732462171255 ) ) ;
#80049 = CARTESIAN_POINT ( 'NONE',  ( -67.03358679442662549, -291.4422528928395764, -339.1072389326330949 ) ) ;
#80050 = CARTESIAN_POINT ( 'NONE',  ( 22.28260205754713397, -274.1719576849306463, -315.5824737641199818 ) ) ;
#80051 = CARTESIAN_POINT ( 'NONE',  ( -13.29759323602683985, -278.6577339457459743, -340.8652588854280339 ) ) ;
#80052 = CARTESIAN_POINT ( 'NONE',  ( 34.83643286206906708, -291.8676917096804004, -288.5718653311324715 ) ) ;
#80053 = CARTESIAN_POINT ( 'NONE',  ( 37.65207086886465504, -283.5496012573414077, -281.1425739204342449 ) ) ;
#80054 = EDGE_LOOP ( 'NONE', ( #91700, #39410, #30471, #12475, #53491 ) ) ;
#80055 = CARTESIAN_POINT ( 'NONE',  ( -56.32848531964684469, -282.9703562229142904, -340.8706171637004445 ) ) ;
#80056 = CARTESIAN_POINT ( 'NONE',  ( -25.45710659807634002, -281.2799010523970651, -194.5966873725202220 ) ) ;
#80057 = CARTESIAN_POINT ( 'NONE',  ( 26.38301014091384999, -280.9095573587291028, -312.8719403645106922 ) ) ;
#80058 = CARTESIAN_POINT ( 'NONE',  ( -2.820151828116852055, -277.5483514206277391, -338.9401955847702652 ) ) ;
#80059 = DIRECTION ( 'NONE',  ( 0.000000000000000000, 0.000000000000000000, 1.000000000000000000 ) ) ;
#80060 = CARTESIAN_POINT ( 'NONE',  ( 38.93132166715036391, -277.1180885344637659, -273.9914976001100513 ) ) ;
#80061 = CARTESIAN_POINT ( 'NONE',  ( 34.45848030099739390, -290.0519495502701943, -270.3284710469131937 ) ) ;
#80062 = ORIENTED_EDGE ( 'NONE', *, *, #60388, .F. ) ;
#80063 = CARTESIAN_POINT ( 'NONE',  ( -98.52875165703105154, -299.1417535804828276, -226.9889451591008367 ) ) ;
#80064 = CARTESIAN_POINT ( 'NONE',  ( -111.5418660780091784, -276.4613905579420248, -278.9546892281958321 ) ) ;
#80065 = CARTESIAN_POINT ( 'NONE',  ( -113.2380736150634419, -292.2653605256031710, -274.0644277253857126 ) ) ;
#80066 = CARTESIAN_POINT ( 'NONE',  ( 34.05115000947299109, -292.6929597509662244, -254.5884493212009545 ) ) ;
#80067 = CARTESIAN_POINT ( 'NONE',  ( -6.950009051545092298, -288.1715633920741197, -341.0568289601474135 ) ) ;
#80068 = CARTESIAN_POINT ( 'NONE',  ( 165.7865175155837676, 3.000000000000000000, 10.00000000000000000 ) ) ;
#80070 = CARTESIAN_POINT ( 'NONE',  ( -70.59343025827944018, -281.8979763391243409, -336.2597173623353797 ) ) ;
#80069 = CARTESIAN_POINT ( 'NONE',  ( -25.02084843196000463, -293.4728433967881642, -345.8256618156088393 ) ) ;
#80071 = CARTESIAN_POINT ( 'NONE',  ( -42.73031733141778687, -290.9811381663828342, -344.4519477512171761 ) ) ;
#80072 = CARTESIAN_POINT ( 'NONE',  ( -102.8459195714102350, -283.4866994054297038, -236.5986390201078109 ) ) ;
#80073 = CARTESIAN_POINT ( 'NONE',  ( -53.78381593217402923, -284.5826540444174384, -342.0438541648820774 ) ) ;
#80074 = CARTESIAN_POINT ( 'NONE',  ( -17.77270809076263447, -289.7469904409516062, -344.5896486358663537 ) ) ;
#80075 = CARTESIAN_POINT ( 'NONE',  ( 2.732503666583546931, -281.0977861864713532, -209.2099361521545973 ) ) ;
#80076 = CARTESIAN_POINT ( 'NONE',  ( 31.86467039748347574, -292.7715252659738780, -303.3250442930788040 ) ) ;
#80077 = CARTESIAN_POINT ( 'NONE',  ( -9.612048096015215037, -289.5017284635072770, -342.0216037376170561 ) ) ;
#80078 = CARTESIAN_POINT ( 'NONE',  ( -6.938468718123411705, -289.1560986677880010, -341.0518669442762416 ) ) ;
#80079 = CARTESIAN_POINT ( 'NONE',  ( -91.52264768132900485, -285.4201652888505691, -221.3641974463189683 ) ) ;
#80080 = EDGE_LOOP ( 'NONE', ( #71202, #2530 ) ) ;
#80081 = DIRECTION ( 'NONE',  ( 0.000000000000000000, 1.000000000000000000, 0.000000000000000000 ) ) ;
#80082 = CARTESIAN_POINT ( 'NONE',  ( 34.32587455301877810, -295.7292037493839985, -295.0997561477851150 ) ) ;
#80083 = CARTESIAN_POINT ( 'NONE',  ( -79.22110686710806249, -294.2894965469516819, -334.3877808903540085 ) ) ;
#80084 = CARTESIAN_POINT ( 'NONE',  ( -106.6635742540715057, -277.9256354349794833, -246.5858482512796570 ) ) ;
#80085 = CARTESIAN_POINT ( 'NONE',  ( -38.35031144247660251, -273.5474816154490441, -193.4292675775446355 ) ) ;
#80086 = CIRCLE ( 'NONE', #51285, 0.4999999999999941158 ) ;
#80087 = CARTESIAN_POINT ( 'NONE',  ( 32.18782895935710542, -292.3556860749015982, -294.9341212905779344 ) ) ;
#80088 = CARTESIAN_POINT ( 'NONE',  ( -1.247778617471408724, -276.2980201543601879, -205.7307983549780204 ) ) ;
#80089 = CARTESIAN_POINT ( 'NONE',  ( -109.2892990270986502, -294.5653881061557513, -287.7788745015828340 ) ) ;
#80090 = CARTESIAN_POINT ( 'NONE',  ( 35.29853326424126436, -294.6192967123104722, -259.8479358909592065 ) ) ;
#80091 = CARTESIAN_POINT ( 'NONE',  ( 32.92140940047527664, -294.3541533903462550, -249.2740717177885870 ) ) ;
#80092 = CARTESIAN_POINT ( 'NONE',  ( -43.54160339317392214, -248.0334966641272842, -465.6442049081569508 ) ) ;
#80093 = CARTESIAN_POINT ( 'NONE',  ( -108.6156135490662251, -294.2440151454694615, -294.2369989424300343 ) ) ;
#80094 = AXIS2_PLACEMENT_3D ( 'NONE', #38531, #66953, #58469 ) ;
#80095 = CARTESIAN_POINT ( 'NONE',  ( -75.30720031495870614, -275.5466224910248343, -205.6200262841623498 ) ) ;
#80096 = CARTESIAN_POINT ( 'NONE',  ( -107.9820024032772068, -291.7478721366301784, -251.0386920719878106 ) ) ;
#80097 = EDGE_CURVE ( 'NONE', #55253, #38497, #86590, .T. ) ;
#80098 = CARTESIAN_POINT ( 'NONE',  ( -66.05754485226840700, -295.7719048644179907, -337.4989444934502671 ) ) ;
#80099 = EDGE_CURVE ( 'NONE', #21221, #83682, #91168, .T. ) ;
#80100 = CARTESIAN_POINT ( 'NONE',  ( -111.6724978246811872, -280.3737956413369261, -282.7441433713780725 ) ) ;
#80101 = CARTESIAN_POINT ( 'NONE',  ( -113.7404504103645593, -277.1858059388442257, -274.4267331729777197 ) ) ;
#80102 = CARTESIAN_POINT ( 'NONE',  ( 11.72703642815687353, -274.0611899324190972, -211.0840483693015415 ) ) ;
#80103 = CARTESIAN_POINT ( 'NONE',  ( -37.56899974487552640, -281.1349018589069146, -344.8134499908030648 ) ) ;
#80104 = CARTESIAN_POINT ( 'NONE',  ( -68.32835065984754408, -278.0517704925619000, -200.7317423997556887 ) ) ;
#80105 = CARTESIAN_POINT ( 'NONE',  ( -74.08888430577559348, -277.5648361328918554, -204.7892270330569033 ) ) ;
#80106 = CARTESIAN_POINT ( 'NONE',  ( -58.02765650272269227, -296.4640526458672980, -199.8392441719955457 ) ) ;
#80107 = CARTESIAN_POINT ( 'NONE',  ( 20.48984560591109272, -276.8932556611515565, -222.5865882084174530 ) ) ;
#80108 = CARTESIAN_POINT ( 'NONE',  ( 154.4002798831584187, 19.39811195953276624, 12.47990318407953048 ) ) ;
#80109 = CARTESIAN_POINT ( 'NONE',  ( -92.40845807965781944, -287.8548443730286408, -321.8762068854688891 ) ) ;
#80110 = CARTESIAN_POINT ( 'NONE',  ( -38.92017453879579847, -289.0714432507294305, -347.3449371820171905 ) ) ;
#80111 = CARTESIAN_POINT ( 'NONE',  ( -32.81898540040753431, -276.1091532378074476, -195.3177966745486742 ) ) ;
#80112 = CARTESIAN_POINT ( 'NONE',  ( -58.39681337701149033, -295.7791764750614334, -198.5508775564273378 ) ) ;
#80113 = CARTESIAN_POINT ( 'NONE',  ( -111.3387315033606342, -283.4893621971894504, -291.0637305812189766 ) ) ;
#80114 = CARTESIAN_POINT ( 'NONE',  ( 208.4306832106270804, -148.7221692137691491, 0.000000000000000000 ) ) ;
#80115 = CARTESIAN_POINT ( 'NONE',  ( -109.5929642193935081, -282.2926494110877798, -290.5268970055794853 ) ) ;
#80116 = CARTESIAN_POINT ( 'NONE',  ( 150.4957602436334412, 21.00000000000000000, -3.637614988394445081 ) ) ;
#80117 = CARTESIAN_POINT ( 'NONE',  ( 36.03827137829312477, -292.3885319432327492, -273.5212894810681519 ) ) ;
#80118 = CARTESIAN_POINT ( 'NONE',  ( -111.5432735277459670, -282.7207125640397294, -268.1268434742939917 ) ) ;
#80119 = CARTESIAN_POINT ( 'NONE',  ( 208.7651279064949961, 35.82729677688830350, 14.29018184646296064 ) ) ;
#80120 = CARTESIAN_POINT ( 'NONE',  ( 199.0743954165634761, 250.0000000000000568, -2.725891136377211144 ) ) ;
#80121 = CARTESIAN_POINT ( 'NONE',  ( 14.29817831523303973, -290.7778141399049332, -215.9706445410839990 ) ) ;
#80122 = CARTESIAN_POINT ( 'NONE',  ( 38.94829797198683252, -279.9909570234822809, -267.1064333782526319 ) ) ;
#80123 = CARTESIAN_POINT ( 'NONE',  ( -18.79644827916364136, -278.4094885963600632, -341.7930019487720301 ) ) ;
#80124 = CARTESIAN_POINT ( 'NONE',  ( -99.03363885297461877, -286.3646196544299301, -224.8633195040349904 ) ) ;
#80125 = CARTESIAN_POINT ( 'NONE',  ( -27.83655209068037450, -286.1762213677894238, -197.9825841428427964 ) ) ;
#80126 = CARTESIAN_POINT ( 'NONE',  ( -106.8145108695952814, -279.6553779793200647, -294.7828827014006947 ) ) ;
#80127 = CARTESIAN_POINT ( 'NONE',  ( -108.7666267651937062, -279.5642426102505738, -254.4581768557627868 ) ) ;
#80128 = CARTESIAN_POINT ( 'NONE',  ( -108.7727410404889241, -286.2567375100544496, -293.2640244154836751 ) ) ;
#80129 = EDGE_CURVE ( 'NONE', #65802, #83549, #80571, .T. ) ;
#80130 = ORIENTED_EDGE ( 'NONE', *, *, #63139, .F. ) ;
#80131 = CARTESIAN_POINT ( 'NONE',  ( -110.9738579476551195, -271.0862022382013947, -270.3424529284315554 ) ) ;
#80132 = CARTESIAN_POINT ( 'NONE',  ( -110.3463837949087747, -296.0771999330336257, -294.8420527524519912 ) ) ;
#80133 = CARTESIAN_POINT ( 'NONE',  ( 11.20367353736895843, -290.3561906234255616, -327.1321578213385237 ) ) ;
#80134 = LINE ( 'NONE', #72574, #57889 ) ;
#80135 = CARTESIAN_POINT ( 'NONE',  ( -37.37352853689063181, -282.5519495502701375, -190.3611179825600175 ) ) ;
#80136 = CARTESIAN_POINT ( 'NONE',  ( -53.68115742273778324, -278.7676869999617111, -195.3767049647952092 ) ) ;
#80137 = CARTESIAN_POINT ( 'NONE',  ( 23.35053209991907863, -291.3313906738401329, -224.2647721550184201 ) ) ;
#80138 = APPLICATION_CONTEXT ( 'automotive_design' ) ;
#80139 = CARTESIAN_POINT ( 'NONE',  ( 35.64977178790378076, -289.2060730198949727, -280.5997311065902409 ) ) ;
#80140 = CARTESIAN_POINT ( 'NONE',  ( -101.7039054191189393, -280.8059205225195001, -233.8168907828803924 ) ) ;
#80141 = CARTESIAN_POINT ( 'NONE',  ( 38.98795499193628444, -288.9203820230122233, -265.8350665710804037 ) ) ;
#80142 = CARTESIAN_POINT ( 'NONE',  ( -111.8568656840711384, -286.4372592247268017, -279.3219226463848486 ) ) ;
#80143 = CARTESIAN_POINT ( 'NONE',  ( -74.09498055748265699, -277.6933367224073095, -338.0384902650253593 ) ) ;
#80144 = ORIENTED_EDGE ( 'NONE', *, *, #71290, .F. ) ;
#80145 = CARTESIAN_POINT ( 'NONE',  ( -55.67375228488625538, -295.8352728631091395, -197.9489255922306370 ) ) ;
#80146 = CARTESIAN_POINT ( 'NONE',  ( 38.06326802820722577, -291.7033188634103453, -275.9573157861938171 ) ) ;
#80147 = CARTESIAN_POINT ( 'NONE',  ( -59.30011135599711025, -279.6088395333754306, -196.5584880779663877 ) ) ;
#80148 = CARTESIAN_POINT ( 'NONE',  ( -46.35179952655523294, -275.7970394122343123, -196.6747312622376853 ) ) ;
#80149 = CARTESIAN_POINT ( 'NONE',  ( 197.6014737559247578, 297.2619998337689822, -7.302417866276520009 ) ) ;
#80150 = CARTESIAN_POINT ( 'NONE',  ( 35.77081079830085031, -295.8376638359844719, -253.6410175316879361 ) ) ;
#80151 = VECTOR ( 'NONE', #16099, 1000.000000000000000 ) ;
#80152 = CARTESIAN_POINT ( 'NONE',  ( -96.13753662277146361, -271.4471393242510544, -222.2053487180667446 ) ) ;
#80153 = DIRECTION ( 'NONE',  ( 0.000000000000000000, 1.000000000000000000, 0.000000000000000000 ) ) ;
#80154 = CARTESIAN_POINT ( 'NONE',  ( -67.32581511905647176, -279.1556679286080680, -203.7221206800453501 ) ) ;
#80155 = CARTESIAN_POINT ( 'NONE',  ( 34.34473886076967375, -276.4138413316737797, -243.3599479537965919 ) ) ;
#80156 = AXIS2_PLACEMENT_3D ( 'NONE', #70701, #84872, #6772 ) ;
#80157 = CARTESIAN_POINT ( 'NONE',  ( -37.84461360083788151, -299.4710052982822504, -196.7736054746696368 ) ) ;
#80158 = CARTESIAN_POINT ( 'NONE',  ( -114.1199427897994241, -283.5799343416538250, -272.8296707813632338 ) ) ;
#80159 = CARTESIAN_POINT ( 'NONE',  ( 31.43502135199491931, -289.6747800674957602, -297.8442249922160272 ) ) ;
#80160 = CARTESIAN_POINT ( 'NONE',  ( -107.1466815574292042, -298.4705546874687911, -239.4087817870976664 ) ) ;
#80161 = CARTESIAN_POINT ( 'NONE',  ( -26.29642376908139312, -299.3926162173195848, -193.7559832543641676 ) ) ;
#80162 = CARTESIAN_POINT ( 'NONE',  ( 35.86628479080598453, -295.7527175164066762, -285.9345904869593937 ) ) ;
#80163 = CARTESIAN_POINT ( 'NONE',  ( -10.33738327588876160, -280.6989166955122528, -340.2071184104029271 ) ) ;
#80164 = CARTESIAN_POINT ( 'NONE',  ( -57.27717137448740203, -271.8138865034761693, -198.3737510935451098 ) ) ;
#80165 = CARTESIAN_POINT ( 'NONE',  ( -75.72159048767646539, -287.1493804845475211, -204.4715962858715557 ) ) ;
#80166 = CARTESIAN_POINT ( 'NONE',  ( -76.04354887463524904, -288.5028806387017539, -332.6218036277110741 ) ) ;
#80167 = CARTESIAN_POINT ( 'NONE',  ( 7.008222688674750955, -59.14221034369032992, -354.5349928849817047 ) ) ;
#80168 = ORIENTED_EDGE ( 'NONE', *, *, #66060, .F. ) ;
#80169 = CARTESIAN_POINT ( 'NONE',  ( -99.54077770306204798, -289.7193030951328865, -225.9777760355230782 ) ) ;
#80170 = CARTESIAN_POINT ( 'NONE',  ( 27.04710791906520839, -287.6895065801194846, -304.9095252768789237 ) ) ;
#80171 = ORIENTED_EDGE ( 'NONE', *, *, #79023, .T. ) ;
#80172 = CARTESIAN_POINT ( 'NONE',  ( -109.6902236168863567, -285.9540316929830510, -244.9213133778100087 ) ) ;
#80173 = CARTESIAN_POINT ( 'NONE',  ( -85.11587065588825851, -278.0662452395932860, -325.6523288780661574 ) ) ;
#80174 = CARTESIAN_POINT ( 'NONE',  ( 26.24434694608633478, -291.9042219353692644, -227.3921933452214432 ) ) ;
#80175 = CARTESIAN_POINT ( 'NONE',  ( -8.069993360068568933, -283.3302103268970882, -341.5265158149848617 ) ) ;
#80176 = CARTESIAN_POINT ( 'NONE',  ( 36.65413941805682185, -282.8369669917644273, -251.7245012111826270 ) ) ;
#80177 = CARTESIAN_POINT ( 'NONE',  ( -41.56373212361046399, -283.4371014809008216, -347.2764170675583841 ) ) ;
#80178 = CARTESIAN_POINT ( 'NONE',  ( 17.07573733919547365, -281.1890097332741902, -221.6699484925040906 ) ) ;
#80179 = CARTESIAN_POINT ( 'NONE',  ( -107.6853268924600258, -262.6636886874907191, -317.6917322938085704 ) ) ;
#80180 = CARTESIAN_POINT ( 'NONE',  ( -72.49338645575330986, -279.5186622439703683, -336.4390797906424950 ) ) ;
#80181 = CARTESIAN_POINT ( 'NONE',  ( 137.8887718377702924, 180.7638570233321502, -240.9316500215461474 ) ) ;
#80182 = CARTESIAN_POINT ( 'NONE',  ( -103.4369591716781400, -253.6469098985514847, -324.2723498539693878 ) ) ;
#80183 = CARTESIAN_POINT ( 'NONE',  ( -96.40569239111900401, -272.3535803324389803, -227.1023580666451380 ) ) ;
#80184 = CARTESIAN_POINT ( 'NONE',  ( 30.84729256903519712, -292.5984107922258772, -234.6123205805411374 ) ) ;
#80185 = CARTESIAN_POINT ( 'NONE',  ( -61.98066181902706973, -183.2303757086580163, -358.9352458450196082 ) ) ;
#80187 = CARTESIAN_POINT ( 'NONE',  ( -110.2122471344940635, -288.7986271683684549, -282.1165168015188556 ) ) ;
#80186 = CARTESIAN_POINT ( 'NONE',  ( -49.62345859354491040, -272.5836358764456122, -194.7930461374557467 ) ) ;
#80188 = CARTESIAN_POINT ( 'NONE',  ( -91.28884199037489111, -297.6895109085813260, -321.4309179702657389 ) ) ;
#80189 = CARTESIAN_POINT ( 'NONE',  ( 16.38283578654633033, -289.5844050553387206, -320.5845556226929034 ) ) ;
#80190 = EDGE_CURVE ( 'NONE', #87468, #77289, #11889, .T. ) ;
#80191 = ORIENTED_EDGE ( 'NONE', *, *, #22848, .T. ) ;
#80192 = CARTESIAN_POINT ( 'NONE',  ( 0.4351883256169691294, -295.5028322673572347, -337.2023468688740877 ) ) ;
#80193 = CARTESIAN_POINT ( 'NONE',  ( -65.12242340855516431, -286.1715795532335278, -202.7334520378003049 ) ) ;
#80194 = CARTESIAN_POINT ( 'NONE',  ( -107.7880932781080645, -271.8616918610850917, -239.9151886549811650 ) ) ;
#80195 = CARTESIAN_POINT ( 'NONE',  ( 39.55002562315474535, -294.3542157417048770, -270.2998611162381621 ) ) ;
#80196 = CARTESIAN_POINT ( 'NONE',  ( 38.00036713489024010, -293.8485377182907996, -254.7049132343567237 ) ) ;
#80197 = CARTESIAN_POINT ( 'NONE',  ( -44.30231890668056849, -292.1284859796155615, -197.6429084690335003 ) ) ;
#80198 = VERTEX_POINT ( 'NONE', #25620 ) ;
#80199 = CARTESIAN_POINT ( 'NONE',  ( -107.8322266577674640, -274.8251853420545103, -243.0066827198599242 ) ) ;
#80200 = CARTESIAN_POINT ( 'NONE',  ( 37.51436423037964829, -274.5523336267168020, -286.6882126927003469 ) ) ;
#80201 = ORIENTED_EDGE ( 'NONE', *, *, #47293, .F. ) ;
#80202 = CARTESIAN_POINT ( 'NONE',  ( -98.52360622794620326, -278.6824386950880807, -223.6888146327250411 ) ) ;
#80203 = CARTESIAN_POINT ( 'NONE',  ( 35.63577074479621842, -273.8075329434725518, -259.2882534756913628 ) ) ;
#80204 = CARTESIAN_POINT ( 'NONE',  ( -67.19592490814873997, -274.7309592246189709, -203.3925201564745180 ) ) ;
#80205 = CARTESIAN_POINT ( 'NONE',  ( -59.55839499149977456, -274.6986576994674465, -200.5238773939100554 ) ) ;
#80206 = CARTESIAN_POINT ( 'NONE',  ( -30.59351236175934829, -299.7354243006657839, -194.1593107214988549 ) ) ;
#80207 = CARTESIAN_POINT ( 'NONE',  ( 37.50083769667960354, -273.6899737794864222, -279.5724096451319838 ) ) ;
#80208 = CARTESIAN_POINT ( 'NONE',  ( -61.03837610465626540, -296.0193187307580729, -339.5693759385610520 ) ) ;
#80209 = CARTESIAN_POINT ( 'NONE',  ( -20.73269188929812046, -293.4095991504188987, -342.1040560909966644 ) ) ;
#80210 = CARTESIAN_POINT ( 'NONE',  ( 10.19742947581766401, -229.5268262511776527, 22.50000000000000000 ) ) ;
#80211 = CARTESIAN_POINT ( 'NONE',  ( -62.38003365465612404, -277.8615380069998082, -343.1676974463954366 ) ) ;
#80212 = EDGE_CURVE ( 'NONE', #48115, #12757, #9461, .T. ) ;
#80213 = CARTESIAN_POINT ( 'NONE',  ( -36.73820218885698097, -274.2266232278939242, -197.3511976062692383 ) ) ;
#80214 = CARTESIAN_POINT ( 'NONE',  ( -113.4152973157573285, -283.1346413437733531, -278.4916827234015955 ) ) ;
#80215 = CARTESIAN_POINT ( 'NONE',  ( -99.25539156025034515, -299.1289719503383253, -227.7154516038609700 ) ) ;
#80216 = CARTESIAN_POINT ( 'NONE',  ( 29.33919985515026596, -280.8906705383787994, 27.50000000000000000 ) ) ;
#80217 = CARTESIAN_POINT ( 'NONE',  ( -95.88903143520013828, -284.3638118189613806, -226.4884416997613528 ) ) ;
#80218 = CARTESIAN_POINT ( 'NONE',  ( -106.4525652776491285, -277.1426240698747279, -243.7287745173469489 ) ) ;
#80219 = CARTESIAN_POINT ( 'NONE',  ( -68.30170890889883140, -276.0417101773569470, -337.1346427323746298 ) ) ;
#80221 = CARTESIAN_POINT ( 'NONE',  ( -63.64575781744154170, -285.3950444189775340, -340.6511832451976147 ) ) ;
#80220 = AXIS2_PLACEMENT_3D ( 'NONE', #53237, #68391, #66998 ) ;
#80222 = CARTESIAN_POINT ( 'NONE',  ( -13.95336164956255054, -275.5675725956606357, -200.7901748558544170 ) ) ;
#80223 = DIRECTION ( 'NONE',  ( 0.000000000000000000, 1.000000000000000000, 0.000000000000000000 ) ) ;
#80224 = CARTESIAN_POINT ( 'NONE',  ( 36.10898713535917182, -274.2093581135291060, -290.6936308663386512 ) ) ;
#80225 = CIRCLE ( 'NONE', #19730, 4.999999999999986677 ) ;
#80226 = CARTESIAN_POINT ( 'NONE',  ( 0.4301328398136732845, -282.5539307350748572, -205.3148149127621593 ) ) ;
#80227 = CARTESIAN_POINT ( 'NONE',  ( 196.0143093133015384, 19.33012701892218743, 12.49999999999999112 ) ) ;
#80228 = CARTESIAN_POINT ( 'NONE',  ( -67.94045614871654948, -287.5737903070487391, -201.2598868122478279 ) ) ;
#80229 = CARTESIAN_POINT ( 'NONE',  ( 219.8344101925596021, 0.000000000000000000, -10.00000000000000000 ) ) ;
#80230 = CARTESIAN_POINT ( 'NONE',  ( 36.66769178160954112, -291.7089882812107362, -282.5883829289818436 ) ) ;
#80231 = LINE ( 'NONE', #35759, #25469 ) ;
#80232 = CARTESIAN_POINT ( 'NONE',  ( -110.6796442498127959, -271.3090536678539593, -264.8599703506379228 ) ) ;
#80233 = CARTESIAN_POINT ( 'NONE',  ( -104.6667555136829151, -289.1069088302418209, -239.0848906720252387 ) ) ;
#80234 = CARTESIAN_POINT ( 'NONE',  ( -111.6667267435858832, -264.5695759149226092, -294.5014218916285245 ) ) ;
#80235 = CARTESIAN_POINT ( 'NONE',  ( 208.6459800967728029, 38.33095280557449769, 12.00000000000000000 ) ) ;
#80236 = CARTESIAN_POINT ( 'NONE',  ( -71.61258491579592089, -287.9765811947996212, -338.5389311694946173 ) ) ;
#80237 = CARTESIAN_POINT ( 'NONE',  ( -91.16915077849236582, -283.5396100526684222, -216.7273639724238876 ) ) ;
#80238 = CARTESIAN_POINT ( 'NONE',  ( 14.35140715528836708, -283.7336158201786702, -322.8084264783296362 ) ) ;
#80239 = CARTESIAN_POINT ( 'NONE',  ( -64.10494413017759996, -284.2132807828363070, -338.4517230435340593 ) ) ;
#80240 = CARTESIAN_POINT ( 'NONE',  ( -108.3078535115005820, -292.2034030775747055, -295.8575675835909919 ) ) ;
#80241 = CARTESIAN_POINT ( 'NONE',  ( 9.494115164424695053, -275.0098740238670985, -209.2697871955946596 ) ) ;
#80242 = CARTESIAN_POINT ( 'NONE',  ( -20.83524963685109199, -286.9218768133200115, -344.1497659931614521 ) ) ;
#80243 = CARTESIAN_POINT ( 'NONE',  ( 36.58585895124687681, -275.2799926308721297, -248.6407251089134434 ) ) ;
#80244 = CARTESIAN_POINT ( 'NONE',  ( 18.32361299801210563, -296.2279029757397097, -320.1118729048590126 ) ) ;
#80245 = CARTESIAN_POINT ( 'NONE',  ( 222.8344101925596306, -0.9999999999999997780, -21.50000000000000000 ) ) ;
#80246 = CARTESIAN_POINT ( 'NONE',  ( 39.58706461736021254, -296.0519495502702512, -270.3284710469133074 ) ) ;
#80247 = CARTESIAN_POINT ( 'NONE',  ( -37.55868560374530318, -281.7397839320220214, -343.8664639022123310 ) ) ;
#80248 = ADVANCED_FACE ( 'NONE', ( #55926 ), #11424, .F. ) ;
#80249 = CARTESIAN_POINT ( 'NONE',  ( -67.00903156837358665, -275.4399410922380298, -339.4254204402751611 ) ) ;
#80250 = CARTESIAN_POINT ( 'NONE',  ( -33.36573434224945345, -296.5010222906605009, -194.1621739645735829 ) ) ;
#80251 = CARTESIAN_POINT ( 'NONE',  ( 25.45890628494019126, -275.4144418074108671, -307.7773778457732305 ) ) ;
#80252 = CARTESIAN_POINT ( 'NONE',  ( -49.82504212435136282, -293.4102987234782063, -197.6809758967185928 ) ) ;
#80253 = CARTESIAN_POINT ( 'NONE',  ( 34.44475985742116819, -294.3028045848624288, -255.8658562906545058 ) ) ;
#80254 = CARTESIAN_POINT ( 'NONE',  ( -97.41018203397366904, -286.9089084554425426, -227.0988654818618784 ) ) ;
#80255 = CARTESIAN_POINT ( 'NONE',  ( 38.91544896830002642, -295.0482065447483251, -275.9776170493406084 ) ) ;
#80256 = CARTESIAN_POINT ( 'NONE',  ( 23.64606455416303632, -295.4866709973297247, -316.5540918351017012 ) ) ;
#80257 = CARTESIAN_POINT ( 'NONE',  ( -101.2135388009997996, -296.8685677401465455, -235.0144317301369199 ) ) ;
#80258 = CARTESIAN_POINT ( 'NONE',  ( -69.59562228236789849, -291.4768901239034449, -338.0714211808935943 ) ) ;
#80259 = CARTESIAN_POINT ( 'NONE',  ( -76.75607058193615728, -283.7308030991761143, -336.5705545799483502 ) ) ;
#80260 = CARTESIAN_POINT ( 'NONE',  ( -64.99184638603904318, -295.7737370410942503, -199.9860472655927310 ) ) ;
#80261 = CARTESIAN_POINT ( 'NONE',  ( -4.772018107890872329, -286.3027026627996179, -200.5885172166640587 ) ) ;
#80262 = CARTESIAN_POINT ( 'NONE',  ( -59.66336925509197187, -279.3226060761432450, -341.5902544928593443 ) ) ;
#80263 = CARTESIAN_POINT ( 'NONE',  ( -96.07450831871780395, -283.9616337113311602, -226.3430790909038137 ) ) ;
#80264 = CARTESIAN_POINT ( 'NONE',  ( 36.14345053613208592, -285.7445636061790424, -285.3588939529307140 ) ) ;
#80265 = CARTESIAN_POINT ( 'NONE',  ( -35.34445786816251456, -278.2165280338551838, -194.6097177489625096 ) ) ;
#80266 = CARTESIAN_POINT ( 'NONE',  ( -104.1716275211822733, -250.7505522545870349, -322.2422935457555582 ) ) ;
#80267 = CARTESIAN_POINT ( 'NONE',  ( -74.74623378463078893, -285.0472553362163808, -207.6005467327343581 ) ) ;
#80268 = CARTESIAN_POINT ( 'NONE',  ( 30.36364230890859872, -282.2908167408970712, -234.4151928515386203 ) ) ;
#80269 = CARTESIAN_POINT ( 'NONE',  ( -40.34160123200027925, -288.1477208693448802, -347.0802271950327622 ) ) ;
#80270 = CARTESIAN_POINT ( 'NONE',  ( 7.783877076245437010, -278.0478822781354893, -331.8277832818928346 ) ) ;
#80271 = CARTESIAN_POINT ( 'NONE',  ( -70.07472619770953770, -278.7894997382234692, -339.5263640227139490 ) ) ;
#80272 = CARTESIAN_POINT ( 'NONE',  ( -94.78954032507844829, -279.0207439628527482, -225.2994000223949342 ) ) ;
#80273 = CARTESIAN_POINT ( 'NONE',  ( -67.75013453554379339, -275.6310344586611336, -202.1769304475502054 ) ) ;
#80274 = CARTESIAN_POINT ( 'NONE',  ( 13.27847622797138705, -292.7375319914993952, -212.3387279449019900 ) ) ;
#80275 = CARTESIAN_POINT ( 'NONE',  ( 28.46896854776603902, -286.0431605781566304, -305.6960873448949201 ) ) ;
#80276 = CARTESIAN_POINT ( 'NONE',  ( -35.00556872179647883, -293.6811223464127352, -194.1839204647555448 ) ) ;
#80277 = CARTESIAN_POINT ( 'NONE',  ( 34.07343665507487174, -292.6906166228977781, -286.9724706225809427 ) ) ;
#80278 = CARTESIAN_POINT ( 'NONE',  ( 3.824808897341764435, -294.1474630673001229, -330.6720292786783375 ) ) ;
#80279 = CARTESIAN_POINT ( 'NONE',  ( -113.8031090717472438, -291.5492016854806820, -276.9408130151417708 ) ) ;
#80280 = CARTESIAN_POINT ( 'NONE',  ( 15.32707242521286872, -281.4719112464981663, -219.5947011091182901 ) ) ;
#80281 = CARTESIAN_POINT ( 'NONE',  ( -96.74633864127601157, -272.2658958494441208, -221.7205606208881363 ) ) ;
#80282 = CARTESIAN_POINT ( 'NONE',  ( -1.840397811864377342, -289.2457177282461771, -338.5738024391012573 ) ) ;
#80283 = CARTESIAN_POINT ( 'NONE',  ( -104.6970875109252148, -282.2360210423176454, -305.1679800931440809 ) ) ;
#80284 = CARTESIAN_POINT ( 'NONE',  ( 3.172617539209466653, -288.8573406899253087, -335.8784775628997750 ) ) ;
#80285 = CARTESIAN_POINT ( 'NONE',  ( -33.24171314383555398, -286.4383409313013544, -197.4053330546549887 ) ) ;
#80286 = DIRECTION ( 'NONE',  ( 0.000000000000000000, 0.000000000000000000, 1.000000000000000000 ) ) ;
#80287 = CARTESIAN_POINT ( 'NONE',  ( -64.81841035795852690, -181.8926033596262926, -360.5284399092209924 ) ) ;
#80288 = CARTESIAN_POINT ( 'NONE',  ( -62.93877720064744352, -182.6451360637343271, -358.5784724557518075 ) ) ;
#80289 = TOROIDAL_SURFACE ( 'NONE', #42498, 1.000000000000000000, 0.5000000000000000000 ) ;
#80290 = CARTESIAN_POINT ( 'NONE',  ( -81.37693647595384050, -278.6332960281381474, -211.8723474750057107 ) ) ;
#80291 = CARTESIAN_POINT ( 'NONE',  ( -110.2721489523059972, -277.5766063470999825, -262.4339883428488065 ) ) ;
#80292 = CARTESIAN_POINT ( 'NONE',  ( 39.29668692297522625, -275.1216153680238676, -262.5867002607046174 ) ) ;
#80293 = CARTESIAN_POINT ( 'NONE',  ( -87.47509635287066487, -230.6792793315559607, -345.4377264683223530 ) ) ;
#80294 = CIRCLE ( 'NONE', #92372, 5.025000000000002132 ) ;
#80295 = CARTESIAN_POINT ( 'NONE',  ( -42.37299311322092166, -278.5646001980651363, -194.1161680902108344 ) ) ;
#80296 = CARTESIAN_POINT ( 'NONE',  ( -48.60111788454638315, -281.2163224418533218, -344.1518512235516027 ) ) ;
#80297 = CARTESIAN_POINT ( 'NONE',  ( -11.38204671525669376, -296.4788136624466119, -341.8317268058464151 ) ) ;
#80298 = CARTESIAN_POINT ( 'NONE',  ( -87.97775539916428045, -291.8132438612482815, -217.6226238143446494 ) ) ;
#80299 = CARTESIAN_POINT ( 'NONE',  ( -18.36219085221994263, -287.4874003300274694, -341.4142086671831748 ) ) ;
#80300 = CARTESIAN_POINT ( 'NONE',  ( -92.10230355117157330, -273.9460803960664066, -216.3741834594142688 ) ) ;
#80301 = CARTESIAN_POINT ( 'NONE',  ( -103.7194740258367887, -297.1300117867306767, -239.8586718505176805 ) ) ;
#80302 = ORIENTED_EDGE ( 'NONE', *, *, #3249, .T. ) ;
#80303 = DIRECTION ( 'NONE',  ( 0.000000000000000000, 1.000000000000000000, 0.000000000000000000 ) ) ;
#80304 = CARTESIAN_POINT ( 'NONE',  ( -97.44606076710093134, -281.0945497193244478, -224.5494222949722598 ) ) ;
#80305 = EDGE_CURVE ( 'NONE', #21234, #5915, #48804, .T. ) ;
#80306 = CARTESIAN_POINT ( 'NONE',  ( 25.39372497046981536, -282.1107776778738412, -232.3353101186652339 ) ) ;
#80307 = CARTESIAN_POINT ( 'NONE',  ( -90.60256909669053016, -279.5540528342153834, -324.6312179729694094 ) ) ;
#80308 = CARTESIAN_POINT ( 'NONE',  ( -8.683498064682357409, -272.9138382001413561, -202.4140126628049359 ) ) ;
#80309 = CARTESIAN_POINT ( 'NONE',  ( 209.4655899500923510, 29.65170969176866933, 14.77867248455306282 ) ) ;
#80310 = DIRECTION ( 'NONE',  ( -1.000000000000000000, 0.000000000000000000, 0.000000000000000000 ) ) ;
#80311 = CARTESIAN_POINT ( 'NONE',  ( 28.35915969007604787, -275.8326241957810794, -230.4152778563501442 ) ) ;
#80312 = CARTESIAN_POINT ( 'NONE',  ( 30.06914310202902030, -277.9870224728589392, -303.3546937354441866 ) ) ;
#80313 = EDGE_LOOP ( 'NONE', ( #91809, #33250, #6036, #56800 ) ) ;
#80314 = FACE_OUTER_BOUND ( 'NONE', #66921, .T. ) ;
#80315 = CARTESIAN_POINT ( 'NONE',  ( 26.91591439077548387, -284.0586696708265890, -309.8220395367054039 ) ) ;
#80316 = CARTESIAN_POINT ( 'NONE',  ( -65.37940793661114469, -290.8732011608630614, -202.7717755022696622 ) ) ;
#80317 = EDGE_CURVE ( 'NONE', #79467, #3893, #74499, .T. ) ;
#80318 = CARTESIAN_POINT ( 'NONE',  ( 1.477395180076321868, -285.9052545169872701, -203.9651495795492053 ) ) ;
#80319 = CARTESIAN_POINT ( 'NONE',  ( -107.9593265488379075, -282.5023039711295496, -292.5224548648868677 ) ) ;
#80320 = CARTESIAN_POINT ( 'NONE',  ( -59.13984719061074458, -281.9144330792287860, -340.7013610447855285 ) ) ;
#80321 = CARTESIAN_POINT ( 'NONE',  ( 35.42437760287097603, -282.6262815073617389, -260.3802753046105636 ) ) ;
#80322 = CARTESIAN_POINT ( 'NONE',  ( -107.2918065740294793, -270.9055020896462338, -243.1631020823736833 ) ) ;
#80323 = CARTESIAN_POINT ( 'NONE',  ( -92.86275204797011895, -282.2320775502694801, -322.5707998812669075 ) ) ;
#80324 = CARTESIAN_POINT ( 'NONE',  ( -105.3420330841699695, -298.1365789501898576, -301.9989966015293703 ) ) ;
#80325 = CARTESIAN_POINT ( 'NONE',  ( -69.85551414817977900, -280.5543560961490925, -204.7251239632608986 ) ) ;
#80326 = CARTESIAN_POINT ( 'NONE',  ( -110.5793482524169349, -286.7690747077533047, -253.4414451513140136 ) ) ;
#80327 = DIRECTION ( 'NONE',  ( -0.000000000000000000, 1.000000000000000000, -0.000000000000000000 ) ) ;
#80328 = CARTESIAN_POINT ( 'NONE',  ( 21.96236683196131168, -294.8338512104769507, -223.5180015283165744 ) ) ;
#80329 = CARTESIAN_POINT ( 'NONE',  ( -36.46774208992923860, -275.0410765128344792, -345.3688393543887969 ) ) ;
#80330 = CARTESIAN_POINT ( 'NONE',  ( -3.141807029913269655, -287.8091394849486164, -339.1836080373892059 ) ) ;
#80331 = CARTESIAN_POINT ( 'NONE',  ( -0.8434956176400330019, -290.9452581690881630, -206.2035051943412043 ) ) ;
#80332 = CARTESIAN_POINT ( 'NONE',  ( -109.7749611134550065, -277.0730410365456464, -282.8720863332231374 ) ) ;
#80334 = EDGE_CURVE ( 'NONE', #5341, #88648, #67010, .T. ) ;
#80333 = CARTESIAN_POINT ( 'NONE',  ( -95.75989057272919069, -294.0566091649648115, -316.1670183553590618 ) ) ;
#80335 = CARTESIAN_POINT ( 'NONE',  ( -25.34497988736165652, -293.5233098302275607, -197.8018994146434579 ) ) ;
#80336 = CARTESIAN_POINT ( 'NONE',  ( -20.25526795762937127, -276.7662352645559167, -195.3538533559490702 ) ) ;
#80337 = SPHERICAL_SURFACE ( 'NONE', #30687, 2.000000000000000000 ) ;
#80338 = CARTESIAN_POINT ( 'NONE',  ( -74.28778874486029338, -294.0136180977058871, -337.1862663831909117 ) ) ;
#80339 = CARTESIAN_POINT ( 'NONE',  ( 28.95526563748203230, -289.5866738515966858, -302.7826038102975872 ) ) ;
#80340 = CARTESIAN_POINT ( 'NONE',  ( -96.51527554341554094, -288.1442830426971682, -318.0519917138868777 ) ) ;
#80341 = CARTESIAN_POINT ( 'NONE',  ( -13.07659988956628005, -290.1558734470841614, -339.8347088428878919 ) ) ;
#80342 = DIRECTION ( 'NONE',  ( 0.000000000000000000, 0.000000000000000000, 1.000000000000000000 ) ) ;
#80343 = CARTESIAN_POINT ( 'NONE',  ( -98.97229980445470687, -290.8108568269145735, -309.7853606563520543 ) ) ;
#80344 = CARTESIAN_POINT ( 'NONE',  ( 152.4536156746142410, 275.5000000000000568, 14.50000000000000000 ) ) ;
#80345 = CARTESIAN_POINT ( 'NONE',  ( 23.83440981576210760, -289.3742880678108804, -316.4641796154584199 ) ) ;
#80346 = CARTESIAN_POINT ( 'NONE',  ( -93.71421849647849456, -277.2646032648693222, -220.3556585084283199 ) ) ;
#80347 = CARTESIAN_POINT ( 'NONE',  ( -42.43289429708828919, -280.3228697736262802, -193.5508059569522459 ) ) ;
#80348 = VECTOR ( 'NONE', #88868, 1000.000000000000000 ) ;
#80349 = CARTESIAN_POINT ( 'NONE',  ( -77.47786862572245070, -279.1962863488473658, -204.6120280759215859 ) ) ;
#80350 = CARTESIAN_POINT ( 'NONE',  ( 36.54199945121559523, -285.3826938225514596, -257.1757657295149215 ) ) ;
#80351 = CARTESIAN_POINT ( 'NONE',  ( 209.1592146219059885, 29.43398993274398734, 14.70257046291166070 ) ) ;
#80352 = CARTESIAN_POINT ( 'NONE',  ( -96.58339880190602855, -277.3099660019990438, -225.6042841602528028 ) ) ;
#80353 = CARTESIAN_POINT ( 'NONE',  ( -101.2281313779566432, -282.0248365376669994, -309.6488329771750614 ) ) ;
#80354 = CARTESIAN_POINT ( 'NONE',  ( -47.42491241558246173, -156.7151974593914190, -362.7999322911606441 ) ) ;
#80355 = CARTESIAN_POINT ( 'NONE',  ( -82.15488251693280120, -276.1310803426380858, -332.1226467461781340 ) ) ;
#80356 = CARTESIAN_POINT ( 'NONE',  ( -112.0554627081022403, -283.6897415074474225, -253.0594939968741528 ) ) ;
#80357 = CARTESIAN_POINT ( 'NONE',  ( -108.6946458389171966, -273.5677800443384058, -254.1945207536275859 ) ) ;
#80358 = CARTESIAN_POINT ( 'NONE',  ( -52.44703789090385726, -275.2877491416678026, -195.4042534402165927 ) ) ;
#80359 = CARTESIAN_POINT ( 'NONE',  ( 20.85120060232780759, -275.8385673865425929, -314.4709104490390814 ) ) ;
#80360 = CARTESIAN_POINT ( 'NONE',  ( -53.55764435794566936, -297.2602238324482755, -343.6405008410101232 ) ) ;
#80361 = CARTESIAN_POINT ( 'NONE',  ( -57.28885219312510912, -289.4692056267678595, -344.7876629160396078 ) ) ;
#80362 = CARTESIAN_POINT ( 'NONE',  ( 5.390398428577372059, -278.7054708981266913, -208.0451332852020698 ) ) ;
#80363 = CARTESIAN_POINT ( 'NONE',  ( -58.93665064041741175, -291.6135693750293854, -196.4513208183290942 ) ) ;
#80364 = CARTESIAN_POINT ( 'NONE',  ( -15.79382446902911497, -287.8253293910272532, -340.4076635772473196 ) ) ;
#80365 = CARTESIAN_POINT ( 'NONE',  ( -5.431338903037021382, -290.4718106567270866, -202.4882257529098410 ) ) ;
#80366 = ORIENTED_EDGE ( 'NONE', *, *, #7541, .F. ) ;
#80367 = LINE ( 'NONE', #29735, #75620 ) ;
#80368 = CARTESIAN_POINT ( 'NONE',  ( -102.9034113917912805, -289.6232649502455843, -302.6047290959142515 ) ) ;
#80369 = CARTESIAN_POINT ( 'NONE',  ( 175.2296996224750103, 133.0000000000000000, -23.00000000000000711 ) ) ;
#80370 = CARTESIAN_POINT ( 'NONE',  ( 24.50656396498728640, -287.8875341668129408, -224.8901113722191383 ) ) ;
#80371 = CARTESIAN_POINT ( 'NONE',  ( -37.37352853689063181, -288.5519495502701375, -200.3611179825600459 ) ) ;
#80372 = CARTESIAN_POINT ( 'NONE',  ( 0.4142989221714316606, -293.6206321889089850, -337.2141490228852376 ) ) ;
#80373 = CARTESIAN_POINT ( 'NONE',  ( -33.06943442094281949, -284.3145973165848659, -346.7616416610520673 ) ) ;
#80374 = CARTESIAN_POINT ( 'NONE',  ( -65.09125361108934271, -285.5126587298330492, -202.7872229992557038 ) ) ;
#80375 = CARTESIAN_POINT ( 'NONE',  ( 35.59764983834237739, -276.9906568814339494, -279.7729882763896399 ) ) ;
#80376 = CARTESIAN_POINT ( 'NONE',  ( 34.32238351275083943, -291.8429545140094774, -291.2901540116704950 ) ) ;
#80377 = CARTESIAN_POINT ( 'NONE',  ( -46.21163202100608913, -272.7320417375804027, -197.5019743382674164 ) ) ;
#80378 = ORIENTED_EDGE ( 'NONE', *, *, #39536, .T. ) ;
#80379 = CARTESIAN_POINT ( 'NONE',  ( 202.9737475146022803, 296.4636489462809550, -68.70538243550777224 ) ) ;
#80380 = CARTESIAN_POINT ( 'NONE',  ( 33.39546151682874608, -293.6072486570630531, -300.8601426496741738 ) ) ;
#80381 = CARTESIAN_POINT ( 'NONE',  ( -30.42129283807700801, -288.0603702630351677, -196.1916943921049494 ) ) ;
#80382 = CARTESIAN_POINT ( 'NONE',  ( -95.34636527920996230, -298.3129103428891540, -220.1126156360013795 ) ) ;
#80383 = CARTESIAN_POINT ( 'NONE',  ( 16.04324499545989369, -287.4859282217960867, -220.4032817418305967 ) ) ;
#80384 = CARTESIAN_POINT ( 'NONE',  ( -72.74286869506777009, -276.5680991823698491, -338.4902217201118333 ) ) ;
#80385 = CARTESIAN_POINT ( 'NONE',  ( -8.418668381705955994, -295.3348644015867421, -341.6689911046485690 ) ) ;
#80386 = CARTESIAN_POINT ( 'NONE',  ( 15.80238528944281562, -286.4492852364213036, -324.4341564320301927 ) ) ;
#80387 = CARTESIAN_POINT ( 'NONE',  ( 39.20462864995405994, -293.7773845494611464, -261.7240737623294535 ) ) ;
#80388 = CARTESIAN_POINT ( 'NONE',  ( -37.55427151558518517, -292.3827367420563519, -197.3278360403185445 ) ) ;
#80389 = FACE_BOUND ( 'NONE', #83214, .T. ) ;
#80390 = DIRECTION ( 'NONE',  ( -1.000000000000000000, 0.000000000000000000, 0.000000000000000000 ) ) ;
#80391 = CARTESIAN_POINT ( 'NONE',  ( 173.9547979362525894, 240.3581496378278928, -177.1551773923532380 ) ) ;
#80392 = CARTESIAN_POINT ( 'NONE',  ( -23.92699244239541656, -287.7405087752162558, -195.1891291902018395 ) ) ;
#80393 = CARTESIAN_POINT ( 'NONE',  ( -111.2586520408596868, -288.4809262143061801, -234.7283546768995564 ) ) ;
#80394 = ORIENTED_EDGE ( 'NONE', *, *, #5869, .F. ) ;
#80395 = CARTESIAN_POINT ( 'NONE',  ( -114.1086100312523115, -277.9569603705388658, -265.8717605420122254 ) ) ;
#80396 = CARTESIAN_POINT ( 'NONE',  ( 23.59186286994720660, -282.9602990343876741, -226.9200161494502765 ) ) ;
#80397 = CARTESIAN_POINT ( 'NONE',  ( -75.66117004219593412, -209.4785753004333060, -356.0246882555991306 ) ) ;
#80398 = CARTESIAN_POINT ( 'NONE',  ( -110.3575498293441512, -283.4139577534669456, -247.6600260010800127 ) ) ;
#80399 = CARTESIAN_POINT ( 'NONE',  ( -69.39985025201343660, -287.5572103574889979, -337.5443689650706460 ) ) ;
#80400 = CARTESIAN_POINT ( 'NONE',  ( -52.32491076153355181, -275.7228227631503614, -196.0390550074943690 ) ) ;
#80401 = CARTESIAN_POINT ( 'NONE',  ( -63.10703266408297907, -298.1998052001035262, -201.9399374625336634 ) ) ;
#80402 = CARTESIAN_POINT ( 'NONE',  ( 31.99980827499022951, -292.5606009983550848, -294.8649601378671719 ) ) ;
#80403 = CARTESIAN_POINT ( 'NONE',  ( -82.47973865649710490, -278.3022659419894467, -332.6176057095522651 ) ) ;
#80404 = CARTESIAN_POINT ( 'NONE',  ( -40.50576614797915909, -277.0930097537486176, -343.3049794409141100 ) ) ;
#80405 = CARTESIAN_POINT ( 'NONE',  ( 32.26669578359336299, -276.2168914236885371, -238.0452073168526965 ) ) ;
#80406 = CARTESIAN_POINT ( 'NONE',  ( -101.8444841358155060, -276.9249240674079147, -311.9415778431463195 ) ) ;
#80407 = CARTESIAN_POINT ( 'NONE',  ( 121.2562179576807182, 149.7689830916746132, -263.4557525059072987 ) ) ;
#80408 = CARTESIAN_POINT ( 'NONE',  ( 37.31200593526440201, -273.6510444178789498, -278.0757982587296624 ) ) ;
#80409 = CARTESIAN_POINT ( 'NONE',  ( -111.0584898532366793, -298.2334702563796895, -250.0547052613120229 ) ) ;
#80410 = EDGE_CURVE ( 'NONE', #87519, #77887, #79119, .T. ) ;
#80411 = CARTESIAN_POINT ( 'NONE',  ( 120.8395553409046528, -299.5541904835127980, -195.3611179825600175 ) ) ;
#80412 = AXIS2_PLACEMENT_3D ( 'NONE', #41520, #25458, #54337 ) ;
#80413 = CARTESIAN_POINT ( 'NONE',  ( 197.2116108777964030, 281.1590520725322335, -110.1526527170710921 ) ) ;
#80414 = VECTOR ( 'NONE', #63150, 1000.000000000000000 ) ;
#80415 = CARTESIAN_POINT ( 'NONE',  ( -35.94129136253315693, -287.1497999163134409, -197.0653818867000666 ) ) ;
#80416 = CARTESIAN_POINT ( 'NONE',  ( -95.48033407271157103, -285.6444370434724647, -319.3084668643841155 ) ) ;
#80417 = CARTESIAN_POINT ( 'NONE',  ( -6.966591636280974775, -285.8101783584715463, -203.8549245842454525 ) ) ;
#80418 = CARTESIAN_POINT ( 'NONE',  ( -109.6672316798495501, -277.1443828610991318, -255.6192592588039076 ) ) ;
#80419 = CARTESIAN_POINT ( 'NONE',  ( -83.54530099275037003, -285.5535512368696800, -328.5312171824938332 ) ) ;
#80420 = CARTESIAN_POINT ( 'NONE',  ( -36.98573078637099343, -278.5365660730943773, -196.6686418364928954 ) ) ;
#80421 = CARTESIAN_POINT ( 'NONE',  ( 16.76856215522951032, -277.3384903137818469, -319.8399865519692753 ) ) ;
#80422 = CARTESIAN_POINT ( 'NONE',  ( 199.4894028483730892, 67.51180740859732055, -8.507532329691386508 ) ) ;
#80423 = CARTESIAN_POINT ( 'NONE',  ( -38.08927566288137001, -274.5348830603441002, -197.3034039977275143 ) ) ;
#80424 = AXIS2_PLACEMENT_3D ( 'NONE', #13640, #86044, #70934 ) ;
#80425 = CARTESIAN_POINT ( 'NONE',  ( 32.25049177970687708, -282.7743620575975569, -303.0608178681232516 ) ) ;
#80426 = CARTESIAN_POINT ( 'NONE',  ( 38.36614193868619083, -282.2169607911520188, -284.1401498912176748 ) ) ;
#80427 = ORIENTED_EDGE ( 'NONE', *, *, #29447, .F. ) ;
#80428 = DIRECTION ( 'NONE',  ( 0.000000000000000000, 0.000000000000000000, -1.000000000000000000 ) ) ;
#80429 = CARTESIAN_POINT ( 'NONE',  ( 36.17248540290382408, -289.1795047701587009, -252.0316332790257263 ) ) ;
#80430 = CARTESIAN_POINT ( 'NONE',  ( -69.16753465296453385, -288.1469122262101337, -339.9485386121825741 ) ) ;
#80431 = CARTESIAN_POINT ( 'NONE',  ( -105.1153225178908457, -295.3810106964807574, -297.9172032399425234 ) ) ;
#80432 = EDGE_CURVE ( 'NONE', #76874, #75355, #68489, .T. ) ;
#80433 = CARTESIAN_POINT ( 'NONE',  ( -16.64606417490007573, -291.6613192706734026, -196.3003089214249428 ) ) ;
#80434 = CARTESIAN_POINT ( 'NONE',  ( 35.68588608369223181, -285.8979943897359135, -260.1043834399056891 ) ) ;
#80435 = CARTESIAN_POINT ( 'NONE',  ( -13.14256136205505321, -289.9357123768817814, -339.6542070136081293 ) ) ;
#80436 = CARTESIAN_POINT ( 'NONE',  ( 35.78497577281001440, -290.2662352645559167, -287.0191576251351080 ) ) ;
#80437 = CARTESIAN_POINT ( 'NONE',  ( 4.464181403716226626, -290.4882716861552012, -332.6288376780019576 ) ) ;
#80438 = CARTESIAN_POINT ( 'NONE',  ( -107.1065809924027832, -288.1882506233327490, -298.3412863548136897 ) ) ;
#80439 = CARTESIAN_POINT ( 'NONE',  ( -104.8190044365329783, -285.8757709481660640, -241.7663236748392137 ) ) ;
#80440 = CARTESIAN_POINT ( 'NONE',  ( -94.28903256405652655, -293.2310981013047808, -221.2799465756962149 ) ) ;
#80441 = CARTESIAN_POINT ( 'NONE',  ( 82.14777765880957361, -299.6392946510901538, -193.3583333091573024 ) ) ;
#80442 = CARTESIAN_POINT ( 'NONE',  ( 154.7659666677267580, 19.56018909072084710, -12.94946946941271193 ) ) ;
#80443 = CARTESIAN_POINT ( 'NONE',  ( -4.223111377502405617, -300.3838190910971093, -194.7903730022934212 ) ) ;
#80444 = CARTESIAN_POINT ( 'NONE',  ( 26.99219641010665072, -281.2236307810478593, -305.2000542853050433 ) ) ;
#80445 = CARTESIAN_POINT ( 'NONE',  ( -97.54190663980156728, -281.9413254717118775, -315.0929387312118024 ) ) ;
#80446 = CARTESIAN_POINT ( 'NONE',  ( 4.131521613627292311, -293.7060280716325451, -335.1086144417380979 ) ) ;
#80447 = CARTESIAN_POINT ( 'NONE',  ( -58.11061667493238048, -296.1791441561043143, -199.5438000516386978 ) ) ;
#80448 = CARTESIAN_POINT ( 'NONE',  ( 36.04941310175368585, -273.4699264072118012, -257.8330058180659421 ) ) ;
#80449 = CARTESIAN_POINT ( 'NONE',  ( -39.19745702385484520, -299.3435906741805752, -196.8789062610658789 ) ) ;
#80450 = DIRECTION ( 'NONE',  ( 0.000000000000000000, 0.000000000000000000, 1.000000000000000000 ) ) ;
#80451 = CARTESIAN_POINT ( 'NONE',  ( -58.58974257309292710, -293.5629331337668191, -343.3713931510915245 ) ) ;
#80452 = CARTESIAN_POINT ( 'NONE',  ( 21.00137245474618908, -295.6037587686863048, -315.2310679839309273 ) ) ;
#80453 = CARTESIAN_POINT ( 'NONE',  ( 152.4536156746142410, 250.0000000000000568, 12.00000000000000000 ) ) ;
#80454 = CARTESIAN_POINT ( 'NONE',  ( -45.09771127264434654, -295.9555775853328328, -343.1609055890218656 ) ) ;
#80455 = CARTESIAN_POINT ( 'NONE',  ( 175.2296996224750103, 138.1603916158177583, 0.000000000000000000 ) ) ;
#80457 = CARTESIAN_POINT ( 'NONE',  ( -110.2122864278408088, -296.6094678515987653, -266.0162759452346677 ) ) ;
#80456 = CARTESIAN_POINT ( 'NONE',  ( -70.32309218439492327, -283.6397327715861820, -202.6068960799756269 ) ) ;
#80458 = CARTESIAN_POINT ( 'NONE',  ( -90.43813906124488256, -283.7787744412349298, -326.1995223562259412 ) ) ;
#80459 = CARTESIAN_POINT ( 'NONE',  ( -33.11439856564233253, -284.9194796525828792, -345.8156675511369826 ) ) ;
#80460 = CARTESIAN_POINT ( 'NONE',  ( 39.55676283843872199, -287.1621116446310680, -265.8238749039458639 ) ) ;
#80461 = CARTESIAN_POINT ( 'NONE',  ( -49.97374396222253523, -289.8905829047055818, -196.5490323371649026 ) ) ;
#80462 = CARTESIAN_POINT ( 'NONE',  ( -114.2830456889115283, -277.8852448426526394, -271.5984660748050601 ) ) ;
#80463 = CARTESIAN_POINT ( 'NONE',  ( -20.25526795762938548, -280.3380690714490129, -345.3683826091709648 ) ) ;
#80464 = CARTESIAN_POINT ( 'NONE',  ( -43.21050657630429015, -280.7973232067119511, -507.6442049081570076 ) ) ;
#80465 = CARTESIAN_POINT ( 'NONE',  ( 2.676288913461658314, -285.3971049422937085, -208.8331482667363446 ) ) ;
#80466 = CARTESIAN_POINT ( 'NONE',  ( -114.0809738918028415, -289.4618034756450129, -271.2115513902590465 ) ) ;
#80467 = CYLINDRICAL_SURFACE ( 'NONE', #56675, 0.5000000000000004441 ) ;
#80468 = CARTESIAN_POINT ( 'NONE',  ( -84.48844452273480954, -279.1118058660972565, -330.5597836848743327 ) ) ;
#80470 = CARTESIAN_POINT ( 'NONE',  ( 35.44972627992955694, -281.3032196759601220, -276.7572149369767658 ) ) ;
#80469 = CARTESIAN_POINT ( 'NONE',  ( 10.14190292920483571, -292.4217283055657504, -328.9408569670604834 ) ) ;
#80471 = CARTESIAN_POINT ( 'NONE',  ( -65.60152216666924119, -295.5783124372812836, -342.0020279719682890 ) ) ;
#80472 = CARTESIAN_POINT ( 'NONE',  ( -21.26604080751098280, -284.3366451853988224, -196.5309928806887854 ) ) ;
#80473 = CARTESIAN_POINT ( 'NONE',  ( -97.00133783835995871, -281.1745431884944537, -224.8899053083866022 ) ) ;
#80474 = CARTESIAN_POINT ( 'NONE',  ( -61.10079790909031772, -294.4269101495706877, -339.6890607983842187 ) ) ;
#80475 = CIRCLE ( 'NONE', #51743, 0.5000000000000004441 ) ;
#80476 = EDGE_LOOP ( 'NONE', ( #86350, #35455, #15061, #45465 ) ) ;
#80478 = CARTESIAN_POINT ( 'NONE',  ( 21.80409003338201757, -282.9050155244781308, -224.8033104702516596 ) ) ;
#80477 = CIRCLE ( 'NONE', #24517, 20.00000000000000355 ) ;
#80479 = CARTESIAN_POINT ( 'NONE',  ( -92.24105611647941316, -295.3722227420502691, -318.5695109638613758 ) ) ;
#80480 = FACE_OUTER_BOUND ( 'NONE', #29278, .T. ) ;
#80481 = CARTESIAN_POINT ( 'NONE',  ( -37.30987171927208834, -271.5523547857346784, -195.3611179825600175 ) ) ;
#80482 = CARTESIAN_POINT ( 'NONE',  ( -31.26262375507214131, -273.3242338649308749, -193.7501905062934782 ) ) ;
#80483 = AXIS2_PLACEMENT_3D ( 'NONE', #17808, #46661, #75565 ) ;
#80484 = CARTESIAN_POINT ( 'NONE',  ( -110.2455214899932798, -290.4465169825947441, -265.7335031654978934 ) ) ;
#80485 = AXIS2_PLACEMENT_3D ( 'NONE', #67778, #37934, #75802 ) ;
#80486 = CARTESIAN_POINT ( 'NONE',  ( -107.8964668889480265, -280.3513288828779082, -249.0836030836581187 ) ) ;
#80487 = CARTESIAN_POINT ( 'NONE',  ( -63.61031775373006525, -275.3041149511859089, -201.3808152747057250 ) ) ;
#80488 = CARTESIAN_POINT ( 'NONE',  ( -10.95968650386789456, -284.3141344996183193, -341.9044519121607664 ) ) ;
#80489 = CARTESIAN_POINT ( 'NONE',  ( 22.90196310605353247, -280.9283076389849612, -312.2876196893815859 ) ) ;
#80490 = CARTESIAN_POINT ( 'NONE',  ( -10.51552069001263767, -278.7023282810374099, -340.3993699997536737 ) ) ;
#80491 = ORIENTED_EDGE ( 'NONE', *, *, #47293, .T. ) ;
#80492 = CARTESIAN_POINT ( 'NONE',  ( -83.57839670604047910, -273.2711561646557357, -208.7219258140593183 ) ) ;
#80493 = CARTESIAN_POINT ( 'NONE',  ( -30.70241951479907172, -294.0568993822982407, -196.2177828088900924 ) ) ;
#80494 = CARTESIAN_POINT ( 'NONE',  ( 184.7149167944524493, -12.49482340714361506, 10.00000000000000000 ) ) ;
#80495 = EDGE_CURVE ( 'NONE', #85558, #71226, #11026, .T. ) ;
#80496 = LINE ( 'NONE', #31715, #49676 ) ;
#80497 = CARTESIAN_POINT ( 'NONE',  ( 37.13855748948093094, -291.8692051104629286, -284.3234284192116661 ) ) ;
#80498 = CARTESIAN_POINT ( 'NONE',  ( 0.6498149643088227956, -274.0813040891083006, -207.9541213986141202 ) ) ;
#80499 = DIRECTION ( 'NONE',  ( 1.000000000000000000, 0.000000000000000000, 0.000000000000000000 ) ) ;
#80500 = CARTESIAN_POINT ( 'NONE',  ( 21.66073268931555873, -294.4165452876623590, -221.9728892809098397 ) ) ;
#80502 = CARTESIAN_POINT ( 'NONE',  ( 20.07086434238075512, -294.0667192088826596, -219.6283270696731620 ) ) ;
#80501 = CARTESIAN_POINT ( 'NONE',  ( 35.78497577281001440, -284.2662352645559167, -287.0191576251351080 ) ) ;
#80503 = CARTESIAN_POINT ( 'NONE',  ( 25.04882278313685617, -288.9919255906511353, -228.9460324083932221 ) ) ;
#80504 = CARTESIAN_POINT ( 'NONE',  ( 35.36177123535527045, -273.7807801538256740, -288.1416578014884635 ) ) ;
#80505 = CARTESIAN_POINT ( 'NONE',  ( -95.56432010041648084, -279.8296776350105119, -316.7650966909973249 ) ) ;
#80506 = CARTESIAN_POINT ( 'NONE',  ( 29.68062272051770023, -292.0633109964564937, -302.8731578813580541 ) ) ;
#80507 = CARTESIAN_POINT ( 'NONE',  ( -64.32493405691835164, -281.5643069343833531, -199.5088151790409086 ) ) ;
#80508 = ORIENTED_EDGE ( 'NONE', *, *, #67393, .T. ) ;
#80509 = CARTESIAN_POINT ( 'NONE',  ( -7.248640754685577114, -282.3129547156637500, -336.9067467155135773 ) ) ;
#80510 = CARTESIAN_POINT ( 'NONE',  ( -2.542737627392792632, -281.5811468724717770, -202.0052132104664224 ) ) ;
#80511 = CARTESIAN_POINT ( 'NONE',  ( 19.47861533819587265, -281.0490526915993428, -321.8143843649933160 ) ) ;
#80512 = CARTESIAN_POINT ( 'NONE',  ( 16.79780885321362405, -277.2457933745729406, -324.8571691315373187 ) ) ;
#80513 = CARTESIAN_POINT ( 'NONE',  ( 16.48004871398853410, -277.8245700654148322, -324.5267599171917254 ) ) ;
#80514 = CARTESIAN_POINT ( 'NONE',  ( 17.40634833298267736, -290.6948066931273047, -313.9805196606274080 ) ) ;
#80515 = ORIENTED_EDGE ( 'NONE', *, *, #37424, .T. ) ;
#80516 = CARTESIAN_POINT ( 'NONE',  ( -100.8494858809941945, -275.0852220125138956, -230.7784251220282954 ) ) ;
#80517 = CARTESIAN_POINT ( 'NONE',  ( -92.79931105088246568, -292.3120855462549343, -222.4165722550149553 ) ) ;
#80518 = CARTESIAN_POINT ( 'NONE',  ( -57.05837417821064150, -275.3276975731592415, -342.4085511733431417 ) ) ;
#80519 = CARTESIAN_POINT ( 'NONE',  ( -83.66655920297384341, -293.1868952341234262, -210.0620601716347551 ) ) ;
#80520 = CARTESIAN_POINT ( 'NONE',  ( -44.30166299510289463, -291.3105246390647380, -197.5403758345906908 ) ) ;
#80521 = CARTESIAN_POINT ( 'NONE',  ( 32.80619832535118974, -287.4638201614991431, -301.9649032878892854 ) ) ;
#80522 = DIRECTION ( 'NONE',  ( 0.000000000000000000, 0.000000000000000000, 1.000000000000000000 ) ) ;
#80524 = CARTESIAN_POINT ( 'NONE',  ( -74.21397431897129593, -281.9504627172444202, -334.3480382853597916 ) ) ;
#80523 = CARTESIAN_POINT ( 'NONE',  ( 37.19062703920061352, -291.9140051033854775, -253.4637887561008824 ) ) ;
#80525 = CARTESIAN_POINT ( 'NONE',  ( -89.51258808471089878, -291.6574094978146832, -323.1727069473811866 ) ) ;
#80526 = CARTESIAN_POINT ( 'NONE',  ( -108.7699837978218227, -282.7949836016989593, -288.4914253758695963 ) ) ;
#80527 = CARTESIAN_POINT ( 'NONE',  ( 5.195047542884161373, -281.9563291684947330, -210.4289181696981075 ) ) ;
#80528 = CARTESIAN_POINT ( 'NONE',  ( -82.70392661974192094, -290.5967950665985313, -332.2892103158422401 ) ) ;
#80529 = CARTESIAN_POINT ( 'NONE',  ( -37.01433908642785298, -280.5487093557175626, -197.3003126446141380 ) ) ;
#80530 = CARTESIAN_POINT ( 'NONE',  ( -53.29158176090530219, -290.6470509080520515, -195.3828751425093913 ) ) ;
#80531 = CARTESIAN_POINT ( 'NONE',  ( 39.19284466788963073, -288.2622599756758177, -262.9626194424529331 ) ) ;
#80532 = CARTESIAN_POINT ( 'NONE',  ( -9.579682989452575015, -289.1912931772486672, -342.1162384104836178 ) ) ;
#80533 = CARTESIAN_POINT ( 'NONE',  ( -98.10824280512076712, -285.2803906610940885, -229.9083393933848072 ) ) ;
#80534 = VERTEX_POINT ( 'NONE', #5280 ) ;
#80535 = CARTESIAN_POINT ( 'NONE',  ( 73.43068321062709458, -134.2391364535880598, 5.025000000000002132 ) ) ;
#80536 = CARTESIAN_POINT ( 'NONE',  ( 29.81855179686944268, -295.8723563734035338, -305.4297084771415598 ) ) ;
#80537 = CARTESIAN_POINT ( 'NONE',  ( -112.1266786164127041, -295.0338279995000335, -286.5012935480532974 ) ) ;
#80538 = CARTESIAN_POINT ( 'NONE',  ( -59.27685380260552961, -276.4019323726130324, -340.2342707734032956 ) ) ;
#80539 = CARTESIAN_POINT ( 'NONE',  ( -97.26169597338578399, -296.5475338491443722, -222.1645736553807069 ) ) ;
#80540 = CARTESIAN_POINT ( 'NONE',  ( 35.89370717058314852, -292.1450562789697187, -279.0109597219382636 ) ) ;
#80541 = CARTESIAN_POINT ( 'NONE',  ( -110.0367799803427573, -294.9738275315411897, -256.3869132325944520 ) ) ;
#80542 = AXIS2_PLACEMENT_3D ( 'NONE', #83104, #90654, #46649 ) ;
#80543 = CARTESIAN_POINT ( 'NONE',  ( 11.18187833525152719, -293.9468005860555309, -215.2243293110636841 ) ) ;
#80544 = CARTESIAN_POINT ( 'NONE',  ( 35.51573438171101316, -294.7444306034954593, -278.9330883976203381 ) ) ;
#80545 = CARTESIAN_POINT ( 'NONE',  ( 160.5350683151633291, 276.0000000000000568, 20.22542485937379908 ) ) ;
#80546 = CARTESIAN_POINT ( 'NONE',  ( -52.93441530482945012, -293.2512535407890368, -343.9459628040423809 ) ) ;
#80547 = CARTESIAN_POINT ( 'NONE',  ( -98.39224404850024541, -297.9596389803091938, -313.9469477613181425 ) ) ;
#80548 = CARTESIAN_POINT ( 'NONE',  ( -100.5008205084786255, -290.9847986763157905, -307.5329838529258382 ) ) ;
#80550 = CARTESIAN_POINT ( 'NONE',  ( -47.79186814010511597, -295.5218504549019940, -342.6819182620483843 ) ) ;
#80549 = VECTOR ( 'NONE', #10927, 1000.000000000000000 ) ;
#80551 = TOROIDAL_SURFACE ( 'NONE', #4936, 12.68950434577434372, 1.000000000000000000 ) ;
#80552 = CARTESIAN_POINT ( 'NONE',  ( -111.1126357630462991, -280.7292592624842200, -254.9281716746444317 ) ) ;
#80553 = CARTESIAN_POINT ( 'NONE',  ( -39.55609598073227318, -278.7097562860465132, -193.8733526945460142 ) ) ;
#80554 = EDGE_LOOP ( 'NONE', ( #51241, #25792, #12648, #48682 ) ) ;
#80555 = EDGE_CURVE ( 'NONE', #90280, #50719, #26176, .T. ) ;
#80556 = CARTESIAN_POINT ( 'NONE',  ( -105.5147294886371014, -272.3616035552637413, -234.6686622686278270 ) ) ;
#80557 = CARTESIAN_POINT ( 'NONE',  ( 29.43217052193039862, -280.0706172615243190, -303.3803670117515026 ) ) ;
#80558 = CARTESIAN_POINT ( 'NONE',  ( -50.77833853402099606, -278.2831164257214027, -195.3551371415321682 ) ) ;
#80559 = CARTESIAN_POINT ( 'NONE',  ( -97.93452628516635627, -277.1574277938487967, -225.8586463041476122 ) ) ;
#80560 = EDGE_CURVE ( 'NONE', #81908, #70640, #64073, .T. ) ;
#80561 = CARTESIAN_POINT ( 'NONE',  ( -69.45802370942078596, -296.3051561188211735, -204.2567668449932512 ) ) ;
#80562 = CARTESIAN_POINT ( 'NONE',  ( -107.3696834841678367, -274.9030493279105940, -243.3659817668374217 ) ) ;
#80563 = CARTESIAN_POINT ( 'NONE',  ( 170.2299524499825338, 214.9970011440366875, -24.94063848305468412 ) ) ;
#80564 = CARTESIAN_POINT ( 'NONE',  ( -93.46899604827929409, -289.2692449370394456, -220.0805704832913534 ) ) ;
#80565 = CARTESIAN_POINT ( 'NONE',  ( -99.87026735700776214, -289.9563016343895470, -315.3189756387700982 ) ) ;
#80566 = CARTESIAN_POINT ( 'NONE',  ( 28.33301635610003544, -277.0655372037653024, -233.6910553124743899 ) ) ;
#80567 = CARTESIAN_POINT ( 'NONE',  ( 98.59996038885898884, -297.7573711738884299, -195.5742745502984405 ) ) ;
#80568 = CARTESIAN_POINT ( 'NONE',  ( -93.79414022174815102, -284.4612531227237469, -218.1556073756473779 ) ) ;
#80569 = DIRECTION ( 'NONE',  ( -0.000000000000000000, -0.000000000000000000, 1.000000000000000000 ) ) ;
#80570 = CARTESIAN_POINT ( 'NONE',  ( 37.61795415412644417, -279.5995653411679882, -274.0665912484985824 ) ) ;
#80571 = CIRCLE ( 'NONE', #89618, 0.4999999999999960587 ) ;
#80572 = DIRECTION ( 'NONE',  ( 0.000000000000000000, 0.000000000000000000, 1.000000000000000000 ) ) ;
#80573 = CARTESIAN_POINT ( 'NONE',  ( -25.32906956490525374, -291.0034657668256273, -197.9019878005229600 ) ) ;
#80574 = CARTESIAN_POINT ( 'NONE',  ( -95.06784649677790355, -283.3410888418707714, -223.6659595435774577 ) ) ;
#80575 = DIRECTION ( 'NONE',  ( -0.9893575751536619611, 0.000000000000000000, -0.1455045995357745758 ) ) ;
#80576 = CARTESIAN_POINT ( 'NONE',  ( 140.6539576904058606, 0.000000000000000000, 10.50000000000000000 ) ) ;
#80577 = CARTESIAN_POINT ( 'NONE',  ( -2.690176148231683939, -290.5102143201916078, -203.8459126714049319 ) ) ;
#80578 = CARTESIAN_POINT ( 'NONE',  ( -104.9967143010387360, -279.7586346608056260, -299.9719555851846167 ) ) ;
#80579 = CARTESIAN_POINT ( 'NONE',  ( -63.76060060907820315, -284.5941626205424768, -342.2641806131185263 ) ) ;
#80581 = CARTESIAN_POINT ( 'NONE',  ( -46.72486963953097217, -285.9298474866923812, -197.9158943556960537 ) ) ;
#80580 = CARTESIAN_POINT ( 'NONE',  ( -38.31388983956673400, -272.1199058179613530, -194.8073685777292781 ) ) ;
#80582 = CARTESIAN_POINT ( 'NONE',  ( 25.77191610591306059, -276.4598782102235646, -232.4200678694771511 ) ) ;
#80583 = CARTESIAN_POINT ( 'NONE',  ( 20.15570014322869241, -276.9919311133270412, -315.6212204323905439 ) ) ;
#80584 = CARTESIAN_POINT ( 'NONE',  ( -112.3537271438698042, -286.5208734590051449, -272.8100192037657621 ) ) ;
#80585 = ORIENTED_EDGE ( 'NONE', *, *, #73503, .F. ) ;
#80586 = CARTESIAN_POINT ( 'NONE',  ( 195.0629117428269126, 293.9636489450776367, -40.00000000000000711 ) ) ;
#80587 = CARTESIAN_POINT ( 'NONE',  ( -107.1672644957429270, -295.9700871516866982, -302.8170968650683221 ) ) ;
#80588 = CARTESIAN_POINT ( 'NONE',  ( 21.62482275452285307, -288.9015482929277141, -224.5921767046817763 ) ) ;
#80589 = CARTESIAN_POINT ( 'NONE',  ( 196.3889435609981149, 25.22386505340214669, 13.78671447301574915 ) ) ;
#80590 = CARTESIAN_POINT ( 'NONE',  ( 108.6256185021308909, -297.2649936051623740, -190.4191791630918544 ) ) ;
#80591 = CARTESIAN_POINT ( 'NONE',  ( -86.59563202631936463, -278.3068472571135317, -211.5080469909619296 ) ) ;
#80592 = CARTESIAN_POINT ( 'NONE',  ( -36.36790730807192773, -290.4640483067564105, -194.1544403441316433 ) ) ;
#80593 = CARTESIAN_POINT ( 'NONE',  ( -104.1218797046931996, -286.4905413017955880, -239.0773581735443543 ) ) ;
#80594 = CARTESIAN_POINT ( 'NONE',  ( -57.40919467121199915, -281.5497210430205541, -199.1201910233922092 ) ) ;
#80595 = CARTESIAN_POINT ( 'NONE',  ( 36.80065962568925642, -288.7444315330823770, -251.8809452291229718 ) ) ;
#80596 = CARTESIAN_POINT ( 'NONE',  ( 37.70437488935201031, -283.5645577177655241, -271.3144373270855567 ) ) ;
#80597 = CARTESIAN_POINT ( 'NONE',  ( -99.64851363520514838, -278.1183205137967889, -315.6257852840058149 ) ) ;
#80598 = CARTESIAN_POINT ( 'NONE',  ( -41.94514764665698436, -296.0139505274502767, -195.8583994094566378 ) ) ;
#80599 = CARTESIAN_POINT ( 'NONE',  ( -38.16777731414562425, -279.8753885375685400, -193.3655492722977840 ) ) ;
#80601 = CARTESIAN_POINT ( 'NONE',  ( -94.74842352585828564, -275.0683620204079034, -223.2739041625046070 ) ) ;
#80600 = VECTOR ( 'NONE', #69050, 1000.000000000000000 ) ;
#80602 = CARTESIAN_POINT ( 'NONE',  ( 160.5350683151633291, 249.5000000000000568, 24.72542485937378842 ) ) ;
#80603 = CARTESIAN_POINT ( 'NONE',  ( -95.99890600148557951, -287.6948066931273615, -223.6242672951989618 ) ) ;
#80604 = CARTESIAN_POINT ( 'NONE',  ( -43.93223171177390896, -272.2099253949742774, -194.6081887851420618 ) ) ;
#80605 = DIRECTION ( 'NONE',  ( -0.7453559924999223485, 0.000000000000000000, -0.6666666666666750674 ) ) ;
#80606 = CARTESIAN_POINT ( 'NONE',  ( -76.84986633076367468, -279.0153687307999917, -208.8427506613836044 ) ) ;
#80607 = CIRCLE ( 'NONE', #14141, 0.5000000000000004441 ) ;
#80608 = CARTESIAN_POINT ( 'NONE',  ( 21.43587133717164050, -277.4217040808248953, -319.4855092007605890 ) ) ;
#80609 = CARTESIAN_POINT ( 'NONE',  ( -61.17005598676182387, -282.4127575109083068, -343.3894364868161801 ) ) ;
#80610 = CARTESIAN_POINT ( 'NONE',  ( -15.53194433218923898, -290.5262876513946821, -341.1416826281522390 ) ) ;
#80611 = CARTESIAN_POINT ( 'NONE',  ( -57.22785902341170328, -299.3203508725534903, -196.6364723243882509 ) ) ;
#80612 = EDGE_CURVE ( 'NONE', #25728, #29030, #91243, .T. ) ;
#80613 = CARTESIAN_POINT ( 'NONE',  ( -112.5020922378360240, -297.9440762879806357, -255.4975068239502889 ) ) ;
#80614 = EDGE_CURVE ( 'NONE', #75524, #16725, #64933, .T. ) ;
#80615 = CARTESIAN_POINT ( 'NONE',  ( 24.46114235158401584, -296.1260809147493092, -312.6470023915463230 ) ) ;
#80616 = CARTESIAN_POINT ( 'NONE',  ( 19.37016060382411098, -278.8735348475181013, -221.5173336865785529 ) ) ;
#80617 = TOROIDAL_SURFACE ( 'NONE', #88174, 4.499999999999986677, 0.5000000000000000000 ) ;
#80618 = CARTESIAN_POINT ( 'NONE',  ( -31.17934293839923754, -272.1504588927260215, -195.9581829050052022 ) ) ;
#80619 = CARTESIAN_POINT ( 'NONE',  ( -89.35521443607908054, -286.9348496448824335, -214.6023984822353157 ) ) ;
#80620 = CARTESIAN_POINT ( 'NONE',  ( -68.90346522408979979, -288.3975569416243729, -336.5281872749503123 ) ) ;
#80621 = CARTESIAN_POINT ( 'NONE',  ( 169.5516713374554456, 231.4314716580894071, -192.4310804009363665 ) ) ;
#80622 = VERTEX_POINT ( 'NONE', #28452 ) ;
#80623 = CARTESIAN_POINT ( 'NONE',  ( -3.339366624424855434, -287.1868004975563622, -338.8040455191342062 ) ) ;
#80624 = CARTESIAN_POINT ( 'NONE',  ( 34.30407757348636011, -287.4057453997950233, -284.5314100344209010 ) ) ;
#80625 = ORIENTED_EDGE ( 'NONE', *, *, #52172, .T. ) ;
#80626 = CARTESIAN_POINT ( 'NONE',  ( -4.917186391078216978, -287.5488524038057108, -200.8618847489759105 ) ) ;
#80627 = CARTESIAN_POINT ( 'NONE',  ( -40.50243445195970082, -277.4262370723741356, -343.3262915105309503 ) ) ;
#80628 = CARTESIAN_POINT ( 'NONE',  ( 39.19265033448239421, -292.5436661972052548, -276.0300475646976111 ) ) ;
#80629 = CARTESIAN_POINT ( 'NONE',  ( 25.85130039774165311, -282.7834178363546584, -314.2015992173868995 ) ) ;
#80630 = CARTESIAN_POINT ( 'NONE',  ( 32.93501657957552453, -283.4556118962891560, -300.2264410652383617 ) ) ;
#80631 = CARTESIAN_POINT ( 'NONE',  ( -96.25139210699917669, -284.2178077463306636, -319.9334288332771621 ) ) ;
#80632 = CARTESIAN_POINT ( 'NONE',  ( 33.13287274737167110, -281.6324163675899399, -251.1972740236468837 ) ) ;
#80633 = CARTESIAN_POINT ( 'NONE',  ( -54.49178911615187104, -274.7666405000204577, -345.3538533559490702 ) ) ;
#80634 = CARTESIAN_POINT ( 'NONE',  ( -21.92796979628985099, -108.3679673722940890, -362.8334583402871658 ) ) ;
#80635 = ORIENTED_EDGE ( 'NONE', *, *, #44097, .T. ) ;
#80636 = CARTESIAN_POINT ( 'NONE',  ( -112.1856056875244008, -280.5843480040693407, -267.8720730314923344 ) ) ;
#80637 = CARTESIAN_POINT ( 'NONE',  ( 202.2089753311514926, 295.8238823582390182, -68.59691984642449825 ) ) ;
#80638 = CARTESIAN_POINT ( 'NONE',  ( -40.16685237741654646, -139.4501677287193502, -361.1782757304578126 ) ) ;
#80639 = CIRCLE ( 'NONE', #33744, 0.5000000000000004441 ) ;
#80640 = CARTESIAN_POINT ( 'NONE',  ( -93.68683404902384382, -296.5602610471650564, -223.7678503208838379 ) ) ;
#80641 = CARTESIAN_POINT ( 'NONE',  ( 23.97613257082112881, -293.6794421192739719, -316.8331557748318801 ) ) ;
#80642 = CARTESIAN_POINT ( 'NONE',  ( 46.05136225311299114, 10.74623296475258627, -328.6500756323578685 ) ) ;
#80644 = CARTESIAN_POINT ( 'NONE',  ( -94.73920026989721066, -288.3030305993506204, -316.7504205760400851 ) ) ;
#80643 = CARTESIAN_POINT ( 'NONE',  ( -48.86308555104901075, -296.4830194937312058, -194.7706940381690970 ) ) ;
#80645 = CARTESIAN_POINT ( 'NONE',  ( -45.19829872390753422, -297.0129904678551611, -344.2307342631454503 ) ) ;
#80646 = CARTESIAN_POINT ( 'NONE',  ( -18.32988954735931841, -290.1173250778139163, -341.4055725574542066 ) ) ;
#80647 = ORIENTED_EDGE ( 'NONE', *, *, #25145, .F. ) ;
#80648 = CARTESIAN_POINT ( 'NONE',  ( -11.12626039145826340, -295.6600564492915737, -342.5671606866590650 ) ) ;
#80649 = CARTESIAN_POINT ( 'NONE',  ( -73.59160737361305848, -286.0495101476194577, -206.9121336901716859 ) ) ;
#80650 = CARTESIAN_POINT ( 'NONE',  ( -33.34474327913569169, -296.8960777995857256, -193.7589848913696358 ) ) ;
#80651 = AXIS2_PLACEMENT_3D ( 'NONE', #48797, #75819, #61630 ) ;
#80652 = CARTESIAN_POINT ( 'NONE',  ( 32.03576029928489532, -293.9293210171288138, -237.2083198445805010 ) ) ;
#80653 = CARTESIAN_POINT ( 'NONE',  ( 38.29790953048718904, -294.2215879961315750, -284.5098473702107071 ) ) ;
#80654 = CARTESIAN_POINT ( 'NONE',  ( -66.56602437012034557, -291.8250603831472745, -203.4661340366758395 ) ) ;
#80655 = EDGE_LOOP ( 'NONE', ( #62268, #67488 ) ) ;
#80656 = DIRECTION ( 'NONE',  ( -0.2156506209390900430, 0.000000000000000000, 0.9764705882352960886 ) ) ;
#80657 = CARTESIAN_POINT ( 'NONE',  ( -8.267702724943189807, -276.3498943526248581, -200.5630844522248708 ) ) ;
#80658 = CARTESIAN_POINT ( 'NONE',  ( 33.35305942019162728, -273.9684279267765987, -240.7238860052175085 ) ) ;
#80659 = ORIENTED_EDGE ( 'NONE', *, *, #6263, .T. ) ;
#80660 = CARTESIAN_POINT ( 'NONE',  ( -17.37991209284142968, -276.3088828790554317, -344.6649127813457198 ) ) ;
#80661 = CARTESIAN_POINT ( 'NONE',  ( -72.26854459626602534, -271.9822259945433416, -205.2922156131260181 ) ) ;
#80662 = CARTESIAN_POINT ( 'NONE',  ( 18.34639594754544945, -274.3812704080507388, -319.4689974431610153 ) ) ;
#80663 = CARTESIAN_POINT ( 'NONE',  ( 52.26321846338277766, -300.4034925610951063, -196.9452196686116849 ) ) ;
#80664 = CARTESIAN_POINT ( 'NONE',  ( -32.68801561960830782, -275.0534625816939638, -197.2612632450224623 ) ) ;
#80665 = CARTESIAN_POINT ( 'NONE',  ( -36.92305596632481013, -299.6574319610531916, -194.1610007473992425 ) ) ;
#80666 = CARTESIAN_POINT ( 'NONE',  ( 3.982697788410620277, -272.6254278401342503, -207.2856974345233425 ) ) ;
#80667 = CARTESIAN_POINT ( 'NONE',  ( -38.33536874342558320, -295.7163486224669668, -343.4562976541824924 ) ) ;
#80668 = CARTESIAN_POINT ( 'NONE',  ( -42.44858803093227806, -293.6925451356875101, -343.7729332000806153 ) ) ;
#80669 = DIRECTION ( 'NONE',  ( 0.000000000000000000, 0.000000000000000000, 1.000000000000000000 ) ) ;
#80670 = CARTESIAN_POINT ( 'NONE',  ( 21.68744721306714851, -276.7090908225387125, -319.7077153084395036 ) ) ;
#80671 = CARTESIAN_POINT ( 'NONE',  ( -34.04280338166187647, -274.2614786291991891, -197.4356952222026678 ) ) ;
#80672 = CARTESIAN_POINT ( 'NONE',  ( -66.98244148497897754, -284.3565134170310102, -199.8293894821586605 ) ) ;
#80673 = CARTESIAN_POINT ( 'NONE',  ( -91.36132212530594643, -297.8187481375859988, -322.6287835645019300 ) ) ;
#80674 = PLANE ( 'NONE',  #64181 ) ;
#80675 = AXIS2_PLACEMENT_3D ( 'NONE', #8363, #61827, #32935 ) ;
#80676 = CARTESIAN_POINT ( 'NONE',  ( -71.24398842751128313, -284.7896357092502058, -205.5287450856548048 ) ) ;
#80677 = CARTESIAN_POINT ( 'NONE',  ( -100.3183350266978948, -277.3220132211541227, -231.3800096711332799 ) ) ;
#80678 = CARTESIAN_POINT ( 'NONE',  ( -93.18553236381445970, -276.4500524535504269, -318.2864903817628033 ) ) ;
#80679 = CARTESIAN_POINT ( 'NONE',  ( -28.26766519831462077, -284.9373004810215662, -344.8618117954649733 ) ) ;
#80680 = CARTESIAN_POINT ( 'NONE',  ( 20.15703958886026470, -276.1165621682254141, -224.7227557075171092 ) ) ;
#80681 = CARTESIAN_POINT ( 'NONE',  ( 85.55100297371598117, -296.0521521680024080, -417.1172536214571096 ) ) ;
#80682 = CARTESIAN_POINT ( 'NONE',  ( 10.01279240863232367, -274.8122076995315979, -330.1276643319100117 ) ) ;
#80683 = AXIS2_PLACEMENT_3D ( 'NONE', #55299, #11724, #39183 ) ;
#80684 = CARTESIAN_POINT ( 'NONE',  ( -6.994466967600344809, -282.4495544418196573, -201.5789260721935818 ) ) ;
#80685 = CARTESIAN_POINT ( 'NONE',  ( 165.2494399300530290, -11.64849832608277325, 9.974999999999996092 ) ) ;
#80686 = CARTESIAN_POINT ( 'NONE',  ( -46.35837608101083873, -287.8587413280799296, -195.3410289967331437 ) ) ;
#80687 = CIRCLE ( 'NONE', #53454, 1.999999999999988454 ) ;
#80688 = DIRECTION ( 'NONE',  ( -0.000000000000000000, -0.000000000000000000, -1.000000000000000000 ) ) ;
#80689 = CARTESIAN_POINT ( 'NONE',  ( -105.5727227803703414, -288.9620752939506474, -239.1005386117919898 ) ) ;
#80690 = DIRECTION ( 'NONE',  ( -0.3024135303179478207, -0.9531768234071973378, 0.000000000000000000 ) ) ;
#80691 = CARTESIAN_POINT ( 'NONE',  ( -109.0121239484455060, -271.4501164827466368, -254.0947776090119419 ) ) ;
#80692 = CARTESIAN_POINT ( 'NONE',  ( -103.4998016162079892, -289.1428355648584443, -236.5729113685504785 ) ) ;
#80693 = CARTESIAN_POINT ( 'NONE',  ( 117.8046289747227320, 148.0164379187816053, -257.9426961570557069 ) ) ;
#80694 = DIRECTION ( 'NONE',  ( 0.000000000000000000, 0.000000000000000000, -1.000000000000000000 ) ) ;
#80695 = CARTESIAN_POINT ( 'NONE',  ( 7.511191807944600285, -286.9328762090681835, -332.1589624366116595 ) ) ;
#80696 = CARTESIAN_POINT ( 'NONE',  ( 6.079041424221729883, -284.0519553649695013, -330.0359000625119847 ) ) ;
#80697 = CARTESIAN_POINT ( 'NONE',  ( -113.3125630315945216, -282.8328988306882934, -267.1347769798854870 ) ) ;
#80698 = CARTESIAN_POINT ( 'NONE',  ( -108.3504172742902369, -290.3287437157649720, -287.2951691591007943 ) ) ;
#80699 = VECTOR ( 'NONE', #12331, 1000.000000000000000 ) ;
#80700 = TOROIDAL_SURFACE ( 'NONE', #3579, 25.50000000000000355, 0.5000000000000000000 ) ;
#80701 = CARTESIAN_POINT ( 'NONE',  ( 34.90931797535003511, -282.7937461364803653, -256.3246587310170526 ) ) ;
#80702 = CARTESIAN_POINT ( 'NONE',  ( -2.342442496387988626, -283.3793297680984438, -334.6222583516037048 ) ) ;
#80703 = CARTESIAN_POINT ( 'NONE',  ( -69.90497682248880551, -291.4586717020156357, -338.3314535750560026 ) ) ;
#80704 = CARTESIAN_POINT ( 'NONE',  ( 30.78618628518020373, -299.0497418230892208, -193.3592212852306318 ) ) ;
#80705 = AXIS2_PLACEMENT_3D ( 'NONE', #78969, #64800, #65254 ) ;
#80706 = CARTESIAN_POINT ( 'NONE',  ( 11.46667891486397473, -286.4611437164322183, -328.0417588463044467 ) ) ;
#80707 = CARTESIAN_POINT ( 'NONE',  ( -0.04544512761132132872, -274.5342885334318908, -202.9815245707586087 ) ) ;
#80708 = CARTESIAN_POINT ( 'NONE',  ( -28.68065138822588978, -296.9218163533998336, -344.5539126099598093 ) ) ;
#80709 = DIRECTION ( 'NONE',  ( -1.000000000000000000, 0.000000000000000000, 0.000000000000000000 ) ) ;
#80710 = CARTESIAN_POINT ( 'NONE',  ( 35.78497577281001440, -290.2662352645559167, -287.0191576251351080 ) ) ;
#80711 = CARTESIAN_POINT ( 'NONE',  ( -5.836634923200410441, -281.3139294116411975, -336.7728089953354242 ) ) ;
#80712 = CARTESIAN_POINT ( 'NONE',  ( -98.18123366909019012, -275.9518301094695403, -314.5257324059594453 ) ) ;
#80713 = CARTESIAN_POINT ( 'NONE',  ( -80.83913248881592040, -271.9538145460363694, -207.6019543870419284 ) ) ;
#80714 = CARTESIAN_POINT ( 'NONE',  ( 25.36753299582257526, -274.3835271994092864, -232.6938536957339920 ) ) ;
#80715 = CARTESIAN_POINT ( 'NONE',  ( -32.12736780972890926, -293.6392091423817874, -196.8397491205238339 ) ) ;
#80716 = CIRCLE ( 'NONE', #47447, 6.338655513825452559 ) ;
#80717 = CARTESIAN_POINT ( 'NONE',  ( 32.02002961880699416, -294.1802606469486250, -246.7010149481445467 ) ) ;
#80718 = CARTESIAN_POINT ( 'NONE',  ( -110.4964874198071527, -286.1617758118932215, -281.9298906159953617 ) ) ;
#80719 = CARTESIAN_POINT ( 'NONE',  ( 28.95532888275551997, -294.4799965604088356, -232.3701949094345309 ) ) ;
#80720 = CARTESIAN_POINT ( 'NONE',  ( 19.17675958178251605, -295.5735539856111131, -322.0034272664332207 ) ) ;
#80721 = CARTESIAN_POINT ( 'NONE',  ( -80.15649115309555839, -295.4836010988398698, -329.4872008391952249 ) ) ;
#80722 = CARTESIAN_POINT ( 'NONE',  ( -92.03424078925327478, -291.8327591062536612, -321.7567772052939858 ) ) ;
#80723 = CARTESIAN_POINT ( 'NONE',  ( -95.33333507678375440, -284.0337332961186121, -321.0165252012948258 ) ) ;
#80724 = CARTESIAN_POINT ( 'NONE',  ( -112.6325156277984689, -270.7992862870522686, -261.8995235254844260 ) ) ;
#80725 = CARTESIAN_POINT ( 'NONE',  ( -114.3407554914418540, -284.3902425960415030, -269.9797026784136733 ) ) ;
#80726 = CARTESIAN_POINT ( 'NONE',  ( -68.70609260014886388, -279.4463236246886026, -338.1108478244917706 ) ) ;
#80727 = CARTESIAN_POINT ( 'NONE',  ( -110.3880023331265789, -283.4476732166726833, -262.6933978173333344 ) ) ;
#80728 = CARTESIAN_POINT ( 'NONE',  ( 18.12745533052277835, -286.2565682542181662, -320.8596755229561381 ) ) ;
#80729 = CARTESIAN_POINT ( 'NONE',  ( -111.1923468024427279, -276.9068386878082038, -253.4381315162311807 ) ) ;
#80730 = CARTESIAN_POINT ( 'NONE',  ( 84.09003387609358526, 83.72762891241104910, -302.5758382668069544 ) ) ;
#80731 = CARTESIAN_POINT ( 'NONE',  ( -107.4121885052917946, -284.3354467313042164, -249.4947627439274243 ) ) ;
#80732 = CARTESIAN_POINT ( 'NONE',  ( 27.97450754521559091, -283.2839780505913154, -310.4841881115479509 ) ) ;
#80733 = CARTESIAN_POINT ( 'NONE',  ( -3.176254805997625219, -287.6707424742872945, -339.1182827741045571 ) ) ;
#80734 = CARTESIAN_POINT ( 'NONE',  ( -88.65816948899072258, -279.3583210976050282, -326.6910424108231155 ) ) ;
#80735 = EDGE_CURVE ( 'NONE', #47701, #72158, #79577, .T. ) ;
#80736 = CARTESIAN_POINT ( 'NONE',  ( 12.39679360693573074, -277.6912109917018938, -328.4935573985345059 ) ) ;
#80738 = EDGE_CURVE ( 'NONE', #2276, #24966, #9526, .T. ) ;
#80737 = CARTESIAN_POINT ( 'NONE',  ( -35.66067117326975477, -279.9071115699464372, -197.3680729565291756 ) ) ;
#80739 = CARTESIAN_POINT ( 'NONE',  ( -3.378317565346750762, -276.4826888935253351, -203.8762101897231673 ) ) ;
#80740 = CARTESIAN_POINT ( 'NONE',  ( 37.42194470148324115, -293.3216869639346669, -251.9383762810997780 ) ) ;
#80741 = CARTESIAN_POINT ( 'NONE',  ( 16.36249123482662426, -284.8170321379483312, -218.2469331948977640 ) ) ;
#80742 = CARTESIAN_POINT ( 'NONE',  ( -42.02536033575427155, -293.5941647697928261, -194.3051928809160245 ) ) ;
#80743 = CARTESIAN_POINT ( 'NONE',  ( -69.87355327019915308, -294.4113844697831723, -336.0566627765817884 ) ) ;
#80744 = CARTESIAN_POINT ( 'NONE',  ( 31.55859179288613703, -293.5423356067616396, -294.6959015195108691 ) ) ;
#80745 = CARTESIAN_POINT ( 'NONE',  ( -47.71524630523616395, -293.0030092285787759, -194.3214733833709715 ) ) ;
#80746 = CARTESIAN_POINT ( 'NONE',  ( 34.04174452890308089, -282.4111437847175239, -286.1185447227665009 ) ) ;
#80747 = CARTESIAN_POINT ( 'NONE',  ( -9.237262086084902180, -297.3166033843284026, -193.6752382179209633 ) ) ;
#80748 = CARTESIAN_POINT ( 'NONE',  ( 38.57570410709797670, -288.3609225647131780, -282.9268169659338810 ) ) ;
#80749 = CARTESIAN_POINT ( 'NONE',  ( 18.85121182303647558, -280.3938182899094045, -321.2577442569548225 ) ) ;
#80750 = CARTESIAN_POINT ( 'NONE',  ( 34.02432539428471614, -288.2534716252163207, -299.3585290927771894 ) ) ;
#80751 = CARTESIAN_POINT ( 'NONE',  ( -59.98921508271534009, -286.0836848681150855, -200.9408215765164698 ) ) ;
#80752 = CARTESIAN_POINT ( 'NONE',  ( 169.9462594094670180, 276.0000000000000568, -23.92352941176469727 ) ) ;
#80753 = CIRCLE ( 'NONE', #83781, 4.000000000000003553 ) ;
#80754 = CARTESIAN_POINT ( 'NONE',  ( 137.0887459190394679, 180.1851913858904766, -239.5941216051346032 ) ) ;
#80755 = CARTESIAN_POINT ( 'NONE',  ( 201.7738562182570661, 292.3636489450776708, -53.99999999998410516 ) ) ;
#80756 = CARTESIAN_POINT ( 'NONE',  ( -109.2890452841104292, -277.9240275538465994, -257.0877893752386854 ) ) ;
#80757 = CARTESIAN_POINT ( 'NONE',  ( -110.2128643799814256, -277.3614662463560876, -278.8118533307255689 ) ) ;
#80758 = CARTESIAN_POINT ( 'NONE',  ( -9.132041924864411797, -297.9041281600072466, -193.4249352461565650 ) ) ;
#80759 = CARTESIAN_POINT ( 'NONE',  ( -11.13748388457448790, -93.05548120058779205, -357.1551308049848785 ) ) ;
#80760 = CARTESIAN_POINT ( 'NONE',  ( -107.9611199367248560, -277.5006323421724801, -241.1805793072681752 ) ) ;
#80761 = AXIS2_PLACEMENT_3D ( 'NONE', #51567, #87545, #942 ) ;
#80762 = CARTESIAN_POINT ( 'NONE',  ( 23.23489877041117069, -295.9315662353751009, -316.2353992550123394 ) ) ;
#80763 = CARTESIAN_POINT ( 'NONE',  ( -22.73444753245486183, -292.7365334218281419, -198.7746904067340665 ) ) ;
#80764 = CARTESIAN_POINT ( 'NONE',  ( -101.4206850775283613, -297.9141795850052290, -227.9338231061404088 ) ) ;
#80765 = CARTESIAN_POINT ( 'NONE',  ( -3.151777270829502431, -287.2757789271626052, -335.4735453984766309 ) ) ;
#80766 = CARTESIAN_POINT ( 'NONE',  ( -111.7218282884229126, -273.4505231540948671, -250.6403448215230867 ) ) ;
#80767 = CARTESIAN_POINT ( 'NONE',  ( -109.1417444117289790, -296.5440327891541870, -283.6119185539668024 ) ) ;
#80768 = ORIENTED_EDGE ( 'NONE', *, *, #47322, .F. ) ;
#80769 = DIRECTION ( 'NONE',  ( 0.000000000000000000, -0.000000000000000000, 1.000000000000000000 ) ) ;
#80770 = TOROIDAL_SURFACE ( 'NONE', #12731, 25.50000000000000355, 0.5000000000000000000 ) ;
#80771 = CIRCLE ( 'NONE', #59645, 20.15985230015483154 ) ;
#80772 = CARTESIAN_POINT ( 'NONE',  ( -112.6117965512912633, -280.5638836903187325, -263.1756497733751985 ) ) ;
#80773 = CIRCLE ( 'NONE', #89816, 8.000000000000000000 ) ;
#80774 = CARTESIAN_POINT ( 'NONE',  ( -110.4679533834542724, -279.6998041295244661, -265.1864529924664566 ) ) ;
#80775 = CARTESIAN_POINT ( 'NONE',  ( -86.42334322707458227, -279.4825635086385773, -328.4382755050291962 ) ) ;
#80776 = CARTESIAN_POINT ( 'NONE',  ( -79.23344749411340615, -271.9556465748632945, -209.6708550135730036 ) ) ;
#80777 = LINE ( 'NONE', #64298, #413 ) ;
#80778 = CARTESIAN_POINT ( 'NONE',  ( 129.4467878515196162, -299.5541904835127980, -200.7046326357662167 ) ) ;
#80779 = CARTESIAN_POINT ( 'NONE',  ( -62.31094260811752150, -279.8849374510551229, -201.7108436353591969 ) ) ;
#80780 = CARTESIAN_POINT ( 'NONE',  ( 0.9754012281359498715, -277.3575839374287284, -337.0244654815010676 ) ) ;
#80781 = AXIS2_PLACEMENT_3D ( 'NONE', #4800, #26584, #5293 ) ;
#80782 = CARTESIAN_POINT ( 'NONE',  ( 2.462230916218959287, -278.5192513584873382, -333.9883533326937481 ) ) ;
#80783 = CARTESIAN_POINT ( 'NONE',  ( -109.1889831946827627, -276.7940754479504335, -296.5270434734528635 ) ) ;
#80784 = EDGE_LOOP ( 'NONE', ( #87391, #44079, #52084, #59946, #39161 ) ) ;
#80785 = LINE ( 'NONE', #87864, #76165 ) ;
#80786 = CARTESIAN_POINT ( 'NONE',  ( 34.90903669404877263, -283.8085414261822734, -291.9473257305984930 ) ) ;
#80787 = CARTESIAN_POINT ( 'NONE',  ( -107.5473703500983333, -290.0215945511944824, -249.7310884712448456 ) ) ;
#80788 = CARTESIAN_POINT ( 'NONE',  ( -49.32065485834987584, -285.2520230882961982, -194.3481395924868025 ) ) ;
#80789 = CARTESIAN_POINT ( 'NONE',  ( -107.1367117731449810, -282.4669304159499461, -295.1437363591193161 ) ) ;
#80791 = CARTESIAN_POINT ( 'NONE',  ( 9.964069392794204560, -284.7897193035814212, -212.8852242100739716 ) ) ;
#80790 = CARTESIAN_POINT ( 'NONE',  ( -76.45556027577532632, -282.1608352030651190, -332.7550164340187848 ) ) ;
#80792 = CARTESIAN_POINT ( 'NONE',  ( -34.31221878957652649, -281.2961284327006410, -197.0139798273647784 ) ) ;
#80793 = CARTESIAN_POINT ( 'NONE',  ( 223.4306832106270804, -147.4436952405746979, 22.50000000000000000 ) ) ;
#80794 = CARTESIAN_POINT ( 'NONE',  ( 17.23887642618106852, -280.6894548620743421, -323.6098032450410074 ) ) ;
#80795 = CARTESIAN_POINT ( 'NONE',  ( 30.36909351505336829, -295.1264562740456086, -237.9876190257857900 ) ) ;
#80796 = CARTESIAN_POINT ( 'NONE',  ( -107.2115936112030283, -278.9172058406896895, -292.0268518571219261 ) ) ;
#80797 = CARTESIAN_POINT ( 'NONE',  ( -69.04340306327220844, -287.6364293456096561, -202.1926326118442887 ) ) ;
#80798 = DIRECTION ( 'NONE',  ( 0.000000000000000000, 0.000000000000000000, -1.000000000000000000 ) ) ;
#80799 = CARTESIAN_POINT ( 'NONE',  ( -98.87289171003052957, -293.0641890920890660, -226.5065097648617041 ) ) ;
#80800 = CARTESIAN_POINT ( 'NONE',  ( -23.99812914350882309, -274.8816854556443445, -344.2174294559167151 ) ) ;
#80801 = CARTESIAN_POINT ( 'NONE',  ( -38.92711335558434627, -288.2687405391064885, -347.1832846144802147 ) ) ;
#80802 = CARTESIAN_POINT ( 'NONE',  ( -25.25825090711430221, -290.6084767101443731, -197.5050163048832133 ) ) ;
#80803 = CARTESIAN_POINT ( 'NONE',  ( -104.7302311409926290, -276.8438014001201282, -299.8149630055418697 ) ) ;
#80804 = CARTESIAN_POINT ( 'NONE',  ( -108.7981029369255452, -294.4301856929252494, -290.4819524438684084 ) ) ;
#80805 = CARTESIAN_POINT ( 'NONE',  ( -110.4652262588898992, -291.9637926657075013, -262.9995010671385671 ) ) ;
#80806 = DIRECTION ( 'NONE',  ( 0.000000000000000000, 0.000000000000000000, -1.000000000000000000 ) ) ;
#80807 = CARTESIAN_POINT ( 'NONE',  ( 27.50640061612403997, -292.5639290026003891, -310.6776540298927785 ) ) ;
#80808 = CARTESIAN_POINT ( 'NONE',  ( 7.395881705345527024, -288.2735091921749699, -211.6025337545028719 ) ) ;
#80809 = CARTESIAN_POINT ( 'NONE',  ( -99.85980111615754140, -288.2140498186846003, -313.5521015672636054 ) ) ;
#80810 = CARTESIAN_POINT ( 'NONE',  ( 22.45096607517663756, -289.5722765538042154, -313.2588100689136468 ) ) ;
#80811 = CARTESIAN_POINT ( 'NONE',  ( 140.6539576904058606, 131.0000000000000568, 11.50000000000000000 ) ) ;
#80812 = CARTESIAN_POINT ( 'NONE',  ( -105.2591433654582289, -290.9901215845535489, -297.6967179592811021 ) ) ;
#80813 = CARTESIAN_POINT ( 'NONE',  ( -37.65625321811246096, -297.0359238922718532, -345.7284651688788131 ) ) ;
#80814 = LINE ( 'NONE', #32017, #59505 ) ;
#80815 = CARTESIAN_POINT ( 'NONE',  ( -43.13687005376367978, -290.3288640853958782, -346.7445240610447854 ) ) ;
#80816 = CARTESIAN_POINT ( 'NONE',  ( -110.7927256074832059, -276.7873817904935549, -253.5280058539548520 ) ) ;
#80817 = CARTESIAN_POINT ( 'NONE',  ( -50.94006445514779102, -280.2162147420324914, -194.5928609149019906 ) ) ;
#80818 = CARTESIAN_POINT ( 'NONE',  ( 17.21112458519271016, -280.4710883573537217, -215.9749191443662824 ) ) ;
#80819 = CARTESIAN_POINT ( 'NONE',  ( -92.98848233180861200, -283.2536745904423015, -220.0012799249687134 ) ) ;
#80820 = CARTESIAN_POINT ( 'NONE',  ( 208.2875714627639923, 29.44753873154004964, 14.76836928283343120 ) ) ;
#80821 = CARTESIAN_POINT ( 'NONE',  ( 7.913775325800443738, -278.8170988821121341, -211.4504393562112625 ) ) ;
#80822 = CARTESIAN_POINT ( 'NONE',  ( -5.048672459209301522, -280.6269117234355122, -338.0668893420386780 ) ) ;
#80823 = DIRECTION ( 'NONE',  ( 0.000000000000000000, 0.000000000000000000, 1.000000000000000000 ) ) ;
#80824 = CARTESIAN_POINT ( 'NONE',  ( -111.7215318996356359, -277.2470775444506330, -253.3215058508797597 ) ) ;
#80825 = CARTESIAN_POINT ( 'NONE',  ( -37.16722594807185232, -299.5745066800461132, -196.6648578062816455 ) ) ;
#80826 = CARTESIAN_POINT ( 'NONE',  ( -88.12717539434204639, -282.6634580603832774, -327.8979222978668986 ) ) ;
#80827 = CARTESIAN_POINT ( 'NONE',  ( -71.99321534080206675, -274.3847987021081281, -205.8696271848382366 ) ) ;
#80828 = CARTESIAN_POINT ( 'NONE',  ( 18.92067436663976565, -300.0578547439411636, -193.8419764170976407 ) ) ;
#80829 = CARTESIAN_POINT ( 'NONE',  ( 34.86320200767453059, -275.0741756914497387, -259.3893663229188178 ) ) ;
#80830 = CARTESIAN_POINT ( 'NONE',  ( -73.05510320491455900, -297.5255909549920830, -336.3269203277943689 ) ) ;
#80831 = CARTESIAN_POINT ( 'NONE',  ( -96.38968977502322844, -290.0535359697130389, -319.8015534905158574 ) ) ;
#80832 = CARTESIAN_POINT ( 'NONE',  ( -40.91535955006486347, -278.0873946025727719, -194.8727217248486738 ) ) ;
#80833 = AXIS2_PLACEMENT_3D ( 'NONE', #73392, #23178, #7577 ) ;
#80834 = CARTESIAN_POINT ( 'NONE',  ( -101.6827927269252996, -290.9426087811735329, -227.9662236921970759 ) ) ;
#80835 = EDGE_CURVE ( 'NONE', #75656, #19742, #29385, .T. ) ;
#80836 = CARTESIAN_POINT ( 'NONE',  ( -53.47197783344539346, -288.3229403575269885, -341.7979613374839118 ) ) ;
#80837 = CARTESIAN_POINT ( 'NONE',  ( 35.48614395923007692, -291.3218501149586359, -252.4416933766567865 ) ) ;
#80838 = EDGE_LOOP ( 'NONE', ( #31376, #67607, #83735, #84829 ) ) ;
#80839 = DIRECTION ( 'NONE',  ( 0.000000000000000000, -0.000000000000000000, -1.000000000000000000 ) ) ;
#80840 = CARTESIAN_POINT ( 'NONE',  ( -109.3363081884106265, -290.2275803959498717, -257.6319502625115092 ) ) ;
#80841 = DIRECTION ( 'NONE',  ( 0.000000000000000000, 0.000000000000000000, 1.000000000000000000 ) ) ;
#80842 = CARTESIAN_POINT ( 'NONE',  ( 0.1583475295494594925, -287.4800369293899962, -203.3642793163164129 ) ) ;
#80843 = CARTESIAN_POINT ( 'NONE',  ( 7.399455738971494334, -295.1948066931273615, -214.2051214447836571 ) ) ;
#80844 = CARTESIAN_POINT ( 'NONE',  ( 6.469851476471298213, -293.5318797081282582, -333.4605390768797406 ) ) ;
#80845 = EDGE_CURVE ( 'NONE', #52696, #77270, #85727, .T. ) ;
#80846 = CARTESIAN_POINT ( 'NONE',  ( -63.72613161114504265, -284.7042431466907715, -342.1744875436768325 ) ) ;
#80847 = CARTESIAN_POINT ( 'NONE',  ( -74.71828596398320599, -285.3728699584102060, -207.6555294297379817 ) ) ;
#80848 = CARTESIAN_POINT ( 'NONE',  ( 18.69521969451735899, -277.5388818947328105, -317.9122178225212565 ) ) ;
#80849 = CARTESIAN_POINT ( 'NONE',  ( 34.69761165295190608, -291.8253849117466530, -289.9591906224781042 ) ) ;
#80850 = AXIS2_PLACEMENT_3D ( 'NONE', #84599, #41978, #57614 ) ;
#80851 = CARTESIAN_POINT ( 'NONE',  ( -2.712835635230579800, -273.3157590727560091, -205.6465736392402732 ) ) ;
#80852 = ORIENTED_EDGE ( 'NONE', *, *, #14513, .T. ) ;
#80853 = CARTESIAN_POINT ( 'NONE',  ( 195.3198774247918550, 42.06793861907576826, 13.13082619117232497 ) ) ;
#80854 = CARTESIAN_POINT ( 'NONE',  ( 0.5264022157440970684, -294.2285048531094276, -337.3968205271914940 ) ) ;
#80855 = CARTESIAN_POINT ( 'NONE',  ( 14.11768923642479479, -288.7012147585972457, -216.5011291933842870 ) ) ;
#80856 = CARTESIAN_POINT ( 'NONE',  ( -97.15766721518704685, -296.9859163018715549, -318.3771321035365531 ) ) ;
#80857 = CARTESIAN_POINT ( 'NONE',  ( -5.762117462996388717, -287.1300569388433246, -204.4183943034166475 ) ) ;
#80858 = CARTESIAN_POINT ( 'NONE',  ( -110.3222376340370658, -277.9132005616436345, -246.3878397897619834 ) ) ;
#80859 = CARTESIAN_POINT ( 'NONE',  ( -30.71433344388374920, -292.7851271298282541, -193.6964800947524736 ) ) ;
#80860 = CARTESIAN_POINT ( 'NONE',  ( 38.34512336514053743, -285.6352227209219450, -265.9148848488836165 ) ) ;
#80861 = CARTESIAN_POINT ( 'NONE',  ( 38.05074099482647654, -294.0799276647240390, -285.9085973009398458 ) ) ;
#80862 = CARTESIAN_POINT ( 'NONE',  ( -7.265413793488712635, -292.7911519563569982, -203.8216222888351297 ) ) ;
#80863 = CARTESIAN_POINT ( 'NONE',  ( 121.3887860922853150, -299.5541904835127980, -195.3611179825600175 ) ) ;
#80864 = DIRECTION ( 'NONE',  ( 1.000000000000000000, 0.000000000000000000, -0.000000000000000000 ) ) ;
#80865 = CARTESIAN_POINT ( 'NONE',  ( 113.5000000000000568, -192.7866584945343504, -447.4016117689005796 ) ) ;
#80866 = CARTESIAN_POINT ( 'NONE',  ( 2.363572411682822061, -288.0941586262227361, -205.1982521407357751 ) ) ;
#80867 = CARTESIAN_POINT ( 'NONE',  ( 40.64545035920995986, -285.2666405000203440, -288.1938231032136741 ) ) ;
#80868 = EDGE_LOOP ( 'NONE', ( #66667, #30185, #52012, #76939 ) ) ;
#80869 = CARTESIAN_POINT ( 'NONE',  ( -8.384742108316707743, -281.5842092396390512, -337.7088770877577986 ) ) ;
#80870 = CARTESIAN_POINT ( 'NONE',  ( -95.19770440732621353, -277.5315372047091955, -321.1393324097162463 ) ) ;
#80871 = CARTESIAN_POINT ( 'NONE',  ( -1.099953963021016445, -282.5344932052304330, -204.8892594259328916 ) ) ;
#80872 = CARTESIAN_POINT ( 'NONE',  ( -68.86288425581687989, -197.2185115433246381, -359.2771530895120122 ) ) ;
#80873 = CARTESIAN_POINT ( 'NONE',  ( -100.4991487550860825, -283.6995131681854900, -227.2590439676938843 ) ) ;
#80874 = AXIS2_PLACEMENT_3D ( 'NONE', #43400, #88697, #72295 ) ;
#80875 = CARTESIAN_POINT ( 'NONE',  ( 24.91962922687913462, -285.0125148525706322, -229.0925754941216326 ) ) ;
#80876 = CARTESIAN_POINT ( 'NONE',  ( 6.500614332665397122, -276.5009111174006193, -208.5055103792745683 ) ) ;
#80877 = CARTESIAN_POINT ( 'NONE',  ( -52.65410000597154294, -298.3431302024771981, -198.8702710869863495 ) ) ;
#80878 = CARTESIAN_POINT ( 'NONE',  ( -5.341822208537517547, -293.3068515727523504, -336.5358187631491091 ) ) ;
#80879 = CARTESIAN_POINT ( 'NONE',  ( -113.9431494924813393, -279.2953472221363995, -263.0319032181764101 ) ) ;
#80880 = CARTESIAN_POINT ( 'NONE',  ( -41.85658474486650960, -277.1105909851053184, -343.2339629271970125 ) ) ;
#80881 = CARTESIAN_POINT ( 'NONE',  ( -113.8735839098065412, -273.7033722426746181, -264.6629600359769370 ) ) ;
#80882 = CARTESIAN_POINT ( 'NONE',  ( -112.8784203360696381, -270.8800938378385581, -296.3057481714963046 ) ) ;
#80883 = CARTESIAN_POINT ( 'NONE',  ( -3.189148384620934085, -274.6009566780471687, -337.1479835168137811 ) ) ;
#80884 = CARTESIAN_POINT ( 'NONE',  ( -88.19961510018092099, -297.1727374243644704, -327.4590559622506589 ) ) ;
#80885 = DIRECTION ( 'NONE',  ( -0.000000000000000000, -1.000000000000000000, -0.000000000000000000 ) ) ;
#80886 = CARTESIAN_POINT ( 'NONE',  ( 212.4629471475955427, 32.98517505407394168, 10.00000000000000000 ) ) ;
#80887 = CARTESIAN_POINT ( 'NONE',  ( -71.54095004379935574, -284.5948383734786944, -335.2042932558952089 ) ) ;
#80888 = CARTESIAN_POINT ( 'NONE',  ( -110.5095964938329161, -286.0519219365333470, -290.8655798501631580 ) ) ;
#80889 = CARTESIAN_POINT ( 'NONE',  ( -73.59899006222124740, -284.9059343601233536, -206.8698225293622386 ) ) ;
#80890 = CARTESIAN_POINT ( 'NONE',  ( -87.65566418352666744, -276.1689209581305136, -324.3513526064785992 ) ) ;
#80891 = CARTESIAN_POINT ( 'NONE',  ( -87.75050315396148903, -285.6253470096708043, -324.9274606503319092 ) ) ;
#80892 = CARTESIAN_POINT ( 'NONE',  ( -66.32472241315528549, -278.1455566757566089, -202.5927044084809268 ) ) ;
#80893 = CARTESIAN_POINT ( 'NONE',  ( 3.316921798269993005, -277.5710095182063242, -331.3619584366844606 ) ) ;
#80894 = DIRECTION ( 'NONE',  ( 0.000000000000000000, 0.000000000000000000, -1.000000000000000000 ) ) ;
#80895 = CARTESIAN_POINT ( 'NONE',  ( -104.4387055546949625, -273.4342340904827893, -241.3195581572348942 ) ) ;
#80896 = SHAPE_REPRESENTATION ( 'Pneumatic Power Actuating Cylinder', ( #18940 ), #37050 ) ;
#80897 = CARTESIAN_POINT ( 'NONE',  ( 30.57429261198475601, -281.8886383253222903, -234.3091980900835836 ) ) ;
#80898 = CARTESIAN_POINT ( 'NONE',  ( 29.71134787749449657, -282.5356082247352560, -308.1978949779359027 ) ) ;
#80899 = VERTEX_POINT ( 'NONE', #13782 ) ;
#80900 = ORIENTED_EDGE ( 'NONE', *, *, #54874, .T. ) ;
#80901 = DIRECTION ( 'NONE',  ( 0.000000000000000000, 0.000000000000000000, 1.000000000000000000 ) ) ;
#80902 = CARTESIAN_POINT ( 'NONE',  ( 34.77934137657171476, -289.7092353481821192, -293.5744945686486744 ) ) ;
#80903 = AXIS2_PLACEMENT_3D ( 'NONE', #91285, #41569, #63400 ) ;
#80904 = CARTESIAN_POINT ( 'NONE',  ( -97.00852005224960806, -296.3392132321985173, -228.0235185306095218 ) ) ;
#80905 = CARTESIAN_POINT ( 'NONE',  ( -30.69779667728393591, -291.4825108423753477, -193.6979123986693594 ) ) ;
#80906 = CARTESIAN_POINT ( 'NONE',  ( 26.28499433688804032, -286.5387682590465488, -307.6419447866070982 ) ) ;
#80908 = CARTESIAN_POINT ( 'NONE',  ( -38.89670468638797018, -290.2722369875604045, -196.3641182001636309 ) ) ;
#80907 = CARTESIAN_POINT ( 'NONE',  ( 34.85876485693646742, -286.3139308670872083, -284.6552950761611669 ) ) ;
#80909 = CARTESIAN_POINT ( 'NONE',  ( -72.57804954362150340, -286.7797417549978150, -205.9610309928523009 ) ) ;
#80910 = CARTESIAN_POINT ( 'NONE',  ( -112.2362121774151262, -276.5009297386895355, -274.3376379402653242 ) ) ;
#80911 = CARTESIAN_POINT ( 'NONE',  ( 38.80381423493700765, -286.0030799819184040, -274.4010520032072691 ) ) ;
#80912 = CARTESIAN_POINT ( 'NONE',  ( -57.25021422476851995, -287.7955695978098447, -197.9977824795448953 ) ) ;
#80913 = CARTESIAN_POINT ( 'NONE',  ( -103.5533819354939311, -288.0807596484780220, -305.9425965351536547 ) ) ;
#80914 = CARTESIAN_POINT ( 'NONE',  ( 29.53420116598874401, -282.8955484070024227, -300.3356754801890247 ) ) ;
#80915 = CARTESIAN_POINT ( 'NONE',  ( -98.55325287289387859, -293.1441825852793954, -226.7357327266190907 ) ) ;
#80916 = CARTESIAN_POINT ( 'NONE',  ( 82.16069579344274132, -298.6247067295462330, -193.5820051170746297 ) ) ;
#80917 = CARTESIAN_POINT ( 'NONE',  ( 195.7510731661265595, -143.7221692137691775, -21.50000000000000000 ) ) ;
#80918 = CARTESIAN_POINT ( 'NONE',  ( -103.9951007501086053, -298.9422436401694654, -234.6601946772061353 ) ) ;
#80919 = EDGE_CURVE ( 'NONE', #8050, #45887, #42870, .T. ) ;
#80920 = VECTOR ( 'NONE', #8898, 1000.000000000000000 ) ;
#80921 = CARTESIAN_POINT ( 'NONE',  ( 18.09355462092307221, -280.0706692306564491, -222.5974153240782982 ) ) ;
#80922 = CARTESIAN_POINT ( 'NONE',  ( 18.57034904698929623, -278.8559449401706729, -220.3726852480296259 ) ) ;
#80923 = CARTESIAN_POINT ( 'NONE',  ( -16.56039960223472463, -293.9875738063915946, -344.3912037942455413 ) ) ;
#80924 = CARTESIAN_POINT ( 'NONE',  ( -37.80733690747151599, -296.4460944566480407, -196.5625841215439209 ) ) ;
#80925 = CARTESIAN_POINT ( 'NONE',  ( 34.62828102998530966, -273.8782533770864802, -289.3778477870255870 ) ) ;
#80926 = CARTESIAN_POINT ( 'NONE',  ( -107.3338236263226833, -297.5701405377287188, -292.9388246761129153 ) ) ;
#80927 = CARTESIAN_POINT ( 'NONE',  ( 154.3961680540041073, 19.39715479370783768, 12.47437324411263937 ) ) ;
#80928 = CARTESIAN_POINT ( 'NONE',  ( -105.0648837072402557, -294.3410257966332892, -304.9378594723468154 ) ) ;
#80929 = CARTESIAN_POINT ( 'NONE',  ( 4.163563080981257158, -295.9057333466056434, -331.1286096365158187 ) ) ;
#80930 = DIRECTION ( 'NONE',  ( 0.9998346970812742596, 0.000000000000000000, 0.01818181818181330636 ) ) ;
#80931 = CARTESIAN_POINT ( 'NONE',  ( -50.49021521649092392, -296.0272074197996517, -342.3313776559213011 ) ) ;
#80932 = DIRECTION ( 'NONE',  ( 0.000000000000000000, 1.000000000000000000, 7.202301750926674102E-15 ) ) ;
#80934 = CARTESIAN_POINT ( 'NONE',  ( -81.94411708228696511, -297.4251187390993891, -212.5075690501982990 ) ) ;
#80933 = CARTESIAN_POINT ( 'NONE',  ( -105.1870544760080008, -283.0022208108266568, -237.5676019597713093 ) ) ;
#80935 = CARTESIAN_POINT ( 'NONE',  ( -113.1369744685507897, -284.3788108970562689, -284.2213454163775168 ) ) ;
#80936 = CARTESIAN_POINT ( 'NONE',  ( 37.44947268265346452, -283.6093297445146959, -281.1126140492563650 ) ) ;
#80937 = CARTESIAN_POINT ( 'NONE',  ( -46.49877174559616577, -285.6056692503037198, -193.9288451466239280 ) ) ;
#80938 = CARTESIAN_POINT ( 'NONE',  ( -60.81034762864257459, -289.7468991514519416, -199.2486713137323306 ) ) ;
#80939 = CARTESIAN_POINT ( 'NONE',  ( 31.98288692825982693, -272.6237833571632905, -237.0123917617630980 ) ) ;
#80940 = CARTESIAN_POINT ( 'NONE',  ( -48.18343439339133027, -281.1256972089279884, -502.6442049077165279 ) ) ;
#80941 = CARTESIAN_POINT ( 'NONE',  ( 31.44203322619777552, -285.8921673213552026, -244.3322107758392860 ) ) ;
#80942 = CARTESIAN_POINT ( 'NONE',  ( -99.62728815232638624, -288.8768046418859399, -315.1273152812001968 ) ) ;
#80943 = DIRECTION ( 'NONE',  ( 0.000000000000000000, 0.000000000000000000, 1.000000000000000000 ) ) ;
#80944 = CARTESIAN_POINT ( 'NONE',  ( -108.2334561269400126, -298.4206595650496752, -249.8477236400458992 ) ) ;
#80945 = CARTESIAN_POINT ( 'NONE',  ( -105.6569804930849727, -280.4224371361070780, -236.0141575381979635 ) ) ;
#80947 = CARTESIAN_POINT ( 'NONE',  ( 28.16816198786099434, -281.6572348123985989, -302.7333412904417855 ) ) ;
#80946 = CARTESIAN_POINT ( 'NONE',  ( 12.29307649831085847, -292.3858026675229667, -327.1294502709004064 ) ) ;
#80948 = CARTESIAN_POINT ( 'NONE',  ( -19.28522074316199664, -294.9928501384467268, -345.2689501496894309 ) ) ;
#80949 = CARTESIAN_POINT ( 'NONE',  ( -40.72701110398927682, -284.0898680019321887, -194.8257700697250812 ) ) ;
#80950 = CARTESIAN_POINT ( 'NONE',  ( -61.43002905117817392, -281.7395822208497407, -199.2799141292963441 ) ) ;
#80951 = EDGE_CURVE ( 'NONE', #14431, #17995, #87515, .T. ) ;
#80952 = CARTESIAN_POINT ( 'NONE',  ( -23.48602998284878041, -293.9295517078970761, -342.3255346346486476 ) ) ;
#80953 = CARTESIAN_POINT ( 'NONE',  ( -43.10984599156205377, -295.9792986177575358, -195.5314249023259947 ) ) ;
#80954 = ORIENTED_EDGE ( 'NONE', *, *, #80410, .T. ) ;
#80955 = CARTESIAN_POINT ( 'NONE',  ( 158.6539576904058606, 276.0000000000000568, -11.60392986742922439 ) ) ;
#80956 = CARTESIAN_POINT ( 'NONE',  ( 10.30754250284056361, -282.6928055696701563, -212.8359783770726779 ) ) ;
#80957 = CARTESIAN_POINT ( 'NONE',  ( -75.69569416502747572, -295.0863798966923923, -332.6049855037002771 ) ) ;
#80958 = CARTESIAN_POINT ( 'NONE',  ( 215.7837434059060229, -142.7221692137691775, 8.778910157967997563 ) ) ;
#80959 = CARTESIAN_POINT ( 'NONE',  ( -92.05005921254146983, -294.6952119285919025, -226.6919474004047572 ) ) ;
#80960 = CARTESIAN_POINT ( 'NONE',  ( -70.05371433758904232, -272.8293408454781002, -200.8191658664519252 ) ) ;
#80961 = CARTESIAN_POINT ( 'NONE',  ( -91.67173919388861236, -291.0834466493888044, -221.5854032711879427 ) ) ;
#80962 = CARTESIAN_POINT ( 'NONE',  ( -27.48462164438750222, -281.6996346729844731, -197.2783136474464243 ) ) ;
#80963 = CARTESIAN_POINT ( 'NONE',  ( -81.56652468207778384, -275.0394463142596919, -211.2156354820562001 ) ) ;
#80964 = CARTESIAN_POINT ( 'NONE',  ( -44.32538618581968137, -284.7390759999619263, -346.2932228828734083 ) ) ;
#80965 = CARTESIAN_POINT ( 'NONE',  ( -91.57995490408625017, -278.0523690607897151, -220.9107163250839108 ) ) ;
#80966 = CARTESIAN_POINT ( 'NONE',  ( -59.76945595974496683, -279.3428711020333139, -341.9292422769228210 ) ) ;
#80967 = ORIENTED_EDGE ( 'NONE', *, *, #77089, .T. ) ;
#80968 = CARTESIAN_POINT ( 'NONE',  ( -0.04358587629538659969, -274.3676354107399789, -202.9825537491880425 ) ) ;
#80969 = CARTESIAN_POINT ( 'NONE',  ( -34.83276561095786406, -294.0040718146144627, -195.9634066742511322 ) ) ;
#80970 = DIRECTION ( 'NONE',  ( 0.000000000000000000, 0.000000000000000000, 1.000000000000000000 ) ) ;
#80971 = EDGE_CURVE ( 'NONE', #26249, #27568, #89686, .T. ) ;
#80972 = CARTESIAN_POINT ( 'NONE',  ( 29.33919985515026596, -232.1443419142230766, 25.50000000000000000 ) ) ;
#80973 = CARTESIAN_POINT ( 'NONE',  ( -0.08783136817415880537, -292.7016166352680102, -336.3491882483041309 ) ) ;
#80974 = CARTESIAN_POINT ( 'NONE',  ( 94.46225245802311576, -299.4135974027564089, -197.3478171873541669 ) ) ;
#80975 = DIRECTION ( 'NONE',  ( -0.000000000000000000, -1.000000000000000000, -0.000000000000000000 ) ) ;
#80976 = EDGE_CURVE ( 'NONE', #42078, #33611, #14721, .T. ) ;
#80977 = CARTESIAN_POINT ( 'NONE',  ( -68.06750732326811715, -293.1761310821050870, -200.4996701153740162 ) ) ;
#80978 = CARTESIAN_POINT ( 'NONE',  ( -85.33152481854864391, -275.9090924074130839, -210.2361428286349110 ) ) ;
#80979 = CARTESIAN_POINT ( 'NONE',  ( 37.38166234488451778, -289.4890081780330888, -265.4414161113364798 ) ) ;
#80980 = CARTESIAN_POINT ( 'NONE',  ( 10.82511592784155141, -274.3840315779106618, -327.6322822322093202 ) ) ;
#80981 = CARTESIAN_POINT ( 'NONE',  ( 37.02415473366912835, -277.4163000128716590, -266.0313103988966077 ) ) ;
#80982 = CARTESIAN_POINT ( 'NONE',  ( 37.06137684319755721, -291.6016631164964679, -268.0166922013801241 ) ) ;
#80983 = CARTESIAN_POINT ( 'NONE',  ( -53.52019912407880042, -281.7073012417760651, -196.2901147211961472 ) ) ;
#80984 = VECTOR ( 'NONE', #48145, 1000.000000000000000 ) ;
#80985 = EDGE_LOOP ( 'NONE', ( #63642, #88302 ) ) ;
#80986 = CARTESIAN_POINT ( 'NONE',  ( -93.44103837372750831, -283.5558013726102899, -317.1045852829162186 ) ) ;
#80987 = CARTESIAN_POINT ( 'NONE',  ( -82.35370408541332665, -278.7304551895524583, -332.4530821058404513 ) ) ;
#80988 = CARTESIAN_POINT ( 'NONE',  ( -33.09617432451796759, -281.7947545888164314, -346.8593749361108394 ) ) ;
#80989 = CARTESIAN_POINT ( 'NONE',  ( -84.71173679581764304, -278.6278634440695896, -330.8347775141432976 ) ) ;
#80990 = CARTESIAN_POINT ( 'NONE',  ( 36.92162573082385535, -277.2942806637337299, -287.9578773858711429 ) ) ;
#80991 = CARTESIAN_POINT ( 'NONE',  ( -6.998514795304313196, -288.9805209788416391, -207.2794874003663779 ) ) ;
#80992 = ORIENTED_EDGE ( 'NONE', *, *, #48158, .T. ) ;
#80993 = CARTESIAN_POINT ( 'NONE',  ( -105.7506846275603181, -298.1477255294961992, -301.2322638647054873 ) ) ;
#80994 = CARTESIAN_POINT ( 'NONE',  ( -104.9936166230227030, -292.0105962207279049, -241.9899019872270856 ) ) ;
#80995 = CARTESIAN_POINT ( 'NONE',  ( -111.9245850319576192, -276.5330386405051968, -273.4008678493808020 ) ) ;
#80996 = CARTESIAN_POINT ( 'NONE',  ( -107.8497421667622405, -291.9479468211941366, -298.6911377430700441 ) ) ;
#80997 = CARTESIAN_POINT ( 'NONE',  ( -9.681227136689926738, -291.7717535669419817, -202.6404911404750919 ) ) ;
#80998 = CARTESIAN_POINT ( 'NONE',  ( 37.08329244450528961, -287.3041584072681189, -289.8661784538941220 ) ) ;
#80999 = CARTESIAN_POINT ( 'NONE',  ( -110.7884892328630571, -283.0526842193842754, -262.6463874164611525 ) ) ;
#81000 = CARTESIAN_POINT ( 'NONE',  ( -87.54761236490108445, -291.6217818917674549, -325.1138439125219293 ) ) ;
#81001 = CARTESIAN_POINT ( 'NONE',  ( -73.88276017995251266, -284.0373658272128523, -206.3507153379153181 ) ) ;
#81002 = CARTESIAN_POINT ( 'NONE',  ( 31.52659216117618257, -282.5256495625073399, -244.5558649205003405 ) ) ;
#81003 = CARTESIAN_POINT ( 'NONE',  ( -71.79010550537037716, -290.4375569107573938, -338.9623394065972093 ) ) ;
#81004 = CARTESIAN_POINT ( 'NONE',  ( -109.1025422709250989, -278.8627298746004044, -284.1519865446053927 ) ) ;
#81005 = CARTESIAN_POINT ( 'NONE',  ( -39.18666668507475492, -290.8244439326350061, -193.7674419063706353 ) ) ;
#81006 = CARTESIAN_POINT ( 'NONE',  ( -15.46923084645170832, -287.1309415353467216, -196.6461273896154580 ) ) ;
#81007 = CARTESIAN_POINT ( 'NONE',  ( 33.98763866029031533, -288.4125120336144050, -299.3414366975588905 ) ) ;
#81008 = CARTESIAN_POINT ( 'NONE',  ( -104.5983809761635115, -285.1013236576974919, -241.8491640071268023 ) ) ;
#81009 = ORIENTED_EDGE ( 'NONE', *, *, #66611, .F. ) ;
#81010 = DIRECTION ( 'NONE',  ( 0.000000000000000000, 1.000000000000000000, 0.000000000000000000 ) ) ;
#81011 = CARTESIAN_POINT ( 'NONE',  ( -36.41762190707066082, -293.9240318489935362, -194.5891269432724471 ) ) ;
#81012 = CARTESIAN_POINT ( 'NONE',  ( -111.8295423015167671, -295.0164994129381171, -287.8780650214542902 ) ) ;
#81013 = CARTESIAN_POINT ( 'NONE',  ( -43.23794448056239048, -276.1871791569755601, -343.3586710289284269 ) ) ;
#81014 = CARTESIAN_POINT ( 'NONE',  ( -48.94640524150316452, -297.2567539731875286, -194.2901330421438217 ) ) ;
#81015 = CARTESIAN_POINT ( 'NONE',  ( 21.06094800268414957, -292.6588410975414263, -315.3243851279051455 ) ) ;
#81016 = CARTESIAN_POINT ( 'NONE',  ( -67.20797283515103970, -295.8949788273944819, -202.6273880238698837 ) ) ;
#81017 = CARTESIAN_POINT ( 'NONE',  ( -69.20378073829436971, -292.8285407349191587, -204.2266040007081074 ) ) ;
#81018 = CARTESIAN_POINT ( 'NONE',  ( 17.32019187608983657, -295.3278275698817765, -319.2298553253233422 ) ) ;
#81019 = CARTESIAN_POINT ( 'NONE',  ( 209.4803090767392462, 35.69423656899339647, 14.26380412667042030 ) ) ;
#81020 = CARTESIAN_POINT ( 'NONE',  ( 34.60722761199123454, -291.8337937111373890, -292.2945376055183715 ) ) ;
#81021 = CARTESIAN_POINT ( 'NONE',  ( -46.76279720659812966, -299.9328330479887086, -195.9035009737389998 ) ) ;
#81022 = CARTESIAN_POINT ( 'NONE',  ( -95.94943698683739797, -290.8786930168090521, -314.2972058669748776 ) ) ;
#81023 = CARTESIAN_POINT ( 'NONE',  ( -34.29606572000218279, -295.3460898357508881, -343.3187193540831572 ) ) ;
#81024 = CARTESIAN_POINT ( 'NONE',  ( -15.05164067315313048, -278.7449016956053924, -342.3988109580352557 ) ) ;
#81025 = CARTESIAN_POINT ( 'NONE',  ( -112.7475847567949927, -277.3997644745304001, -257.4285684779155190 ) ) ;
#81026 = CARTESIAN_POINT ( 'NONE',  ( -92.09066196691415485, -272.6434640186287766, -216.3623775894970152 ) ) ;
#81027 = CARTESIAN_POINT ( 'NONE',  ( 24.89974019181063625, -279.0757743414590095, -229.4353190999128174 ) ) ;
#81028 = CARTESIAN_POINT ( 'NONE',  ( -112.2826064898294192, -276.7767850834315482, -284.2278717966325416 ) ) ;
#81029 = EDGE_CURVE ( 'NONE', #63422, #4490, #65559, .T. ) ;
#81030 = CARTESIAN_POINT ( 'NONE',  ( 95.54697187129778513, -298.4345910877814845, -196.8985534675756810 ) ) ;
#81031 = DIRECTION ( 'NONE',  ( 0.000000000000000000, 0.000000000000000000, -1.000000000000000000 ) ) ;
#81032 = CARTESIAN_POINT ( 'NONE',  ( 17.35631459575653324, -275.5108287996426952, -221.7884948099801647 ) ) ;
#81033 = DIRECTION ( 'NONE',  ( -0.000000000000000000, -0.000000000000000000, 1.000000000000000000 ) ) ;
#81034 = CARTESIAN_POINT ( 'NONE',  ( -108.3248792541964036, -288.2442567293040838, -295.8101322244813787 ) ) ;
#81035 = CARTESIAN_POINT ( 'NONE',  ( -65.44702332552137136, -289.4094629418118529, -342.1049131632886429 ) ) ;
#81036 = CARTESIAN_POINT ( 'NONE',  ( 30.87819878916672067, -277.1372324003118024, -238.6766222048762813 ) ) ;
#81037 = CARTESIAN_POINT ( 'NONE',  ( -39.18867085314754917, -296.0287923967409256, -195.5378555190710586 ) ) ;
#81038 = CARTESIAN_POINT ( 'NONE',  ( -30.24001523134090874, -282.1616333731604982, -346.8707571922872148 ) ) ;
#81039 = CYLINDRICAL_SURFACE ( 'NONE', #89448, 2.000000000000007105 ) ;
#81040 = CARTESIAN_POINT ( 'NONE',  ( -7.028099366246645552, -280.6542849723426798, -338.9757737723930973 ) ) ;
#81041 = AXIS2_PLACEMENT_3D ( 'NONE', #22181, #52443, #30676 ) ;
#81042 = CARTESIAN_POINT ( 'NONE',  ( 200.4025527154073245, 25.63806215016873580, 10.01693176487371240 ) ) ;
#81043 = CARTESIAN_POINT ( 'NONE',  ( -2.236089605140999304, -291.3226378346382148, -205.8896753515070372 ) ) ;
#81044 = CARTESIAN_POINT ( 'NONE',  ( -14.15813556143607244, -284.4954930384076306, -199.7849451296545737 ) ) ;
#81045 = CARTESIAN_POINT ( 'NONE',  ( 201.0592549708491958, 40.73798607845792219, 10.49999999999999822 ) ) ;
#81046 = DIRECTION ( 'NONE',  ( 0.000000000000000000, 0.000000000000000000, -1.000000000000000000 ) ) ;
#81047 = CARTESIAN_POINT ( 'NONE',  ( 37.28808806273238474, -291.4499572040390944, -262.4146482955856641 ) ) ;
#81048 = CARTESIAN_POINT ( 'NONE',  ( -76.76615179585407134, -279.1892942604593486, -332.8083330218639730 ) ) ;
#81049 = CARTESIAN_POINT ( 'NONE',  ( -83.63099041918093235, -284.8761227367322135, -331.4630610348853565 ) ) ;
#81051 = CARTESIAN_POINT ( 'NONE',  ( -109.1930275799229548, -284.7232403703180239, -257.3916972783390520 ) ) ;
#81050 = CARTESIAN_POINT ( 'NONE',  ( 8.653505572859097938, -272.7568014588411529, -210.4131801722226669 ) ) ;
#81052 = CARTESIAN_POINT ( 'NONE',  ( -18.85150736666681581, -278.2346606510798210, -341.5895370801849253 ) ) ;
#81053 = CARTESIAN_POINT ( 'NONE',  ( -9.918369515986093177, -277.4874940834125141, -338.2021623163374215 ) ) ;
#81054 = CARTESIAN_POINT ( 'NONE',  ( -112.3409153512424297, -286.5567344017749747, -270.0170808755260623 ) ) ;
#81055 = ADVANCED_FACE ( 'NONE', ( #49283 ), #80028, .T. ) ;
#81056 = ORIENTED_EDGE ( 'NONE', *, *, #27503, .T. ) ;
#81057 = CARTESIAN_POINT ( 'NONE',  ( 76.08708295871279859, -296.0521521680024080, -465.6442049081569508 ) ) ;
#81058 = CARTESIAN_POINT ( 'NONE',  ( -113.3892119865381574, -296.5375164170397966, -258.2038337485387842 ) ) ;
#81059 = CARTESIAN_POINT ( 'NONE',  ( -6.356235243700066206, -288.4410580755821911, -202.4372341950638088 ) ) ;
#81060 = DIRECTION ( 'NONE',  ( -0.000000000000000000, -1.000000000000000000, -0.000000000000000000 ) ) ;
#81061 = CARTESIAN_POINT ( 'NONE',  ( -99.90806341382575795, -293.4094976428775681, -320.2154176792147382 ) ) ;
#81062 = CARTESIAN_POINT ( 'NONE',  ( -110.2515050878268426, -277.7748034725568118, -246.4092066451927394 ) ) ;
#81063 = CARTESIAN_POINT ( 'NONE',  ( -67.98812607131755215, -290.0563851197890699, -200.5813163142338738 ) ) ;
#81064 = CARTESIAN_POINT ( 'NONE',  ( -71.51678181549092983, -287.1122146640895494, -205.0712141259976136 ) ) ;
#81065 = CARTESIAN_POINT ( 'NONE',  ( -93.87857215656791254, -280.9819653218258395, -222.5759777706735463 ) ) ;
#81066 = CARTESIAN_POINT ( 'NONE',  ( 38.50798064533656628, -289.0992827698227643, -280.0304756630850420 ) ) ;
#81067 = CARTESIAN_POINT ( 'NONE',  ( 35.89886190683343870, -283.7596727216234740, -286.5110630639703686 ) ) ;
#81068 = CARTESIAN_POINT ( 'NONE',  ( 23.51935042613633442, -276.3488882282474606, -317.5516931681427195 ) ) ;
#81069 = CARTESIAN_POINT ( 'NONE',  ( -66.18552049367583834, -295.6928304350341818, -201.5143255293843367 ) ) ;
#81070 = CARTESIAN_POINT ( 'NONE',  ( -94.96038012907692405, -279.0775225141174474, -219.2818881581052892 ) ) ;
#81071 = CARTESIAN_POINT ( 'NONE',  ( -110.1933854105593014, -298.6709517194341856, -255.0044317975683157 ) ) ;
#81072 = FACE_OUTER_BOUND ( 'NONE', #27431, .T. ) ;
#81073 = EDGE_CURVE ( 'NONE', #82490, #89945, #42157, .T. ) ;
#81074 = CARTESIAN_POINT ( 'NONE',  ( -20.25526795762937127, -276.7662352645559167, -195.3538533559490702 ) ) ;
#81075 = CARTESIAN_POINT ( 'NONE',  ( 17.37568445726946820, -273.0598127527824772, -217.5600284599838403 ) ) ;
#81076 = CYLINDRICAL_SURFACE ( 'NONE', #7694, 204.9779373800640485 ) ;
#81077 = CARTESIAN_POINT ( 'NONE',  ( -93.98426742187328387, -278.7124853701401435, -224.2134418521454791 ) ) ;
#81078 = CARTESIAN_POINT ( 'NONE',  ( 22.43879563562683899, -276.1120401272316940, -222.4414599991953594 ) ) ;
#81079 = CARTESIAN_POINT ( 'NONE',  ( -5.563894817473393317, -281.7030332560919419, -340.2395216810197098 ) ) ;
#81080 = CARTESIAN_POINT ( 'NONE',  ( -39.97180380360236285, -290.8456640728059028, -344.3779728523724089 ) ) ;
#81081 = CARTESIAN_POINT ( 'NONE',  ( -75.45058760562159250, -299.0740573700583695, -204.1913127847192868 ) ) ;
#81082 = CARTESIAN_POINT ( 'NONE',  ( -57.30112750002992783, -299.0053553423152835, -196.3491747455985035 ) ) ;
#81083 = CARTESIAN_POINT ( 'NONE',  ( -63.46397673707561182, -293.7111094890969412, -200.2351235796422202 ) ) ;
#81084 = CARTESIAN_POINT ( 'NONE',  ( 36.28474852576971443, -279.7251665690557161, -283.8183955616313483 ) ) ;
#81085 = CARTESIAN_POINT ( 'NONE',  ( 36.95562760380333600, -283.4127182693125633, -265.7544611261768068 ) ) ;
#81086 = CARTESIAN_POINT ( 'NONE',  ( -100.6627215264306727, -271.1058108246733127, -230.8352397431230543 ) ) ;
#81087 = CARTESIAN_POINT ( 'NONE',  ( -83.38344493765916354, -285.2711118183223675, -331.1447497554304391 ) ) ;
#81088 = CARTESIAN_POINT ( 'NONE',  ( 21.41301934707465904, -287.0852999203791001, -314.2239903163523422 ) ) ;
#81089 = CARTESIAN_POINT ( 'NONE',  ( 46.50794016136936193, 11.67038243352686422, -331.8346843585704846 ) ) ;
#81090 = EDGE_LOOP ( 'NONE', ( #29421, #80427, #54892, #20239 ) ) ;
#81091 = CARTESIAN_POINT ( 'NONE',  ( -54.38796339852894590, -287.8415736881570410, -344.9005210889691853 ) ) ;
#81092 = CARTESIAN_POINT ( 'NONE',  ( -75.88350115612369962, -289.2491505352648460, -332.3822197162926386 ) ) ;
#81093 = ORIENTED_EDGE ( 'NONE', *, *, #41567, .F. ) ;
#81094 = CARTESIAN_POINT ( 'NONE',  ( -12.81562848708069247, -287.4433219292967010, -197.6977550056344342 ) ) ;
#81095 = CARTESIAN_POINT ( 'NONE',  ( 21.49570089064525291, -275.2796840825200775, -227.1147571160295229 ) ) ;
#81096 = EDGE_CURVE ( 'NONE', #2308, #83547, #56490, .T. ) ;
#81097 = CARTESIAN_POINT ( 'NONE',  ( 38.92029238707755923, -292.3646596883158963, -261.7742424161612576 ) ) ;
#81098 = CARTESIAN_POINT ( 'NONE',  ( 25.02948034077640571, -282.8009855733371296, -315.3628977539175935 ) ) ;
#81099 = CARTESIAN_POINT ( 'NONE',  ( 33.94673017477119004, -283.4199389111307141, -297.5763243271287593 ) ) ;
#81100 = CARTESIAN_POINT ( 'NONE',  ( -33.05568014553059442, -283.3328630566061292, -347.2336945856786201 ) ) ;
#81101 = CARTESIAN_POINT ( 'NONE',  ( 4.931943334121755562, -280.9745944060103398, -210.8209923937971553 ) ) ;
#81102 = CARTESIAN_POINT ( 'NONE',  ( -92.08974858914540107, -293.4094976428775681, -313.9805196606274080 ) ) ;
#81103 = CARTESIAN_POINT ( 'NONE',  ( 139.2571438113172633, 180.4774994735251994, -241.5552550638034859 ) ) ;
#81104 = ORIENTED_EDGE ( 'NONE', *, *, #67389, .T. ) ;
#81105 = CARTESIAN_POINT ( 'NONE',  ( 36.65065063670046897, -277.4072407555393625, -259.0875783784314308 ) ) ;
#81106 = CARTESIAN_POINT ( 'NONE',  ( 152.8849392923119410, 207.2903029783794011, -216.9541755379844403 ) ) ;
#81107 = CARTESIAN_POINT ( 'NONE',  ( -49.96337633816796853, -297.2354167151027582, -198.3570489480232197 ) ) ;
#81108 = CARTESIAN_POINT ( 'NONE',  ( 39.17517298197189035, -293.1666106410748966, -278.8942770213425888 ) ) ;
#81109 = CARTESIAN_POINT ( 'NONE',  ( -46.80064229255074082, -155.6065870646474991, -361.5538532369118343 ) ) ;
#81111 = CARTESIAN_POINT ( 'NONE',  ( -53.60443062215115617, -287.6641699959375273, -342.3469777737124105 ) ) ;
#81110 = CARTESIAN_POINT ( 'NONE',  ( -37.23604188324430453, -296.6281871560266836, -193.9496097253216078 ) ) ;
#81112 = CARTESIAN_POINT ( 'NONE',  ( -6.225953906302037488, -296.4993180164240130, -337.7604935021706183 ) ) ;
#81113 = CARTESIAN_POINT ( 'NONE',  ( 23.93604853365003038, -288.3070496038653800, -229.6946232054161214 ) ) ;
#81114 = EDGE_LOOP ( 'NONE', ( #7175, #55842, #29985, #45546, #61096, #36611 ) ) ;
#81115 = CARTESIAN_POINT ( 'NONE',  ( 15.32598778891112978, -295.2707988202014349, -326.2085428286755473 ) ) ;
#81116 = CARTESIAN_POINT ( 'NONE',  ( -110.4519534791522659, -285.0371887254378862, -270.9160186227093163 ) ) ;
#81117 = CARTESIAN_POINT ( 'NONE',  ( -3.612408327879128134, -297.2605349072478020, -193.7649110999839763 ) ) ;
#81118 = CARTESIAN_POINT ( 'NONE',  ( -4.682081716713339503, -293.2743500184636787, -200.8089207022684093 ) ) ;
#81119 = CARTESIAN_POINT ( 'NONE',  ( 33.36249715357018886, -294.4327441453648930, -300.8345012732876853 ) ) ;
#81120 = CARTESIAN_POINT ( 'NONE',  ( -34.85940900976114420, -292.2508812796249345, -197.4033340569970960 ) ) ;
#81121 = ORIENTED_EDGE ( 'NONE', *, *, #22861, .T. ) ;
#81122 = FACE_OUTER_BOUND ( 'NONE', #18451, .T. ) ;
#81123 = CARTESIAN_POINT ( 'NONE',  ( -35.88208377262943571, -299.9306490915744234, -194.5958537802862338 ) ) ;
#81124 = CARTESIAN_POINT ( 'NONE',  ( 7.017615659521933225, -273.4359129123248522, -207.8439515411113803 ) ) ;
#81125 = ORIENTED_EDGE ( 'NONE', *, *, #39601, .T. ) ;
#81126 = CARTESIAN_POINT ( 'NONE',  ( -75.31129124947567277, -277.0520165697235484, -337.2777605563284169 ) ) ;
#81127 = CARTESIAN_POINT ( 'NONE',  ( -40.52876287109086917, -296.4912599921035508, -196.7240627453659840 ) ) ;
#81128 = CARTESIAN_POINT ( 'NONE',  ( -111.6278932407283691, -280.4086155239939444, -270.6663847939050811 ) ) ;
#81129 = CARTESIAN_POINT ( 'NONE',  ( 34.78103651359941750, -273.9205020976803553, -287.9980050952301553 ) ) ;
#81130 = CARTESIAN_POINT ( 'NONE',  ( -66.99375193943554052, -298.8597163750683308, -203.2065673810634507 ) ) ;
#81131 = CARTESIAN_POINT ( 'NONE',  ( -91.30399596762678982, -274.2018672948210565, -220.8301371711825425 ) ) ;
#81132 = CARTESIAN_POINT ( 'NONE',  ( -75.93760363468544483, -275.3046920651395908, -204.8455145941681508 ) ) ;
#81133 = CARTESIAN_POINT ( 'NONE',  ( -18.92697745587564384, -272.3080288994905800, -197.2367124416590514 ) ) ;
#81134 = CARTESIAN_POINT ( 'NONE',  ( -105.0532035735895278, -296.8350223503308598, -297.9118887351315834 ) ) ;
#81135 = CARTESIAN_POINT ( 'NONE',  ( 23.84114592328646154, -291.5635845737907061, -229.4706023793314387 ) ) ;
#81136 = CARTESIAN_POINT ( 'NONE',  ( 193.8739039770516968, 214.6009552038330526, 16.65543863426445270 ) ) ;
#81137 = CARTESIAN_POINT ( 'NONE',  ( 30.49177328673300380, -276.5153797471604662, -306.7799177930620544 ) ) ;
#81138 = CARTESIAN_POINT ( 'NONE',  ( 33.83328632781571343, -275.5041863207380857, -254.0842228874323325 ) ) ;
#81139 = CARTESIAN_POINT ( 'NONE',  ( -80.64519636445542972, -284.1634609480477707, -207.2249561492333783 ) ) ;
#81140 = CARTESIAN_POINT ( 'NONE',  ( -111.5829074091532362, -298.7040071300628483, -258.5205138357268879 ) ) ;
#81141 = CARTESIAN_POINT ( 'NONE',  ( 207.6662022560301182, 36.29800326561209545, 14.90057469441957316 ) ) ;
#81142 = CARTESIAN_POINT ( 'NONE',  ( -10.68162471579387507, -285.6061263622431170, -202.2164956722405122 ) ) ;
#81143 = CARTESIAN_POINT ( 'NONE',  ( -87.12680032124481500, -281.7431171282759124, -326.7464627112561288 ) ) ;
#81144 = CARTESIAN_POINT ( 'NONE',  ( -105.2094247737140336, -276.3989058013166868, -300.0183623878365893 ) ) ;
#81145 = CARTESIAN_POINT ( 'NONE',  ( -41.91116146937901021, -275.6855488254684019, -343.8210415753244433 ) ) ;
#81146 = CARTESIAN_POINT ( 'NONE',  ( -72.09033144272315496, -281.5928239206886019, -203.8823139526549824 ) ) ;
#81147 = CARTESIAN_POINT ( 'NONE',  ( 25.60853230369290756, -276.2397171162194240, -232.5215005462403610 ) ) ;
#81148 = CARTESIAN_POINT ( 'NONE',  ( 140.6539576904058606, 250.5000000000000568, 12.00000000000000000 ) ) ;
#81149 = CARTESIAN_POINT ( 'NONE',  ( -4.155900712283271403, -272.8822561361930070, -201.7527120644970751 ) ) ;
#81150 = CARTESIAN_POINT ( 'NONE',  ( -101.8515968014017830, -281.0687960857908365, -231.6787520485760012 ) ) ;
#81151 = CARTESIAN_POINT ( 'NONE',  ( 152.2747007761510076, 129.8137010776104603, 12.50000000000000178 ) ) ;
#81152 = CARTESIAN_POINT ( 'NONE',  ( -72.95631528853381553, -287.5045709336444588, -203.6629816887706568 ) ) ;
#81153 = CARTESIAN_POINT ( 'NONE',  ( 155.0741174296533984, 18.62644422905990638, -11.41100038915083914 ) ) ;
#81154 = CARTESIAN_POINT ( 'NONE',  ( -84.15084003026952075, -287.6950971216859898, -329.0263352753115669 ) ) ;
#81155 = CARTESIAN_POINT ( 'NONE',  ( 82.13289967990638729, -300.8078083816499770, -196.9362037238964547 ) ) ;
#81156 = CARTESIAN_POINT ( 'NONE',  ( -94.98917991864817623, -271.8759651007783873, -224.7759059781753592 ) ) ;
#81157 = CARTESIAN_POINT ( 'NONE',  ( -111.4777333574609344, -288.7530537491341533, -265.6337423474823822 ) ) ;
#81158 = CARTESIAN_POINT ( 'NONE',  ( -98.31850732666445936, -258.1384851437703674, -325.6453615436536211 ) ) ;
#81159 = CARTESIAN_POINT ( 'NONE',  ( 113.5000000000000568, -211.8141737103562434, -518.0411269958476623 ) ) ;
#81160 = CARTESIAN_POINT ( 'NONE',  ( 37.14389035191657484, -286.2419176999983392, -286.9919003115932696 ) ) ;
#81161 = CARTESIAN_POINT ( 'NONE',  ( -38.88156114600245417, -284.6718822012624059, -344.1576822308709893 ) ) ;
#81162 = CARTESIAN_POINT ( 'NONE',  ( -108.0768612491187639, -283.1502107414489728, -242.4600521636990322 ) ) ;
#81163 = CARTESIAN_POINT ( 'NONE',  ( -104.7030699935923224, -290.9310985910718728, -242.0969267024317730 ) ) ;
#81164 = CARTESIAN_POINT ( 'NONE',  ( 28.29883504831773422, -282.5280022861361999, -236.9811566978089559 ) ) ;
#81165 = CARTESIAN_POINT ( 'NONE',  ( -8.421022560577354099, -283.4664089788720958, -337.5637677543663244 ) ) ;
#81166 = CARTESIAN_POINT ( 'NONE',  ( -26.35883693561027385, -290.8929229774543614, -344.9116613525393973 ) ) ;
#81167 = CARTESIAN_POINT ( 'NONE',  ( -48.97208509230587481, -298.0747154951972107, -194.1908688108873946 ) ) ;
#81168 = CARTESIAN_POINT ( 'NONE',  ( -43.09745856201845982, -287.2041386406997958, -345.7015815009527273 ) ) ;
#81169 = CARTESIAN_POINT ( 'NONE',  ( 35.20097124020939816, -275.8797668597750317, -296.3361183855998320 ) ) ;
#81170 = CARTESIAN_POINT ( 'NONE',  ( -75.84926095790396516, -293.5156267409894326, -206.3553586539070750 ) ) ;
#81171 = CARTESIAN_POINT ( 'NONE',  ( 152.4536156746142410, 250.5000000000000568, -14.50000000000000000 ) ) ;
#81172 = CARTESIAN_POINT ( 'NONE',  ( -37.37352853689063892, -282.5519495502701943, -195.3611179825600175 ) ) ;
#81173 = CARTESIAN_POINT ( 'NONE',  ( -111.4251638451020625, -276.7148886522541034, -257.6462120927429851 ) ) ;
#81174 = DIRECTION ( 'NONE',  ( -0.000000000000000000, -1.000000000000000000, -0.000000000000000000 ) ) ;
#81175 = CARTESIAN_POINT ( 'NONE',  ( -100.0802968076212522, -295.5292642151891869, -227.0911278678306644 ) ) ;
#81176 = CARTESIAN_POINT ( 'NONE',  ( -3.828115394928857995, -275.9463152518902689, -335.3282812792550658 ) ) ;
#81177 = CARTESIAN_POINT ( 'NONE',  ( -110.9393000054353848, -292.1330474482526256, -265.7109778318026088 ) ) ;
#81178 = CARTESIAN_POINT ( 'NONE',  ( -66.66927161994094320, -292.5995071177352429, -203.2544715230085330 ) ) ;
#81179 = CARTESIAN_POINT ( 'NONE',  ( -89.59403115579823407, -285.5608774909879344, -322.8512329352829511 ) ) ;
#81180 = CARTESIAN_POINT ( 'NONE',  ( 39.06610522908409422, -294.9406199826531179, -267.4408758182344172 ) ) ;
#81181 = CARTESIAN_POINT ( 'NONE',  ( 32.86517394689387572, -294.4773977508162375, -239.9589288487968304 ) ) ;
#81182 = CARTESIAN_POINT ( 'NONE',  ( 35.53482023703489290, -293.3189499881820552, -265.3184566903651103 ) ) ;
#81183 = CARTESIAN_POINT ( 'NONE',  ( 37.26126986915375028, -289.4533585890311542, -262.6541396555891197 ) ) ;
#81184 = CARTESIAN_POINT ( 'NONE',  ( 34.58826261581754835, -282.0667149979192345, -297.8398454667993178 ) ) ;
#81185 = CARTESIAN_POINT ( 'NONE',  ( -112.9466463274225134, -270.7637583252351305, -264.6946417773449980 ) ) ;
#81186 = CARTESIAN_POINT ( 'NONE',  ( -85.51125822836189627, -285.2400396894515779, -210.2887143606990605 ) ) ;
#81187 = CARTESIAN_POINT ( 'NONE',  ( 18.68613221842540995, -278.2209581168903583, -319.7031097048322295 ) ) ;
#81188 = CARTESIAN_POINT ( 'NONE',  ( -42.68782004208540570, -284.7781555897413455, -197.1463096205446845 ) ) ;
#81189 = CARTESIAN_POINT ( 'NONE',  ( 26.99632535157911661, -285.0347991573499371, -231.7171722181275868 ) ) ;
#81190 = CARTESIAN_POINT ( 'NONE',  ( -109.3679212725146215, -276.9941848409339968, -246.6888339108536456 ) ) ;
#81191 = CARTESIAN_POINT ( 'NONE',  ( -114.4693268140674434, -273.6886850827510216, -284.2063049943780015 ) ) ;
#81192 = CARTESIAN_POINT ( 'NONE',  ( -87.73241653717960276, -284.8324266291617732, -217.4577708169034622 ) ) ;
#81193 = CARTESIAN_POINT ( 'NONE',  ( 36.59769847098299067, -282.5045859886839708, -250.2870757476581218 ) ) ;
#81194 = CARTESIAN_POINT ( 'NONE',  ( -70.54817239863834288, -288.5380006093341194, -339.5864729170215810 ) ) ;
#81195 = CARTESIAN_POINT ( 'NONE',  ( 34.93456752430741119, -295.1041237575412310, -254.3616042233055055 ) ) ;
#81196 = CARTESIAN_POINT ( 'NONE',  ( -48.35797936653824536, -278.7901101711087790, -345.8139334309867650 ) ) ;
#81197 = CARTESIAN_POINT ( 'NONE',  ( 16.61935737316933981, -277.6196551414937517, -324.6707318905287138 ) ) ;
#81198 = CARTESIAN_POINT ( 'NONE',  ( -24.87430416598558480, -280.0489614866456805, -198.4336264204988254 ) ) ;
#81199 = CARTESIAN_POINT ( 'NONE',  ( -35.10398325353420290, -300.0803836229325157, -195.5270108691089490 ) ) ;
#81200 = CARTESIAN_POINT ( 'NONE',  ( 28.63509732596806501, -286.0228955493852823, -305.7855054670853292 ) ) ;
#81201 = CARTESIAN_POINT ( 'NONE',  ( -110.0126609545595926, -291.8592385785266288, -293.4543401422267266 ) ) ;
#81202 = CARTESIAN_POINT ( 'NONE',  ( -50.54029706534402067, -294.1450064490936143, -342.4723037419922775 ) ) ;
#81203 = ORIENTED_EDGE ( 'NONE', *, *, #6509, .F. ) ;
#81204 = CARTESIAN_POINT ( 'NONE',  ( -39.69396982502791360, -294.7491881178716540, -343.3567987811692319 ) ) ;
#81205 = CARTESIAN_POINT ( 'NONE',  ( -109.5697662326491724, -291.3033273372230951, -296.2982938339348493 ) ) ;
#81206 = CARTESIAN_POINT ( 'NONE',  ( -98.08292487737951149, -279.7687812167593506, -229.5969493747275578 ) ) ;
#81207 = EDGE_CURVE ( 'NONE', #5562, #83883, #73099, .T. ) ;
#81208 = CARTESIAN_POINT ( 'NONE',  ( -109.8756055228439834, -271.9287356430028240, -245.2284145694832489 ) ) ;
#81209 = CARTESIAN_POINT ( 'NONE',  ( 24.06582193259179903, -288.8207150812963846, -316.6474984990423991 ) ) ;
#81210 = CARTESIAN_POINT ( 'NONE',  ( -8.237192175341450096, -289.0146020207796482, -341.6401820037439734 ) ) ;
#81211 = CARTESIAN_POINT ( 'NONE',  ( -93.27403225407111620, -285.5518670442850748, -223.4179426553355938 ) ) ;
#81212 = CARTESIAN_POINT ( 'NONE',  ( 175.2296996224750103, 250.0000000000000568, 0.000000000000000000 ) ) ;
#81213 = CARTESIAN_POINT ( 'NONE',  ( 82.92025895306024097, 83.20676217455302037, -300.2504679712564553 ) ) ;
#81214 = CARTESIAN_POINT ( 'NONE',  ( -70.26940817115894333, -195.8484599149890073, -356.6074167248179378 ) ) ;
#81215 = CARTESIAN_POINT ( 'NONE',  ( 11.84872889966633736, -275.5452533590565167, -324.5861405847504102 ) ) ;
#81216 = CARTESIAN_POINT ( 'NONE',  ( -103.6435683292885415, -277.8947443028860107, -238.9642479356203069 ) ) ;
#81217 = CARTESIAN_POINT ( 'NONE',  ( -95.06780847111842547, -272.9086296281636805, -219.4352826223653494 ) ) ;
#81218 = CARTESIAN_POINT ( 'NONE',  ( 104.4767245839417882, 114.1861031128568129, -280.3257878957174398 ) ) ;
#81219 = CARTESIAN_POINT ( 'NONE',  ( -48.43911547166732134, -275.8752772437485419, -346.1123941580989367 ) ) ;
#81220 = CARTESIAN_POINT ( 'NONE',  ( -71.59689116425990107, -297.2586104950106574, -338.1885158671365730 ) ) ;
#81221 = CARTESIAN_POINT ( 'NONE',  ( -57.67807833190245503, -292.2748651219350222, -200.1339822480225337 ) ) ;
#81222 = CARTESIAN_POINT ( 'NONE',  ( -95.45569687099602163, -298.0361162550571521, -220.0131935004228581 ) ) ;
#81223 = CARTESIAN_POINT ( 'NONE',  ( -36.90359686735268241, -298.5498438543773432, -193.4226204581699164 ) ) ;
#81224 = CARTESIAN_POINT ( 'NONE',  ( -70.46944551625000486, -297.7694525685462850, -205.2968219823161746 ) ) ;
#81225 = VERTEX_POINT ( 'NONE', #72025 ) ;
#81226 = DIRECTION ( 'NONE',  ( 0.000000000000000000, 0.000000000000000000, -1.000000000000000000 ) ) ;
#81227 = CARTESIAN_POINT ( 'NONE',  ( -111.3776692228935161, -280.2790515053716263, -285.5242811224306365 ) ) ;
#81228 = CARTESIAN_POINT ( 'NONE',  ( -41.57202976823054286, -282.6116064330056474, -347.2354775583726223 ) ) ;
#81229 = CARTESIAN_POINT ( 'NONE',  ( -92.44985349180895184, -280.3191176864269210, -221.9962056982960803 ) ) ;
#81230 = CARTESIAN_POINT ( 'NONE',  ( -108.7763599518977884, -279.9789757689379144, -296.4198064831964530 ) ) ;
#81231 = CARTESIAN_POINT ( 'NONE',  ( -64.80940502125579883, -272.1666873750790501, -201.9645246539039363 ) ) ;
#81232 = DIRECTION ( 'NONE',  ( 0.000000000000000000, 0.000000000000000000, 1.000000000000000000 ) ) ;
#81233 = FACE_BOUND ( 'NONE', #71970, .T. ) ;
#81234 = CARTESIAN_POINT ( 'NONE',  ( -27.56047655018827669, -280.3464107401491674, -197.9681849790304398 ) ) ;
#81235 = CARTESIAN_POINT ( 'NONE',  ( 33.56059034655385176, -275.9760130332741142, -240.6091487538548961 ) ) ;
#81236 = CARTESIAN_POINT ( 'NONE',  ( 36.25122665503943153, -277.3666505411950993, -255.9014575707936956 ) ) ;
#81237 = CARTESIAN_POINT ( 'NONE',  ( -4.266453781182229399, -275.1994211951595162, -339.2568102565784898 ) ) ;
#81238 = ORIENTED_EDGE ( 'NONE', *, *, #15024, .F. ) ;
#81239 = CARTESIAN_POINT ( 'NONE',  ( 185.2519943799831879, 3.000000000000000000, 10.00000000000000000 ) ) ;
#81240 = CARTESIAN_POINT ( 'NONE',  ( 12.60975930829918035, -284.3402093709125893, -326.8509687194577396 ) ) ;
#81241 = CARTESIAN_POINT ( 'NONE',  ( -49.70597577007611534, -291.0877180726020583, -198.2005511889541367 ) ) ;
#81242 = CARTESIAN_POINT ( 'NONE',  ( -63.15939255558951260, -285.0730949495654158, -197.9265989727552437 ) ) ;
#81243 = CARTESIAN_POINT ( 'NONE',  ( -111.3328080770970274, -282.7490649166518324, -273.6612706559420758 ) ) ;
#81245 = CARTESIAN_POINT ( 'NONE',  ( 36.70932245555122364, -285.5336757920342166, -262.7611014771114810 ) ) ;
#81244 = CARTESIAN_POINT ( 'NONE',  ( -8.278098004815507949, -281.2386641966512570, -337.9679367943122656 ) ) ;
#81246 = CARTESIAN_POINT ( 'NONE',  ( 2.908983637272627654, -281.8103999212079884, -208.9241445252194751 ) ) ;
#81247 = CARTESIAN_POINT ( 'NONE',  ( -108.2036598348584988, -270.8699978517628892, -245.7931853405240759 ) ) ;
#81248 = CARTESIAN_POINT ( 'NONE',  ( -61.00282083519147847, -281.7539872453096450, -342.8495905510337707 ) ) ;
#81249 = CARTESIAN_POINT ( 'NONE',  ( 35.80491741264854255, -295.3388831302748940, -253.7333811615970944 ) ) ;
#81250 = CARTESIAN_POINT ( 'NONE',  ( -87.15894502997495863, -278.4200999510301244, -323.8600411337701530 ) ) ;
#81251 = CARTESIAN_POINT ( 'NONE',  ( -49.08406813156094017, -287.9031698753166779, -196.0648369469861905 ) ) ;
#81252 = ADVANCED_FACE ( 'NONE', ( #57347 ), #86187, .F. ) ;
#81253 = EDGE_CURVE ( 'NONE', #60748, #50317, #21339, .T. ) ;
#81254 = CARTESIAN_POINT ( 'NONE',  ( 209.3463262141449661, 1.051285333831499136, -7.457902384259533335 ) ) ;
#81255 = CARTESIAN_POINT ( 'NONE',  ( -101.9965865210954377, -292.9935195910395578, -231.1569917194355241 ) ) ;
#81256 = CARTESIAN_POINT ( 'NONE',  ( 36.60166337140330484, -273.3899329055136604, -257.7395825494043038 ) ) ;
#81257 = CARTESIAN_POINT ( 'NONE',  ( -75.59218773248352363, -288.7462402929367613, -337.0023891180822488 ) ) ;
#81258 = CARTESIAN_POINT ( 'NONE',  ( 28.20632927188960082, -291.4958893708869141, -236.4509977397852651 ) ) ;
#81259 = CARTESIAN_POINT ( 'NONE',  ( -48.18343439339133027, -267.2165102599228135, -440.1639404234281301 ) ) ;
#81260 = CARTESIAN_POINT ( 'NONE',  ( -99.60172158447142010, -276.7002309264416908, -309.5066041128490610 ) ) ;
#81261 = CARTESIAN_POINT ( 'NONE',  ( -108.0529894272545732, -294.3950627734656678, -293.1281215358523013 ) ) ;
#81262 = CARTESIAN_POINT ( 'NONE',  ( -109.7656357839777570, -292.0348096266854441, -257.5795006073743707 ) ) ;
#81263 = LINE ( 'NONE', #31553, #71461 ) ;
#81264 = CARTESIAN_POINT ( 'NONE',  ( 199.0143093133015668, 16.83012701892219098, 9.999999999999998224 ) ) ;
#81265 = CARTESIAN_POINT ( 'NONE',  ( 3.784309863321918321, -291.0744258250283565, -206.0228280620011674 ) ) ;
#81266 = CARTESIAN_POINT ( 'NONE',  ( 28.36118508618228518, -288.6992533750243979, -236.6394093944941233 ) ) ;
#81267 = CARTESIAN_POINT ( 'NONE',  ( -87.95758496441295904, -289.5954569490654649, -213.6865539008864232 ) ) ;
#81268 = CARTESIAN_POINT ( 'NONE',  ( -8.036849414009644477, -287.8690213044634447, -202.8585206774452274 ) ) ;
#81269 = DIRECTION ( 'NONE',  ( -0.000000000000000000, -1.000000000000000000, -0.000000000000000000 ) ) ;
#81270 = CARTESIAN_POINT ( 'NONE',  ( 35.12172837380102663, -288.4888993508541262, -280.5347457627498784 ) ) ;
#81271 = CARTESIAN_POINT ( 'NONE',  ( 24.38219372006125596, -296.1163363189299389, -313.6105805481400921 ) ) ;
#81272 = DIRECTION ( 'NONE',  ( 0.000000000000000000, 1.000000000000000000, -0.000000000000000000 ) ) ;
#81273 = CARTESIAN_POINT ( 'NONE',  ( -34.66524695905027897, -290.2242894414718535, -346.9172759190810780 ) ) ;
#81274 = CARTESIAN_POINT ( 'NONE',  ( -89.89266497888856122, -277.3352484817424966, -216.2809644601839523 ) ) ;
#81275 = CARTESIAN_POINT ( 'NONE',  ( -59.65482564042597602, -277.6667666883224115, -344.0351888713203721 ) ) ;
#81276 = CARTESIAN_POINT ( 'NONE',  ( 21.05283429031712217, -280.5414857760982841, -220.1830962588607292 ) ) ;
#81277 = CARTESIAN_POINT ( 'NONE',  ( -111.0114230219513161, -274.6150527521714935, -259.3269491315330697 ) ) ;
#81278 = CARTESIAN_POINT ( 'NONE',  ( -98.98564862407852161, -283.1316085372211546, -227.6181247792901843 ) ) ;
#81279 = CARTESIAN_POINT ( 'NONE',  ( -48.18343439339131606, -257.5766546844495792, -488.5262689091994730 ) ) ;
#81280 = CARTESIAN_POINT ( 'NONE',  ( -62.70914154084307768, -277.8581682846553917, -200.5404094773799102 ) ) ;
#81281 = CARTESIAN_POINT ( 'NONE',  ( -105.2070147809307770, -282.1321585583525575, -302.2875915225437780 ) ) ;
#81282 = CARTESIAN_POINT ( 'NONE',  ( -109.4300603157634129, -269.0111957867250112, -295.3470538382887867 ) ) ;
#81283 = CARTESIAN_POINT ( 'NONE',  ( -62.19860101427708088, -275.8493931374848671, -342.5615171215882242 ) ) ;
#81284 = CARTESIAN_POINT ( 'NONE',  ( -109.9623686681617301, -298.2359860622638053, -257.8332987720730216 ) ) ;
#81285 = CARTESIAN_POINT ( 'NONE',  ( -113.5979705919323379, -283.3701060021716103, -278.5142599687440566 ) ) ;
#81286 = CARTESIAN_POINT ( 'NONE',  ( -55.36312153228242749, -298.7559470015147554, -199.3252804010661805 ) ) ;
#81287 = CARTESIAN_POINT ( 'NONE',  ( -97.36159442831041133, -274.6147419195990551, -223.0724450925362135 ) ) ;
#81288 = CARTESIAN_POINT ( 'NONE',  ( 0.6270834835491304604, -274.2403444553486906, -207.9875742495381701 ) ) ;
#81289 = CARTESIAN_POINT ( 'NONE',  ( -3.965314640643761379, -294.4924206900255967, -203.1827047360903293 ) ) ;
#81290 = CARTESIAN_POINT ( 'NONE',  ( -93.59134379385628222, -290.0010702836752330, -323.0210130841915657 ) ) ;
#81291 = CARTESIAN_POINT ( 'NONE',  ( -53.42958015600600419, -277.9273395718526558, -196.4801097755100727 ) ) ;
#81292 = CARTESIAN_POINT ( 'NONE',  ( -96.39242224725961705, -289.7202298037295805, -319.7982899446544138 ) ) ;
#81293 = CARTESIAN_POINT ( 'NONE',  ( -68.87009993124429741, -288.5359539375419899, -336.4623165707907333 ) ) ;
#81294 = CARTESIAN_POINT ( 'NONE',  ( 33.57020032810189036, -291.2341105417483504, -245.7803418904064472 ) ) ;
#81295 = ORIENTED_EDGE ( 'NONE', *, *, #80971, .T. ) ;
#81296 = CARTESIAN_POINT ( 'NONE',  ( 197.9840890846857349, 69.90067952545793162, 11.10260959755656174 ) ) ;
#81297 = CARTESIAN_POINT ( 'NONE',  ( -94.33497372814193227, -290.7055407066397947, -224.6273991964368975 ) ) ;
#81298 = DIRECTION ( 'NONE',  ( -0.000000000000000000, -1.000000000000000000, -0.000000000000000000 ) ) ;
#81299 = CARTESIAN_POINT ( 'NONE',  ( 31.20628789008248205, -288.0473889107122432, -235.8069062139917662 ) ) ;
#81300 = CARTESIAN_POINT ( 'NONE',  ( -53.28691492658256834, -285.7662352645559736, -340.3683826091709079 ) ) ;
#81301 = CARTESIAN_POINT ( 'NONE',  ( 32.01228332807568222, -293.0353065566533246, -303.3916041617171686 ) ) ;
#81302 = CARTESIAN_POINT ( 'NONE',  ( -30.24386454247041911, -284.2792983634745951, -346.5380108207003218 ) ) ;
#81303 = CARTESIAN_POINT ( 'NONE',  ( -109.4986889700974189, -284.2352655521664815, -281.7475375758394307 ) ) ;
#81304 = CARTESIAN_POINT ( 'NONE',  ( 28.47958570605879558, -277.3090026658273928, -303.1684304172225666 ) ) ;
#81305 = CARTESIAN_POINT ( 'NONE',  ( -34.77605330411625317, -290.1046560923730908, -195.7604191807333791 ) ) ;
#81306 = CARTESIAN_POINT ( 'NONE',  ( 15.74453713689562662, -273.6192544356102303, -219.6024046098876283 ) ) ;
#81307 = ORIENTED_EDGE ( 'NONE', *, *, #64718, .T. ) ;
#81308 = LINE ( 'NONE', #74211, #80348 ) ;
#81309 = CARTESIAN_POINT ( 'NONE',  ( -37.30422292179076038, -287.9727411305697728, -195.9084390689546353 ) ) ;
#81310 = CARTESIAN_POINT ( 'NONE',  ( -113.3443784492282020, -297.4982220499722985, -281.0006568820179496 ) ) ;
#81311 = CARTESIAN_POINT ( 'NONE',  ( -44.04196611058176103, -286.6166151926872203, -197.5668935966541540 ) ) ;
#81312 = CARTESIAN_POINT ( 'NONE',  ( -113.4821331940253089, -277.7385326713653626, -260.1871278906868383 ) ) ;
#81313 = CARTESIAN_POINT ( 'NONE',  ( 35.35352747067980772, -293.8852568680878790, -245.1257620952529521 ) ) ;
#81314 = CARTESIAN_POINT ( 'NONE',  ( 26.39269665070026605, -286.2390620322331074, -311.4240389712932711 ) ) ;
#81315 = CARTESIAN_POINT ( 'NONE',  ( 38.58613285433296625, -294.0450194006032802, -283.1180974408335942 ) ) ;
#81316 = CARTESIAN_POINT ( 'NONE',  ( -70.23404068746381768, -291.9394870254791954, -205.1677025221914334 ) ) ;
#81317 = FACE_OUTER_BOUND ( 'NONE', #19519, .T. ) ;
#81318 = CARTESIAN_POINT ( 'NONE',  ( 85.09997405915690649, 81.31097194785500903, -298.9058856463690290 ) ) ;
#81319 = CARTESIAN_POINT ( 'NONE',  ( -80.56158883095672252, -286.9983004016568771, -207.4105338568816137 ) ) ;
#81320 = CARTESIAN_POINT ( 'NONE',  ( -72.02372285203398405, -277.1237833571632905, -198.2697987213421698 ) ) ;
#81321 = ORIENTED_EDGE ( 'NONE', *, *, #3347, .T. ) ;
#81322 = CARTESIAN_POINT ( 'NONE',  ( -18.67012212205499111, -281.7264401183609266, -341.3051949448220626 ) ) ;
#81323 = CARTESIAN_POINT ( 'NONE',  ( -104.7730214049796871, -278.6999484682532398, -233.2294441407206875 ) ) ;
#81324 = CARTESIAN_POINT ( 'NONE',  ( 36.03320654325722927, -283.7423361360032459, -285.1278041019679677 ) ) ;
#81325 = CARTESIAN_POINT ( 'NONE',  ( 66.82556401647084954, 46.20335925335534455, -317.4906725690062785 ) ) ;
#81326 = CARTESIAN_POINT ( 'NONE',  ( -58.34236709178786384, -281.8930107278820856, -343.8844082265167685 ) ) ;
#81327 = CARTESIAN_POINT ( 'NONE',  ( 23.34318196787115696, -284.9771508198932111, -226.8091009963864337 ) ) ;
#81328 = CARTESIAN_POINT ( 'NONE',  ( -16.14599672560019528, -276.1836196671497987, -197.5670846912198328 ) ) ;
#81329 = CARTESIAN_POINT ( 'NONE',  ( -71.69947979957566986, -298.0775888007794947, -205.8679853551003021 ) ) ;
#81330 = CARTESIAN_POINT ( 'NONE',  ( -37.01003171226221156, -293.7327053368494489, -343.8660299603760109 ) ) ;
#81331 = CARTESIAN_POINT ( 'NONE',  ( -106.0881764365554716, -279.6487025778943689, -235.7862254908652915 ) ) ;
#81332 = CARTESIAN_POINT ( 'NONE',  ( -9.988363180829333388, -276.6847911203981312, -338.0562539702432332 ) ) ;
#81333 = CARTESIAN_POINT ( 'NONE',  ( 30.51773547607830395, -299.8235251788059941, -193.5858418448398481 ) ) ;
#81334 = CARTESIAN_POINT ( 'NONE',  ( 5.686445206171891975, -275.4042148266325967, -333.8439599020867377 ) ) ;
#81335 = CARTESIAN_POINT ( 'NONE',  ( 164.2231345125756263, 300.2961574867697436, 7.500000000000000000 ) ) ;
#81336 = CARTESIAN_POINT ( 'NONE',  ( 26.82474003563958931, -274.0734160259896157, -309.2887839668493939 ) ) ;
#81337 = CARTESIAN_POINT ( 'NONE',  ( -101.8289202621643312, -298.5187736273210817, -229.3732571988008715 ) ) ;
#81338 = DIRECTION ( 'NONE',  ( 0.000000000000000000, 1.000000000000000000, 0.000000000000000000 ) ) ;
#81339 = CARTESIAN_POINT ( 'NONE',  ( -110.2140734402150315, -271.0703965937372004, -283.6296548450457635 ) ) ;
#81340 = CARTESIAN_POINT ( 'NONE',  ( -108.9698682338513009, -285.8376328758349700, -254.6937588525607907 ) ) ;
#81341 = CARTESIAN_POINT ( 'NONE',  ( -52.69072012957874307, -285.0062027726391420, -344.8351931436837958 ) ) ;
#81342 = CARTESIAN_POINT ( 'NONE',  ( 16.05458418754304262, -286.1833120211005621, -220.4154012836551999 ) ) ;
#81343 = CARTESIAN_POINT ( 'NONE',  ( -83.52307047194003076, -276.0971419712317356, -327.9918357338194710 ) ) ;
#81344 = CARTESIAN_POINT ( 'NONE',  ( -68.27787930424383944, -285.3233100589075093, -337.8431029952679410 ) ) ;
#81345 = CARTESIAN_POINT ( 'NONE',  ( -93.60715118031951931, -277.7022325903813567, -222.7506770376182885 ) ) ;
#81346 = CARTESIAN_POINT ( 'NONE',  ( 9.873583870998631440, -277.4633677864011361, -326.4409096151675271 ) ) ;
#81347 = CARTESIAN_POINT ( 'NONE',  ( 207.0561972617101674, 35.35788477359428583, 15.00000000000000178 ) ) ;
#81348 = CARTESIAN_POINT ( 'NONE',  ( -46.19244642374174248, -274.4291911342560866, -197.8376546648480314 ) ) ;
#81349 = CARTESIAN_POINT ( 'NONE',  ( 21.83978537285823762, -281.6947813910225022, -221.3538675489834588 ) ) ;
#81350 = CARTESIAN_POINT ( 'NONE',  ( -53.75347074004272230, -280.3394526330582721, -195.1389079685595505 ) ) ;
#81351 = ORIENTED_EDGE ( 'NONE', *, *, #42527, .F. ) ;
#81352 = EDGE_LOOP ( 'NONE', ( #72369, #84728 ) ) ;
#81353 = CARTESIAN_POINT ( 'NONE',  ( 196.8865788344860164, 19.32388290151324028, -12.43054049969427588 ) ) ;
#81354 = CARTESIAN_POINT ( 'NONE',  ( 37.86747419535247161, -289.5343562493065974, -279.9430820895992724 ) ) ;
#81355 = CARTESIAN_POINT ( 'NONE',  ( -109.2023493307237914, -295.9309814179370051, -256.5594944881757442 ) ) ;
#81356 = CARTESIAN_POINT ( 'NONE',  ( -64.34522807906411401, -291.0575650914665289, -198.3041729302228475 ) ) ;
#81357 = CARTESIAN_POINT ( 'NONE',  ( 33.74561369506310626, -286.2884649720591028, -289.9745456191522521 ) ) ;
#81358 = CARTESIAN_POINT ( 'NONE',  ( 19.96097293214453572, -286.7744640986632021, -316.5323057434561065 ) ) ;
#81359 = AXIS2_PLACEMENT_3D ( 'NONE', #26799, #5961, #12597 ) ;
#81360 = CARTESIAN_POINT ( 'NONE',  ( -94.44057324830791345, -286.4060842098854209, -224.2234177018688115 ) ) ;
#81361 = CARTESIAN_POINT ( 'NONE',  ( -111.0263549127709410, -276.7324355071842206, -256.3078387516918610 ) ) ;
#81362 = CARTESIAN_POINT ( 'NONE',  ( -20.69126801014350647, -287.2418510029499998, -344.7738281839484671 ) ) ;
#81363 = CARTESIAN_POINT ( 'NONE',  ( -10.72811651100436059, -288.3992486793349030, -200.1864893045815847 ) ) ;
#81364 = CARTESIAN_POINT ( 'NONE',  ( -72.34331628848264018, -287.5139770990570014, -336.8955619537001667 ) ) ;
#81365 = CARTESIAN_POINT ( 'NONE',  ( 3.531447220981597468, -283.4290639767513653, -331.1908326551225628 ) ) ;
#81366 = CARTESIAN_POINT ( 'NONE',  ( -111.8523868708366251, -292.6841544289595163, -260.0702160009950603 ) ) ;
#81367 = CARTESIAN_POINT ( 'NONE',  ( 82.17440492340898572, -297.5479941798179766, -195.4018648718562758 ) ) ;
#81368 = ADVANCED_FACE ( 'NONE', ( #79113 ), #14261, .T. ) ;
#81369 = CARTESIAN_POINT ( 'NONE',  ( 155.7140808774800007, 20.99999999999999645, -15.62500000000000711 ) ) ;
#81370 = CARTESIAN_POINT ( 'NONE',  ( -43.20291855017449478, -299.8989806329308294, -194.9765699901674907 ) ) ;
#81371 = CARTESIAN_POINT ( 'NONE',  ( -5.478949716187477392, -279.6795877892465114, -204.5024293851987238 ) ) ;
#81372 = CARTESIAN_POINT ( 'NONE',  ( 36.67329314420914699, -279.7075511315860581, -282.4764562279408437 ) ) ;
#81373 = CARTESIAN_POINT ( 'NONE',  ( -36.28694200525179525, -294.2364525765680696, -347.2054790667232282 ) ) ;
#81374 = CARTESIAN_POINT ( 'NONE',  ( -98.67045888005063148, -271.3611402587774819, -228.8359544951688349 ) ) ;
#81375 = CARTESIAN_POINT ( 'NONE',  ( 36.78577978026066830, -273.7201423301747809, -277.1751416586939740 ) ) ;
#81376 = CARTESIAN_POINT ( 'NONE',  ( -10.29302344350573684, -296.0067533491657628, -338.6956814769762332 ) ) ;
#81377 = DIRECTION ( 'NONE',  ( 0.000000000000000000, 0.000000000000000000, -1.000000000000000000 ) ) ;
#81378 = CARTESIAN_POINT ( 'NONE',  ( -26.31477977795560008, -296.6677219392449274, -194.0572370515587295 ) ) ;
#81379 = CARTESIAN_POINT ( 'NONE',  ( -78.94119356547467703, -293.8446010281147096, -333.9492942262800170 ) ) ;
#81380 = CARTESIAN_POINT ( 'NONE',  ( 25.34032596684660632, -294.4490716688201246, -231.7113560091423210 ) ) ;
#81381 = DIRECTION ( 'NONE',  ( 0.000000000000000000, 0.000000000000000000, 1.000000000000000000 ) ) ;
#81382 = CARTESIAN_POINT ( 'NONE',  ( 27.62524867361743830, -293.8984636010243889, -236.7174367059492965 ) ) ;
#81383 = CYLINDRICAL_SURFACE ( 'NONE', #74691, 6.654241149514406040 ) ;
#81385 = CARTESIAN_POINT ( 'NONE',  ( -50.47120694303523436, -295.2245040643452967, -342.1706998696318465 ) ) ;
#81384 = CARTESIAN_POINT ( 'NONE',  ( -112.1830620587764145, -282.6845268662134458, -261.5760541710594111 ) ) ;
#81386 = CARTESIAN_POINT ( 'NONE',  ( 19.78351099337463026, -282.2539338830199540, -322.0696422999189963 ) ) ;
#81387 = CARTESIAN_POINT ( 'NONE',  ( 7.668760580706223351, -282.5808814582451305, -209.6052980017566369 ) ) ;
#81388 = CARTESIAN_POINT ( 'NONE',  ( -69.78006142819397439, -285.3033658619228277, -200.5363206065779877 ) ) ;
#81389 = CARTESIAN_POINT ( 'NONE',  ( -78.23625058208033067, -289.5005245633677760, -207.6900387831504418 ) ) ;
#81390 = CARTESIAN_POINT ( 'NONE',  ( 205.7786681169002350, 32.98517505407394168, 10.00000000000000000 ) ) ;
#81391 = CARTESIAN_POINT ( 'NONE',  ( -1.934187046497397588, -285.2159557426453489, -205.9025260038430076 ) ) ;
#81392 = CARTESIAN_POINT ( 'NONE',  ( -96.16285584303419398, -288.8073861016825958, -319.5908826408016807 ) ) ;
#81393 = CYLINDRICAL_SURFACE ( 'NONE', #77889, 0.9999999999999991118 ) ;
#81394 = CARTESIAN_POINT ( 'NONE',  ( -7.647927608291255730, -296.2564634006638471, -337.9375599932996579 ) ) ;
#81395 = CARTESIAN_POINT ( 'NONE',  ( -112.7149367621744318, -279.8192653164257990, -282.9102810096326266 ) ) ;
#81397 = CARTESIAN_POINT ( 'NONE',  ( 32.97866413002670782, -281.4788522812967244, -290.0368354391640082 ) ) ;
#81396 = CARTESIAN_POINT ( 'NONE',  ( 16.37106635171574354, -292.3144476596136201, -323.2874188217909364 ) ) ;
#81398 = CARTESIAN_POINT ( 'NONE',  ( -8.386067436567360645, -294.8502094787792771, -341.7658402314601176 ) ) ;
#81399 = CARTESIAN_POINT ( 'NONE',  ( -110.1113746663502582, -282.3722212337845576, -290.7053718961213917 ) ) ;
#81400 = CARTESIAN_POINT ( 'NONE',  ( -71.89597354845865596, -279.5090360629486668, -336.9412160895406032 ) ) ;
#81401 = CARTESIAN_POINT ( 'NONE',  ( 6.193218587319894830, -293.5038060208798356, -329.3150502127592745 ) ) ;
#81402 = CARTESIAN_POINT ( 'NONE',  ( -29.30121614929279161, -296.1526455479262268, -195.3638505560702470 ) ) ;
#81403 = ORIENTED_EDGE ( 'NONE', *, *, #32103, .F. ) ;
#81404 = FACE_OUTER_BOUND ( 'NONE', #18705, .T. ) ;
#81405 = CARTESIAN_POINT ( 'NONE',  ( 25.52912028483387630, -284.0775065495608942, -310.6943117138903858 ) ) ;
#81406 = CARTESIAN_POINT ( 'NONE',  ( -108.0307092747496966, -295.8155947024000056, -288.8782039335736158 ) ) ;
#81407 = CARTESIAN_POINT ( 'NONE',  ( 195.5881128153457098, -0.9999999999999991118, 22.50000000000000000 ) ) ;
#81408 = CARTESIAN_POINT ( 'NONE',  ( 31.95455697924147032, -279.4809262143061233, -303.7686719486574702 ) ) ;
#81409 = CARTESIAN_POINT ( 'NONE',  ( -21.37833918266614930, -273.4490437758136068, -195.1990934799911770 ) ) ;
#81410 = CARTESIAN_POINT ( 'NONE',  ( 33.59144544411675071, -289.2352063861476950, -299.1691354513337160 ) ) ;
#81411 = CARTESIAN_POINT ( 'NONE',  ( -106.5706182956691492, -290.6930563875704365, -247.2017377264558888 ) ) ;
#81412 = CARTESIAN_POINT ( 'NONE',  ( -65.09501091746756174, -281.2029266097997606, -202.0935452020635239 ) ) ;
#81413 = CARTESIAN_POINT ( 'NONE',  ( -35.38936557030753249, -275.6771580834642350, -196.5743010034133249 ) ) ;
#81414 = CARTESIAN_POINT ( 'NONE',  ( -6.589118888062201584, -279.2601040915910175, -203.7034982912537657 ) ) ;
#81415 = CARTESIAN_POINT ( 'NONE',  ( -6.666977479457773192, -278.6495834704358572, -338.8013257726720440 ) ) ;
#81416 = VERTEX_POINT ( 'NONE', #65390 ) ;
#81417 = CARTESIAN_POINT ( 'NONE',  ( -96.93472160949181671, -273.0403422845866999, -221.5791674555806878 ) ) ;
#81418 = CARTESIAN_POINT ( 'NONE',  ( 9.741089117532043318, -294.6257718584731720, -212.6355812249413191 ) ) ;
#81419 = CARTESIAN_POINT ( 'NONE',  ( 128.9467878515196162, -293.3047352414760667, -195.3611179825600175 ) ) ;
#81420 = LINE ( 'NONE', #67249, #8832 ) ;
#81421 = CARTESIAN_POINT ( 'NONE',  ( -3.845742125410460233, -290.6288506239876028, -202.3885421346880946 ) ) ;
#81422 = VECTOR ( 'NONE', #84057, 1000.000000000000000 ) ;
#81423 = CARTESIAN_POINT ( 'NONE',  ( -109.1890653965824640, -272.2382006614454895, -256.8262100058338433 ) ) ;
#81424 = DIRECTION ( 'NONE',  ( 0.000000000000000000, 1.000000000000000000, 0.000000000000000000 ) ) ;
#81425 = CARTESIAN_POINT ( 'NONE',  ( -99.29592239190790792, -291.4761780387928525, -314.9299009550358619 ) ) ;
#81426 = CARTESIAN_POINT ( 'NONE',  ( -69.85430415644619018, -285.9805209788416391, -337.9475929042657754 ) ) ;
#81427 = CARTESIAN_POINT ( 'NONE',  ( 12.33246085699259709, -288.7453289605854820, -214.3227204541045694 ) ) ;
#81428 = CARTESIAN_POINT ( 'NONE',  ( -4.278437262528261620, -274.6152354769872659, -337.5084252735588279 ) ) ;
#81429 = CARTESIAN_POINT ( 'NONE',  ( -1.041374552024579847, -276.4580071578250227, -205.3572902395208075 ) ) ;
#81430 = CARTESIAN_POINT ( 'NONE',  ( -75.70109231751027323, -289.6162094113578291, -206.5054070283297563 ) ) ;
#81431 = CARTESIAN_POINT ( 'NONE',  ( -83.82805160294078917, -281.2824061446086148, -210.4672535462808014 ) ) ;
#81432 =( BOUNDED_CURVE ( )  B_SPLINE_CURVE ( 3, ( #69772, #3976, #77344, #61740 ),
 .UNSPECIFIED., .F., .F. ) 
 B_SPLINE_CURVE_WITH_KNOTS ( ( 4, 4 ),
 ( 3.141592653589793116, 4.712388980384689674 ),
 .UNSPECIFIED. ) 
 CURVE ( )  GEOMETRIC_REPRESENTATION_ITEM ( )  RATIONAL_B_SPLINE_CURVE ( ( 1.000000000000000000, 0.8047378541243649375, 0.8047378541243649375, 1.000000000000000000 ) ) 
 REPRESENTATION_ITEM ( '' )  );
#81433 = VERTEX_POINT ( 'NONE', #503 ) ;
#81434 = CARTESIAN_POINT ( 'NONE',  ( -2.387209970727946384, -281.9253189169133407, -334.5788242504833647 ) ) ;
#81435 = CARTESIAN_POINT ( 'NONE',  ( -111.4359621981392507, -279.8811430163831915, -250.5231947129944956 ) ) ;
#81436 =( BOUNDED_SURFACE ( )  B_SPLINE_SURFACE ( 3, 2, ( 
 ( #50195, #28901, #57789 ),
 ( #53924, #53457, #82792 ),
 ( #10355, #40157, #45397 ),
 ( #9420, #60117, #23651 ) ),
 .UNSPECIFIED., .F., .F., .F. ) 
 B_SPLINE_SURFACE_WITH_KNOTS ( ( 4, 4 ),
 ( 3, 3 ),
 ( -1.728218262941894068E-16, 0.0009404805950306077342 ),
 ( 0.000000000000000000, 1.000000000000000000 ),
 .UNSPECIFIED. ) 
 GEOMETRIC_REPRESENTATION_ITEM ( )  RATIONAL_B_SPLINE_SURFACE ( (
 ( 1.000000000000000000, 0.6287211027134009811, 1.000000000000000000),
 ( 1.000000000000000000, 0.6575897825471116453, 1.000000000000000000),
 ( 1.000000000000000000, 0.6851250445827015145, 1.000000000000000000),
 ( 1.000000000000000000, 0.7071067811865358044, 1.000000000000000000) ) ) 
 REPRESENTATION_ITEM ( '' )  SURFACE ( )  );
#81437 = CARTESIAN_POINT ( 'NONE',  ( -5.633954510387108705, -281.4392521888790384, -340.0936612302977551 ) ) ;
#81438 = CARTESIAN_POINT ( 'NONE',  ( 5.749137854813886506, -277.4248127276291598, -333.8906378482966488 ) ) ;
#81439 = SHAPE_REPRESENTATION_RELATIONSHIP ( 'NONE' , 'NONE' ,  #67633, #29498 ) ;
#81440 = CARTESIAN_POINT ( 'NONE',  ( 38.45129827353991203, -277.1894236963454432, -279.6441618940204989 ) ) ;
#81441 = CARTESIAN_POINT ( 'NONE',  ( -6.941161984400275209, -291.1233781216987495, -333.4151289067050357 ) ) ;
#81442 = EDGE_LOOP ( 'NONE', ( #28623, #88570, #74365 ) ) ;
#81443 = ORIENTED_EDGE ( 'NONE', *, *, #40562, .F. ) ;
#81444 = CARTESIAN_POINT ( 'NONE',  ( -107.8591793374336589, -298.2193793707130567, -296.0535669861957899 ) ) ;
#81445 = CARTESIAN_POINT ( 'NONE',  ( -15.74752801627614396, -289.8459273966242904, -340.4707034162061063 ) ) ;
#81446 = CARTESIAN_POINT ( 'NONE',  ( -24.06118893897670574, -274.9019504825189415, -343.8676214626292449 ) ) ;
#81447 = CARTESIAN_POINT ( 'NONE',  ( -2.248520732216863660, -290.3542664703600167, -337.7587646469406195 ) ) ;
#81448 = CARTESIAN_POINT ( 'NONE',  ( -57.67534972201610799, -291.1312888155581504, -200.0911101867267234 ) ) ;
#81449 = CARTESIAN_POINT ( 'NONE',  ( 39.02868673217405160, -287.1819724656100448, -280.1216023615793347 ) ) ;
#81450 = CARTESIAN_POINT ( 'NONE',  ( 199.1087447750284980, 64.61450673763175701, 10.46317447812566570 ) ) ;
#81451 = CARTESIAN_POINT ( 'NONE',  ( -66.89848307319547871, -281.8459238038355466, -337.9975948380028399 ) ) ;
#81452 = CARTESIAN_POINT ( 'NONE',  ( -81.11709823628069671, -291.5139719558001161, -330.3798859420436429 ) ) ;
#81453 = CARTESIAN_POINT ( 'NONE',  ( -109.0355722145596928, -283.2554844095222393, -253.2570102271590144 ) ) ;
#81454 = CARTESIAN_POINT ( 'NONE',  ( 34.13366569337756573, -283.0921338086079686, -287.5177939692293307 ) ) ;
#81455 = CARTESIAN_POINT ( 'NONE',  ( 18.48196404994004993, -289.2151711512897805, -323.0539897076217812 ) ) ;
#81456 = CARTESIAN_POINT ( 'NONE',  ( -100.6330112341380953, -278.5432377405155648, -306.9620047640015059 ) ) ;
#81457 = CARTESIAN_POINT ( 'NONE',  ( -68.15489172491606951, -290.4513739081874064, -200.2144094642738708 ) ) ;
#81458 = CARTESIAN_POINT ( 'NONE',  ( -43.66319970291937835, -286.7771650855093526, -193.7299220376817743 ) ) ;
#81459 = CARTESIAN_POINT ( 'NONE',  ( 39.57839156035623063, -288.0234559837098232, -268.6799286120365764 ) ) ;
#81460 = CARTESIAN_POINT ( 'NONE',  ( -107.7605909859749431, -284.4640800756865815, -289.6483647304665396 ) ) ;
#81461 = ORIENTED_EDGE ( 'NONE', *, *, #78636, .T. ) ;
#81462 = PLANE ( 'NONE',  #2011 ) ;
#81463 = CARTESIAN_POINT ( 'NONE',  ( -61.32048074744731281, -293.6045735923605093, -198.4356701956213556 ) ) ;
#81464 = CARTESIAN_POINT ( 'NONE',  ( 37.28402649504832311, -292.0240855542635927, -253.4411470878083037 ) ) ;
#81465 = CARTESIAN_POINT ( 'NONE',  ( -78.77496429265643485, -276.6841147795372535, -330.8107311738360181 ) ) ;
#81466 = EDGE_CURVE ( 'NONE', #85835, #45114, #8515, .T. ) ;
#81467 = CARTESIAN_POINT ( 'NONE',  ( -51.77333915807633957, -297.2208882694891372, -194.7751326927263165 ) ) ;
#81468 = CARTESIAN_POINT ( 'NONE',  ( 33.41046195464509339, -292.3026504975281910, -291.0180623975079470 ) ) ;
#81469 = CARTESIAN_POINT ( 'NONE',  ( -105.9089854201567675, -294.4238561900944546, -298.2268926734060415 ) ) ;
#81470 = CARTESIAN_POINT ( 'NONE',  ( -105.0754000392019947, -292.1359803686528380, -241.9573154962923525 ) ) ;
#81471 = CARTESIAN_POINT ( 'NONE',  ( 35.95157311956521085, -294.6729113895875685, -273.4885028503704234 ) ) ;
#81472 = FACE_OUTER_BOUND ( 'NONE', #85546, .T. ) ;
#81473 = CARTESIAN_POINT ( 'NONE',  ( -39.09132017121444846, -293.0739058119107199, -345.5074236786803681 ) ) ;
#81474 = CARTESIAN_POINT ( 'NONE',  ( -75.36370812783209772, -299.5457771993484926, -205.6547606666991896 ) ) ;
#81475 = CARTESIAN_POINT ( 'NONE',  ( 32.54174415005469001, -288.7847564620081471, -292.4323337025993510 ) ) ;
#81476 = CARTESIAN_POINT ( 'NONE',  ( 35.30677965448295907, -277.7888002471546542, -290.4244152352820265 ) ) ;
#81477 = CARTESIAN_POINT ( 'NONE',  ( -88.58862666975814193, -278.0356210561185435, -213.5539811804669910 ) ) ;
#81478 = CARTESIAN_POINT ( 'NONE',  ( -1.341860430457181064, -273.8655115880363837, -202.4102215307920289 ) ) ;
#81479 = CARTESIAN_POINT ( 'NONE',  ( 36.46376833751075708, -279.5015557598004534, -260.2781165315608405 ) ) ;
#81480 = CARTESIAN_POINT ( 'NONE',  ( -73.73291075551577478, -275.9268137223404551, -337.3246045073453274 ) ) ;
#81481 = ADVANCED_FACE ( 'NONE', ( #38323 ), #61005, .F. ) ;
#81482 = CARTESIAN_POINT ( 'NONE',  ( -95.17179299640066859, -294.6017628289737900, -315.7144402254459123 ) ) ;
#81483 = CARTESIAN_POINT ( 'NONE',  ( -64.71025148262748417, -275.6949772249146235, -200.5193411917497031 ) ) ;
#81484 = CARTESIAN_POINT ( 'NONE',  ( -78.91985458104686302, -274.1268321491026541, -210.1735099633457651 ) ) ;
#81485 = AXIS2_PLACEMENT_3D ( 'NONE', #10114, #38980, #67893 ) ;
#81486 = CARTESIAN_POINT ( 'NONE',  ( 196.4644011024695658, 24.42492343596410365, 11.30625710096401093 ) ) ;
#81487 = CARTESIAN_POINT ( 'NONE',  ( -95.29734249440812732, -289.2342558586020687, -222.1794760285708037 ) ) ;
#81488 = CARTESIAN_POINT ( 'NONE',  ( -114.3688399610460635, -290.5772450426365481, -268.3547120787731046 ) ) ;
#81489 = CARTESIAN_POINT ( 'NONE',  ( -93.72847377785052458, -275.2416943149733584, -220.6563879686030702 ) ) ;
#81490 = CARTESIAN_POINT ( 'NONE',  ( -107.7198665985480233, -294.2197028883838925, -295.9486879867826019 ) ) ;
#81491 = CARTESIAN_POINT ( 'NONE',  ( -58.45222210322820899, -282.5153502516368462, -344.2981959699600907 ) ) ;
#81492 = DIRECTION ( 'NONE',  ( -0.000000000000000000, -0.000000000000000000, 1.000000000000000000 ) ) ;
#81493 = CARTESIAN_POINT ( 'NONE',  ( -67.50851954882334383, -281.4476789634111924, -339.0405383877470058 ) ) ;
#81494 = CARTESIAN_POINT ( 'NONE',  ( 129.4467878515196162, -299.5541904835127980, -195.3611179825600175 ) ) ;
#81495 = CARTESIAN_POINT ( 'NONE',  ( -109.0955318707426898, -289.5497042579262370, -254.9170855964073041 ) ) ;
#81496 = CARTESIAN_POINT ( 'NONE',  ( -89.78336789831863030, -281.9409037893129835, -322.9760100402969556 ) ) ;
#81497 = DIRECTION ( 'NONE',  ( 0.000000000000000000, 0.000000000000000000, 1.000000000000000000 ) ) ;
#81498 = LINE ( 'NONE', #60683, #83575 ) ;
#81499 = CARTESIAN_POINT ( 'NONE',  ( 33.41874587569338217, -291.8757249217769072, -295.3752671500746487 ) ) ;
#81500 = CARTESIAN_POINT ( 'NONE',  ( -87.62589355168771021, -279.3686623335170225, -324.3790807862029624 ) ) ;
#81501 = CARTESIAN_POINT ( 'NONE',  ( -104.0635800021767494, -285.2651340506965312, -308.1009423208942053 ) ) ;
#81503 = CARTESIAN_POINT ( 'NONE',  ( -33.23865699473719104, -286.1051135741359985, -197.4266971368483894 ) ) ;
#81502 = CARTESIAN_POINT ( 'NONE',  ( -49.46366225083603752, -271.9787532176643481, -195.7270078547863648 ) ) ;
#81504 = CARTESIAN_POINT ( 'NONE',  ( -3.581105182315538205, -278.0226648926341113, -335.7491684772039093 ) ) ;
#81505 = CARTESIAN_POINT ( 'NONE',  ( -37.80053278590420263, -277.8608422846659778, -343.5336368507983025 ) ) ;
#81506 = CARTESIAN_POINT ( 'NONE',  ( -100.8391223664173850, -287.0888725477194043, -230.4477365575937426 ) ) ;
#81507 = ORIENTED_EDGE ( 'NONE', *, *, #61310, .T. ) ;
#81508 = CARTESIAN_POINT ( 'NONE',  ( 123.4306832106270946, -134.2391364535880882, 0.000000000000000000 ) ) ;
#81509 = CARTESIAN_POINT ( 'NONE',  ( -74.60822251473014433, -295.3668414701115807, -337.8018845265034997 ) ) ;
#81510 = CARTESIAN_POINT ( 'NONE',  ( -44.20004833608461325, -287.9448798957060944, -196.0320532614270803 ) ) ;
#81511 = CARTESIAN_POINT ( 'NONE',  ( 196.1984952657759038, 25.39230566755399821, 14.04035613084743339 ) ) ;
#81512 = CARTESIAN_POINT ( 'NONE',  ( -115.3288506153726871, -294.2666405000204009, -252.5284128619063608 ) ) ;
#81513 = CARTESIAN_POINT ( 'NONE',  ( -113.7346718246339208, -277.5645414789357801, -263.0297439466132232 ) ) ;
#81514 = CARTESIAN_POINT ( 'NONE',  ( -66.68831987432899666, -290.0739243870403925, -200.0388858949283986 ) ) ;
#81515 = CARTESIAN_POINT ( 'NONE',  ( -98.69492629326609290, -286.6336142422166517, -229.5384601609094659 ) ) ;
#81516 = CARTESIAN_POINT ( 'NONE',  ( -81.91577897981534306, -281.1958574203101193, -211.2110024554951337 ) ) ;
#81517 = CARTESIAN_POINT ( 'NONE',  ( -52.07756747361237615, -287.2924948895428656, -195.3307418806546423 ) ) ;
#81518 = CARTESIAN_POINT ( 'NONE',  ( 24.24114958020114230, -284.1330263699405805, -313.1694497831790613 ) ) ;
#81519 = CARTESIAN_POINT ( 'NONE',  ( 37.90613039848756216, -275.9238673877632664, -286.7556407575713706 ) ) ;
#81520 = CARTESIAN_POINT ( 'NONE',  ( -89.25187456871118741, -295.3378472127571968, -216.6496211389093673 ) ) ;
#81521 = CARTESIAN_POINT ( 'NONE',  ( -107.4182413264988867, -278.7947956418959734, -238.3222776578252251 ) ) ;
#81522 = CARTESIAN_POINT ( 'NONE',  ( -99.66634836054889490, -299.0265852024221545, -229.5621137030160810 ) ) ;
#81523 = LINE ( 'NONE', #52191, #23337 ) ;
#81524 = DIRECTION ( 'NONE',  ( -0.000000000000000000, -0.000000000000000000, -1.000000000000000000 ) ) ;
#81525 = CARTESIAN_POINT ( 'NONE',  ( -110.8323744494958163, -271.0393599817121526, -250.8442989716325258 ) ) ;
#81526 = CARTESIAN_POINT ( 'NONE',  ( 142.6449502718966755, 15.36528803885690664, 22.50000000000000000 ) ) ;
#81527 = CARTESIAN_POINT ( 'NONE',  ( -39.16557828376275552, -276.5833071689592089, -343.3998878949193454 ) ) ;
#81528 = CARTESIAN_POINT ( 'NONE',  ( -24.24268197716851603, -275.4207735462100572, -194.8325718524619674 ) ) ;
#81529 = CARTESIAN_POINT ( 'NONE',  ( 24.90943393627685154, -281.2085776663339516, -315.3013132314085283 ) ) ;
#81530 = CARTESIAN_POINT ( 'NONE',  ( -37.24449393671535091, -290.8110606060461123, -344.3743908985322832 ) ) ;
#81531 = CARTESIAN_POINT ( 'NONE',  ( -23.53560918908046773, -299.7421508013676430, -194.0509510646687659 ) ) ;
#81532 = CARTESIAN_POINT ( 'NONE',  ( -66.75769995234024634, -296.6341364125992186, -341.1050666453737108 ) ) ;
#81533 = CARTESIAN_POINT ( 'NONE',  ( -66.05334213155849454, -293.6757415116455263, -201.2410391655178614 ) ) ;
#81534 = CARTESIAN_POINT ( 'NONE',  ( 35.09178510338133350, -279.7946907542589656, -289.2115230566017203 ) ) ;
#81535 = CARTESIAN_POINT ( 'NONE',  ( -11.26110028518248463, -282.3146674815915276, -200.5849068157895374 ) ) ;
#81536 = CARTESIAN_POINT ( 'NONE',  ( -72.32043912949114883, -295.6654774467655784, -204.6366580609269192 ) ) ;
#81537 = CARTESIAN_POINT ( 'NONE',  ( -93.34575983112711128, -286.8638263222467799, -218.6118593460829800 ) ) ;
#81538 = CARTESIAN_POINT ( 'NONE',  ( 10.30578182832529244, -287.2971193838337740, -326.1412745977937675 ) ) ;
#81539 = CARTESIAN_POINT ( 'NONE',  ( -38.25200987741680336, -140.4184747178956343, -364.5570500621696510 ) ) ;
#81540 = ORIENTED_EDGE ( 'NONE', *, *, #54222, .T. ) ;
#81541 = CARTESIAN_POINT ( 'NONE',  ( -70.40069959264657484, -288.0540586919979660, -339.2645996929285275 ) ) ;
#81542 = CARTESIAN_POINT ( 'NONE',  ( 35.57403419954985679, -287.1559421773070540, -265.5895491088462563 ) ) ;
#81543 = ORIENTED_EDGE ( 'NONE', *, *, #80738, .F. ) ;
#81544 = CARTESIAN_POINT ( 'NONE',  ( -110.3869172541948700, -285.3363969243524139, -293.7686626534448919 ) ) ;
#81545 = CARTESIAN_POINT ( 'NONE',  ( -6.523916385703952159, -274.8016836365604831, -204.1617849641908720 ) ) ;
#81546 = CARTESIAN_POINT ( 'NONE',  ( -36.36842439695983842, -290.9844209475647858, -193.6634243876421237 ) ) ;
#81547 = CARTESIAN_POINT ( 'NONE',  ( 15.68924443910203692, -282.9762888375470880, -326.0480258216661582 ) ) ;
#81548 = CARTESIAN_POINT ( 'NONE',  ( 5.776392461285563051, -282.1451928941652909, -207.4044833621010469 ) ) ;
#81549 = CARTESIAN_POINT ( 'NONE',  ( -70.45717404443072951, -283.8100457040980586, -339.8673710692067402 ) ) ;
#81551 = CARTESIAN_POINT ( 'NONE',  ( -91.29681870373481445, -279.2572502353401092, -221.1895288330605638 ) ) ;
#81550 = AXIS2_PLACEMENT_3D ( 'NONE', #37046, #2916, #65958 ) ;
#81552 = CARTESIAN_POINT ( 'NONE',  ( -37.37352853689063181, -274.5523547857346784, -345.3611179825600175 ) ) ;
#81553 = CARTESIAN_POINT ( 'NONE',  ( 122.3993579641739728, 149.2681047531912952, -263.6619803441950012 ) ) ;
#81554 = EDGE_LOOP ( 'NONE', ( #14547, #2400, #78216, #70299 ) ) ;
#81555 = CARTESIAN_POINT ( 'NONE',  ( 4.171787011464936690, -278.4913503194197233, -332.6239384301701421 ) ) ;
#81556 = CARTESIAN_POINT ( 'NONE',  ( -56.98314758917310030, -168.9463999539727013, -363.9601112268161387 ) ) ;
#81557 = CARTESIAN_POINT ( 'NONE',  ( -60.54039684088365192, -297.0918750966832249, -200.9843253510601357 ) ) ;
#81558 = CARTESIAN_POINT ( 'NONE',  ( 35.39649021963634823, -292.7416808081691784, -245.1262667562004935 ) ) ;
#81559 = CARTESIAN_POINT ( 'NONE',  ( 185.2856823005118372, 260.3293175957331869, -151.1391428729190523 ) ) ;
#81561 = CARTESIAN_POINT ( 'NONE',  ( -106.7922364318259270, -288.6231920933798847, -295.3223563613800025 ) ) ;
#81560 = CARTESIAN_POINT ( 'NONE',  ( 52.74161837482967741, -297.7338270766273922, -193.9716452598525223 ) ) ;
#81562 = CARTESIAN_POINT ( 'NONE',  ( -69.02332783173842756, -297.3336372524170770, -337.5103162485534085 ) ) ;
#81563 = CARTESIAN_POINT ( 'NONE',  ( -79.60648291651470743, -286.7832031638206445, -210.1743301218138527 ) ) ;
#81564 = ORIENTED_EDGE ( 'NONE', *, *, #60435, .F. ) ;
#81565 = CARTESIAN_POINT ( 'NONE',  ( -84.03256058658378436, -296.6170882930271659, -331.3607465515333956 ) ) ;
#81566 = CARTESIAN_POINT ( 'NONE',  ( -110.3800281877222034, -285.0011908244450751, -273.6471505607017889 ) ) ;
#81567 = CARTESIAN_POINT ( 'NONE',  ( -35.82243785402641834, -296.8657060230561342, -193.7584906295155918 ) ) ;
#81568 = CARTESIAN_POINT ( 'NONE',  ( -16.67988201711195728, -293.1153309467529766, -196.3526854063570397 ) ) ;
#81569 = CARTESIAN_POINT ( 'NONE',  ( 33.26543502597483126, -293.6547033828719009, -239.7970971671970517 ) ) ;
#81570 = CARTESIAN_POINT ( 'NONE',  ( -104.0468533493264118, -290.3181164821702396, -300.1410053159339668 ) ) ;
#81571 = ORIENTED_EDGE ( 'NONE', *, *, #66872, .T. ) ;
#81572 = DIRECTION ( 'NONE',  ( 0.000000000000000000, 0.000000000000000000, -1.000000000000000000 ) ) ;
#81573 = CARTESIAN_POINT ( 'NONE',  ( -57.09095328135572345, -299.6605900812083974, -197.1611648092674898 ) ) ;
#81574 = CARTESIAN_POINT ( 'NONE',  ( -46.81659624768673211, -272.7293088958181215, -194.3464150530818415 ) ) ;
#81575 = CARTESIAN_POINT ( 'NONE',  ( 34.80093529074917313, -280.4451696346272342, -257.7576024673706456 ) ) ;
#81576 = ORIENTED_EDGE ( 'NONE', *, *, #8605, .F. ) ;
#81577 = ORIENTED_EDGE ( 'NONE', *, *, #80835, .T. ) ;
#81578 = EDGE_CURVE ( 'NONE', #36174, #79410, #17115, .T. ) ;
#81579 = CARTESIAN_POINT ( 'NONE',  ( -80.19711561016082157, -277.1228843770078925, -334.3231448457644888 ) ) ;
#81580 = CARTESIAN_POINT ( 'NONE',  ( -89.79662402800906307, -271.6963692214894195, -218.4484858658417465 ) ) ;
#81581 = CARTESIAN_POINT ( 'NONE',  ( -69.07239738653603922, -281.4907108190378722, -203.2490599355635368 ) ) ;
#81582 = CARTESIAN_POINT ( 'NONE',  ( 30.26966211654734451, -274.0980063522423507, -301.0135105961224440 ) ) ;
#81583 = CARTESIAN_POINT ( 'NONE',  ( -65.74044477742103254, -298.8772838463473818, -202.6806790964819811 ) ) ;
#81584 = CARTESIAN_POINT ( 'NONE',  ( -65.91596933917897161, -274.6101130862098785, -202.9302675682357346 ) ) ;
#81585 = CARTESIAN_POINT ( 'NONE',  ( -37.27495885999479697, -299.6530978762457949, -194.1603388541626600 ) ) ;
#81586 = CARTESIAN_POINT ( 'NONE',  ( 24.00290855613504704, -272.9796924011017154, -226.5755129491877540 ) ) ;
#81587 = CARTESIAN_POINT ( 'NONE',  ( 32.44658160340369335, -294.4915137755492651, -292.1209066123664115 ) ) ;
#81588 = CARTESIAN_POINT ( 'NONE',  ( 25.35935763370303420, -291.5989863552330235, -231.7422419614223372 ) ) ;
#81589 = CARTESIAN_POINT ( 'NONE',  ( 211.4629471475955427, 32.98517505407394168, 10.00000000000000000 ) ) ;
#81590 = CARTESIAN_POINT ( 'NONE',  ( -72.80673558396618716, -278.0014665834356151, -338.6528785617550739 ) ) ;
#81591 = CARTESIAN_POINT ( 'NONE',  ( -40.77706564845924930, -274.1745594221836768, -197.3922959930540628 ) ) ;
#81592 = DIRECTION ( 'NONE',  ( -0.000000000000000000, -0.000000000000000000, 1.000000000000000000 ) ) ;
#81593 = CARTESIAN_POINT ( 'NONE',  ( -97.66598511725841547, -282.6042219454085966, -317.4172431457615176 ) ) ;
#81594 = CARTESIAN_POINT ( 'NONE',  ( -55.59971727143970810, -297.2867801675276382, -343.2766391937759067 ) ) ;
#81595 = DIRECTION ( 'NONE',  ( -0.000000000000000000, -0.000000000000000000, 1.000000000000000000 ) ) ;
#81596 = CARTESIAN_POINT ( 'NONE',  ( -37.27047264571911001, -285.2501954749469064, -197.1872097385394227 ) ) ;
#81597 = CARTESIAN_POINT ( 'NONE',  ( -22.12267351696975481, -280.8574611657795685, -343.9709655066067171 ) ) ;
#81598 = EDGE_CURVE ( 'NONE', #47569, #443, #67691, .T. ) ;
#81599 = CARTESIAN_POINT ( 'NONE',  ( -39.20543821871805790, -275.3157182006963239, -344.3509855061574285 ) ) ;
#81600 = CARTESIAN_POINT ( 'NONE',  ( 20.47421352498274061, -274.7641869881182402, -315.9082663212735156 ) ) ;
#81601 = CARTESIAN_POINT ( 'NONE',  ( -15.69785892337878508, -282.3322176857517434, -198.4986803509737570 ) ) ;
#81602 = CARTESIAN_POINT ( 'NONE',  ( 34.21747475951372053, -276.5424138334703912, -253.9827549142806902 ) ) ;
#81603 = DIRECTION ( 'NONE',  ( 0.000000000000000000, 0.000000000000000000, 1.000000000000000000 ) ) ;
#81604 = CARTESIAN_POINT ( 'NONE',  ( 194.3594574420116317, 20.00000000000002842, 14.58911678380875010 ) ) ;
#81605 = CARTESIAN_POINT ( 'NONE',  ( -52.36771837151059117, -272.2628353220592885, -195.6034358290793591 ) ) ;
#81606 = CARTESIAN_POINT ( 'NONE',  ( -104.5481009790185851, -280.9972328273689754, -236.5801782912776332 ) ) ;
#81607 = CARTESIAN_POINT ( 'NONE',  ( 165.2494399300530290, 8.542400036368780647, -9.000000000000001776 ) ) ;
#81608 = CARTESIAN_POINT ( 'NONE',  ( -31.02899395412981320, -288.0514537690238512, -195.0522291287576024 ) ) ;
#81609 = CARTESIAN_POINT ( 'NONE',  ( 52.66432107828247666, -260.8771019122912094, -472.6442049081569508 ) ) ;
#81610 = CARTESIAN_POINT ( 'NONE',  ( -94.42509389845753276, -289.2256952187570960, -221.6950631401307135 ) ) ;
#81611 = CARTESIAN_POINT ( 'NONE',  ( 82.12839394370399759, -301.1616880754598924, -196.5497600369658073 ) ) ;
#81612 = CARTESIAN_POINT ( 'NONE',  ( -97.51767341889299701, -294.7643033988899219, -312.3847154461004152 ) ) ;
#81613 = CARTESIAN_POINT ( 'NONE',  ( -47.13434429495616484, -290.0660109057705540, -196.7746409711008084 ) ) ;
#81614 = CARTESIAN_POINT ( 'NONE',  ( 168.8235619055982113, 230.3815547064285738, -190.2228674158758395 ) ) ;
#81615 = CARTESIAN_POINT ( 'NONE',  ( 209.5561215397301282, 38.04219307066034617, 12.07126757350762247 ) ) ;
#81616 = CARTESIAN_POINT ( 'NONE',  ( 39.00843874868931493, -286.0471595427563329, -271.5598921398479320 ) ) ;
#81617 = CARTESIAN_POINT ( 'NONE',  ( -92.70874832080957617, -282.0720905285465392, -322.4231050419248277 ) ) ;
#81618 = CARTESIAN_POINT ( 'NONE',  ( -46.99446503852924906, -291.9261271243483407, -198.0021231748401931 ) ) ;
#81619 = CARTESIAN_POINT ( 'NONE',  ( 36.15531568292917797, -283.0256259870450890, -274.0439949215377737 ) ) ;
#81620 = CARTESIAN_POINT ( 'NONE',  ( 33.48240068952684823, -282.5972305728804486, -288.7563043430086509 ) ) ;
#81621 = CARTESIAN_POINT ( 'NONE',  ( -5.015299507994749995, -290.6086075241711342, -338.4444515369659712 ) ) ;
#81622 = TOROIDAL_SURFACE ( 'NONE', #10588, 27.00000000000000355, 2.000000000000000000 ) ;
#81623 = CARTESIAN_POINT ( 'NONE',  ( -109.1484134547367404, -273.2385679935342750, -242.4737820105218589 ) ) ;
#81624 = CARTESIAN_POINT ( 'NONE',  ( -4.972541508331775439, -286.7091926481447217, -338.6508816839652809 ) ) ;
#81625 = CARTESIAN_POINT ( 'NONE',  ( 24.47987131220617840, -274.9418145528446757, -224.4580319789651242 ) ) ;
#81627 = CARTESIAN_POINT ( 'NONE',  ( -91.01617433687907521, -293.2650626749801859, -218.4872553857778144 ) ) ;
#81626 = CIRCLE ( 'NONE', #51416, 0.5000000000000004441 ) ;
#81628 = DIRECTION ( 'NONE',  ( -0.000000000000000000, -0.000000000000000000, -1.000000000000000000 ) ) ;
#81629 = CARTESIAN_POINT ( 'NONE',  ( 35.77081079830085031, -289.8376638359844719, -253.6410175316879361 ) ) ;
#81630 = CARTESIAN_POINT ( 'NONE',  ( -110.3001379511744773, -276.7843817808888502, -252.2226227578659916 ) ) ;
#81631 = CARTESIAN_POINT ( 'NONE',  ( 152.1970149279871976, 130.7370361098515446, -11.50000000000000000 ) ) ;
#81632 = CARTESIAN_POINT ( 'NONE',  ( -107.0330269614949827, -295.3508064804711353, -239.4158173966790173 ) ) ;
#81633 = CARTESIAN_POINT ( 'NONE',  ( -64.38351344228058792, -293.2934088378746083, -201.6802611414068451 ) ) ;
#81634 = CARTESIAN_POINT ( 'NONE',  ( -69.52837777310138279, -272.9654644204912870, -204.7264438328053018 ) ) ;
#81635 = CARTESIAN_POINT ( 'NONE',  ( -110.3900185015198758, -292.2043677344128128, -260.2530174932358591 ) ) ;
#81636 = CARTESIAN_POINT ( 'NONE',  ( -64.16892672441777279, -292.6346387786325636, -202.2027799395722241 ) ) ;
#81637 = CARTESIAN_POINT ( 'NONE',  ( -103.1494808854555032, -286.7664346686281647, -236.4891531330040664 ) ) ;
#81638 = CARTESIAN_POINT ( 'NONE',  ( 19.92496197988670303, -294.2868802007924387, -219.7534551073445073 ) ) ;
#81639 = CARTESIAN_POINT ( 'NONE',  ( -70.69793139008710625, -292.9365514218004023, -201.5086662383682210 ) ) ;
#81640 = CARTESIAN_POINT ( 'NONE',  ( -41.04134257427484300, -294.9332907131907859, -343.2798760160671350 ) ) ;
#81641 = CARTESIAN_POINT ( 'NONE',  ( 18.35936030458486812, -288.8521129955078663, -220.1185269631860706 ) ) ;
#81642 = CARTESIAN_POINT ( 'NONE',  ( 39.27833376018075029, -281.8208250199415943, -278.5164184276005130 ) ) ;
#81643 = CARTESIAN_POINT ( 'NONE',  ( -111.8491326714697180, -270.8700077986529209, -256.3356461168180545 ) ) ;
#81644 = CARTESIAN_POINT ( 'NONE',  ( -105.4311018208756394, -284.8510027319231881, -234.2909678048208661 ) ) ;
#81645 = CARTESIAN_POINT ( 'NONE',  ( 35.09946729279015187, -277.2997023367249199, -252.3576719530347816 ) ) ;
#81646 = CARTESIAN_POINT ( 'NONE',  ( -73.73927684388478099, -284.3523612073391860, -206.6100015843028643 ) ) ;
#81647 = CARTESIAN_POINT ( 'NONE',  ( 37.58122927918864065, -285.4955006632043819, -265.9617785773266405 ) ) ;
#81648 = CARTESIAN_POINT ( 'NONE',  ( -36.73820996776817083, -278.1992510171389199, -194.5858810721728958 ) ) ;
#81649 = CARTESIAN_POINT ( 'NONE',  ( 152.4536156746142410, 249.5000000000000568, -14.50000000000000000 ) ) ;
#81650 = CARTESIAN_POINT ( 'NONE',  ( -56.34093780218476866, -282.8113158081263236, -340.9090974665748490 ) ) ;
#81651 = CARTESIAN_POINT ( 'NONE',  ( -96.52052592055589741, -280.4141484921134975, -221.7004517271347197 ) ) ;
#81652 = CARTESIAN_POINT ( 'NONE',  ( 23.68170821781545499, -285.9878601338201065, -223.7674258250456489 ) ) ;
#81653 = CARTESIAN_POINT ( 'NONE',  ( 16.91705418887001144, -296.0258548913882350, -320.6995882996473028 ) ) ;
#81654 = CARTESIAN_POINT ( 'NONE',  ( -69.94008744300448654, -279.0744079446678825, -339.2505487498410162 ) ) ;
#81655 = CARTESIAN_POINT ( 'NONE',  ( 5.608361393400615569, -277.7986745285733718, -333.6745485249807075 ) ) ;
#81656 = CARTESIAN_POINT ( 'NONE',  ( -89.08731883574807853, -277.6379124203764945, -321.9245602074665840 ) ) ;
#81657 = CARTESIAN_POINT ( 'NONE',  ( -105.9001735268633553, -274.9215396830576879, -240.7074501944988469 ) ) ;
#81658 = CARTESIAN_POINT ( 'NONE',  ( 12.37051056494015100, -284.7456518831746735, -214.3564716067566849 ) ) ;
#81659 = CARTESIAN_POINT ( 'NONE',  ( -43.10128925807787681, -290.7238529822260489, -346.3431392017514554 ) ) ;
#81660 = CARTESIAN_POINT ( 'NONE',  ( -15.51384472010242810, -293.6833690411612565, -340.3985863505198495 ) ) ;
#81661 = EDGE_LOOP ( 'NONE', ( #90714, #78472, #61171, #9004 ) ) ;
#81662 = CARTESIAN_POINT ( 'NONE',  ( -6.759917655077732235, -294.3059758813359963, -336.6698057062560565 ) ) ;
#81663 = EDGE_LOOP ( 'NONE', ( #15815, #17251 ) ) ;
#81664 = CARTESIAN_POINT ( 'NONE',  ( -97.04075038563554756, -290.9836356689590389, -318.5224085003367236 ) ) ;
#81665 = CARTESIAN_POINT ( 'NONE',  ( -70.99596869006805377, -280.2472151768046160, -205.4526122486982445 ) ) ;
#81666 = EDGE_CURVE ( 'NONE', #89341, #10071, #74310, .T. ) ;
#81667 = CARTESIAN_POINT ( 'NONE',  ( -48.90973313567330649, -296.8285647415410722, -194.4942580596371045 ) ) ;
#81668 = CARTESIAN_POINT ( 'NONE',  ( 35.85327613079493858, -288.5004276563072949, -293.9367035957822623 ) ) ;
#81669 = CARTESIAN_POINT ( 'NONE',  ( -69.34464197355562476, -289.7951007624710655, -340.3866506129477330 ) ) ;
#81670 = CARTESIAN_POINT ( 'NONE',  ( -92.57233954507852047, -284.2048386811063665, -318.1469109438336318 ) ) ;
#81671 = CARTESIAN_POINT ( 'NONE',  ( 138.6539576904058606, 275.0000000000000568, 10.50000000000000000 ) ) ;
#81672 = CARTESIAN_POINT ( 'NONE',  ( 172.2203992884101069, 243.0707097176554043, -178.6047228861598910 ) ) ;
#81673 = CARTESIAN_POINT ( 'NONE',  ( -56.07279955880657951, -169.1889862642364051, -360.6176426954027079 ) ) ;
#81674 = CARTESIAN_POINT ( 'NONE',  ( -59.25307663538929859, -276.5403294896335638, -340.1643650859928698 ) ) ;
#81675 = CARTESIAN_POINT ( 'NONE',  ( -54.03763492351997400, -276.1917721815169671, -341.7960554523485825 ) ) ;
#81676 = CARTESIAN_POINT ( 'NONE',  ( 7.950400138221583646, -298.1126310072594947, -193.4263109806098839 ) ) ;
#81677 = CARTESIAN_POINT ( 'NONE',  ( -106.8441832117048875, -265.9836032479844334, -305.8845056521548713 ) ) ;
#81678 = CARTESIAN_POINT ( 'NONE',  ( -42.78788612005686076, -275.8043580061844864, -346.6738779317395256 ) ) ;
#81679 = CARTESIAN_POINT ( 'NONE',  ( -48.06382480049870054, -289.6844529238566679, -342.6826778869114491 ) ) ;
#81680 = CARTESIAN_POINT ( 'NONE',  ( -68.12218479301739649, -298.4611051804134263, -199.9004540013002895 ) ) ;
#81681 = CARTESIAN_POINT ( 'NONE',  ( 34.17715015035893344, -286.4586989024804211, -287.2814470124419586 ) ) ;
#81682 = CARTESIAN_POINT ( 'NONE',  ( 76.26758135708726627, -299.9312107013272453, -193.4133755750621617 ) ) ;
#81683 = CARTESIAN_POINT ( 'NONE',  ( -96.10158266802766036, -297.3261569210868629, -227.0240094179578421 ) ) ;
#81684 = VERTEX_POINT ( 'NONE', #23194 ) ;
#81685 = CARTESIAN_POINT ( 'NONE',  ( 199.4392256788250677, 65.82574266882504332, -7.741079165001071516 ) ) ;
#81686 = CARTESIAN_POINT ( 'NONE',  ( -64.55322078613674819, -279.3246348767544873, -340.9063943174588189 ) ) ;
#81687 = VECTOR ( 'NONE', #37181, 1000.000000000000000 ) ;
#81688 = CARTESIAN_POINT ( 'NONE',  ( -58.47586977684338194, -282.8257856576762492, -344.3954471951713003 ) ) ;
#81689 = CARTESIAN_POINT ( 'NONE',  ( -93.83548717843014231, -278.9720845331555097, -317.0999220533333869 ) ) ;
#81690 = CARTESIAN_POINT ( 'NONE',  ( -111.4189468759351342, -280.5268095417676477, -253.4337575196671821 ) ) ;
#81691 = VECTOR ( 'NONE', #86401, 1000.000000000000000 ) ;
#81692 = CARTESIAN_POINT ( 'NONE',  ( -39.16487771124121764, -296.6035876180735045, -196.7819657958442292 ) ) ;
#81693 = FACE_OUTER_BOUND ( 'NONE', #41869, .T. ) ;
#81694 = CARTESIAN_POINT ( 'NONE',  ( -38.35598725574979539, -280.2057721526154523, -197.3557639725252670 ) ) ;
#81695 = CARTESIAN_POINT ( 'NONE',  ( 38.57783508923524352, -276.5076616489199637, -282.5436712995240782 ) ) ;
#81696 = CARTESIAN_POINT ( 'NONE',  ( 24.43439190859696808, -278.1297590524230827, -312.9800392277856531 ) ) ;
#81697 = CARTESIAN_POINT ( 'NONE',  ( 38.73252060783467243, -274.0298001884705172, -262.6579311392850968 ) ) ;
#81698 = EDGE_LOOP ( 'NONE', ( #51037, #86686, #5891, #63223 ) ) ;
#81699 = DIRECTION ( 'NONE',  ( 1.000000000000000000, 0.000000000000000000, 0.000000000000000000 ) ) ;
#81700 = CARTESIAN_POINT ( 'NONE',  ( -107.1526404102343548, -290.0392534629336296, -248.4320811874937078 ) ) ;
#81701 = CARTESIAN_POINT ( 'NONE',  ( 5.130297916989874807, -285.9584118267812300, -206.1927601651087798 ) ) ;
#81702 = CARTESIAN_POINT ( 'NONE',  ( 10.54752895163773196, -280.6203346498940618, -326.8607211160672250 ) ) ;
#81704 = CARTESIAN_POINT ( 'NONE',  ( -37.25512277678583928, -284.1330549220610351, -195.9084808381126379 ) ) ;
#81703 = CARTESIAN_POINT ( 'NONE',  ( -33.48333667966325322, -281.5773931398748005, -343.8618043847972103 ) ) ;
#81705 = CARTESIAN_POINT ( 'NONE',  ( -108.8659954780599008, -292.2592040743076609, -293.0957207673508833 ) ) ;
#81706 = CARTESIAN_POINT ( 'NONE',  ( 13.59970718387610766, -281.9898080790516701, -217.4499471845261667 ) ) ;
#81707 = CARTESIAN_POINT ( 'NONE',  ( -112.1833100136661585, -270.6240362747285531, -264.7498312333518129 ) ) ;
#81708 = CARTESIAN_POINT ( 'NONE',  ( -30.30922140166665812, -281.3644661619290446, -346.2359139161668509 ) ) ;
#81709 = CARTESIAN_POINT ( 'NONE',  ( 30.43389058723382945, -295.9762457352487104, -302.5987744817679754 ) ) ;
#81710 = CARTESIAN_POINT ( 'NONE',  ( -112.3032331533630952, -276.6343661818296482, -282.8006750906004640 ) ) ;
#81711 = CARTESIAN_POINT ( 'NONE',  ( -63.92327072832434709, -287.7064970886273159, -200.0376239088250259 ) ) ;
#81712 = CARTESIAN_POINT ( 'NONE',  ( 153.6987871352777404, 19.48326534539592458, 11.45812909364015297 ) ) ;
#81713 = CARTESIAN_POINT ( 'NONE',  ( -105.9631163195439854, -292.8860414310746592, -238.6070255444787165 ) ) ;
#81714 = CARTESIAN_POINT ( 'NONE',  ( 35.52370789363173031, -273.7807801508527064, -288.1812025981160446 ) ) ;
#81715 = EDGE_CURVE ( 'NONE', #81225, #90630, #53408, .T. ) ;
#81716 = CARTESIAN_POINT ( 'NONE',  ( -62.71998869198446158, -288.5712730437087430, -342.9439427101294768 ) ) ;
#81717 = CARTESIAN_POINT ( 'NONE',  ( -17.19484027032354945, -290.7162995976032676, -199.3111526025095657 ) ) ;
#81718 = CARTESIAN_POINT ( 'NONE',  ( -48.18343439339133027, -274.8200403470382298, -436.8002545823482023 ) ) ;
#81719 = CARTESIAN_POINT ( 'NONE',  ( -51.39145209629101174, -275.9204033576540951, -342.4988192647832079 ) ) ;
#81720 = CARTESIAN_POINT ( 'NONE',  ( -111.4438894342690674, -294.7493514445453684, -265.9191569274854032 ) ) ;
#81721 = CARTESIAN_POINT ( 'NONE',  ( -88.99585677463919353, -291.1122554514721514, -322.6400963451912958 ) ) ;
#81722 = PRESENTATION_STYLE_ASSIGNMENT (( #66607 ) ) ;
#81723 = DIRECTION ( 'NONE',  ( 0.000000000000000000, 0.000000000000000000, 1.000000000000000000 ) ) ;
#81724 = CARTESIAN_POINT ( 'NONE',  ( 30.27890819409663337, -292.4923626002055244, -305.7187349992332770 ) ) ;
#81725 = CARTESIAN_POINT ( 'NONE',  ( 2.865992995962707734, -288.2018570862796309, -208.4758868868453305 ) ) ;
#81726 = CARTESIAN_POINT ( 'NONE',  ( 31.93176170945120163, -286.1962301827105080, -301.5886938793698278 ) ) ;
#81727 = CARTESIAN_POINT ( 'NONE',  ( 15.43957754999853194, -288.2419125267824711, -219.0823539217273606 ) ) ;
#81728 = EDGE_CURVE ( 'NONE', #21852, #63583, #37394, .T. ) ;
#81729 = DIRECTION ( 'NONE',  ( 0.000000000000000000, 1.000000000000000000, 0.000000000000000000 ) ) ;
#81730 = CARTESIAN_POINT ( 'NONE',  ( 28.95197012942375991, -287.9380140802033452, -239.4135654103442050 ) ) ;
#81731 = CARTESIAN_POINT ( 'NONE',  ( -22.39852171518658963, -296.8416151114992090, -344.2198224035504381 ) ) ;
#81732 = CARTESIAN_POINT ( 'NONE',  ( -74.94434090351494149, -212.1443419142231051, 25.50000000000000000 ) ) ;
#81733 = CARTESIAN_POINT ( 'NONE',  ( 24.37421298961141858, -288.1513152695231952, -224.9832071944996699 ) ) ;
#81734 = CARTESIAN_POINT ( 'NONE',  ( -26.01050746721648466, -274.9887816967616914, -345.0666617444682061 ) ) ;
#81735 = CARTESIAN_POINT ( 'NONE',  ( -25.76895742779925058, -277.2418540313242374, -346.4650989418158247 ) ) ;
#81736 = CARTESIAN_POINT ( 'NONE',  ( -94.94314872069300293, -278.9109482867825136, -219.2943243530987445 ) ) ;
#81737 = CARTESIAN_POINT ( 'NONE',  ( -106.2909426827863513, -298.9070820918510663, -241.7630629577626564 ) ) ;
#81738 = CARTESIAN_POINT ( 'NONE',  ( -97.35129869781235357, -283.1666775117235488, -225.3739116760270633 ) ) ;
#81739 = CARTESIAN_POINT ( 'NONE',  ( -48.18343439339132317, -257.8434817577606282, -488.9450021220059170 ) ) ;
#81740 = CARTESIAN_POINT ( 'NONE',  ( -77.46996165711199467, -277.6475204092960212, -207.8451630430427315 ) ) ;
#81741 = CARTESIAN_POINT ( 'NONE',  ( -19.42160838525141742, -280.8216104449914496, -343.2423238295277201 ) ) ;
#81742 = FACE_OUTER_BOUND ( 'NONE', #21373, .T. ) ;
#81743 = CARTESIAN_POINT ( 'NONE',  ( -23.08757232357777411, -275.3530328817878399, -345.3783213572709201 ) ) ;
#81744 = CARTESIAN_POINT ( 'NONE',  ( -109.1570256572031781, -298.2882931683211041, -253.8303353658724006 ) ) ;
#81745 = PRODUCT_RELATED_PRODUCT_CATEGORY ( 'part', '', ( #73213 ) ) ;
#81746 = CARTESIAN_POINT ( 'NONE',  ( -47.23017728899625922, -282.0953262108982358, -346.4118282267479572 ) ) ;
#81747 = CARTESIAN_POINT ( 'NONE',  ( -109.5097604275956797, -297.6572095929784609, -257.9040107300236286 ) ) ;
#81748 = CARTESIAN_POINT ( 'NONE',  ( -68.61960193026243360, -275.0743771140536751, -200.6309853788793589 ) ) ;
#81749 = CARTESIAN_POINT ( 'NONE',  ( -92.92712001049940795, -272.8924114127940470, -222.9883748504422840 ) ) ;
#81750 = CARTESIAN_POINT ( 'NONE',  ( 7.861940942577713365, -294.6698512480499517, -210.5143847409766806 ) ) ;
#81751 = CARTESIAN_POINT ( 'NONE',  ( 37.37631310072897861, -287.4860428834808772, -251.7541702567963000 ) ) ;
#81752 = CARTESIAN_POINT ( 'NONE',  ( -106.0984352063183991, -277.0416037779816634, -238.9011393139275583 ) ) ;
#81753 = CARTESIAN_POINT ( 'NONE',  ( -114.2514034051426108, -290.3388494518025595, -274.0890592805192227 ) ) ;
#81754 = CARTESIAN_POINT ( 'NONE',  ( -48.10737545686681926, -288.2510845727973106, -342.8519951788838966 ) ) ;
#81755 = CARTESIAN_POINT ( 'NONE',  ( 23.21506827447304744, -290.9489093193146232, -226.1131976733700526 ) ) ;
#81756 = EDGE_LOOP ( 'NONE', ( #17539, #28595, #16015, #63113 ) ) ;
#81757 = CARTESIAN_POINT ( 'NONE',  ( 193.6056169066500274, 279.7126221763799094, -126.0203154767880989 ) ) ;
#81758 = CARTESIAN_POINT ( 'NONE',  ( -98.34746959362136920, -290.6180054286815562, -230.0661910540931103 ) ) ;
#81759 = CARTESIAN_POINT ( 'NONE',  ( 41.08708295871279859, -296.0521521680024080, -472.6442049081569508 ) ) ;
#81760 = VECTOR ( 'NONE', #65512, 1000.000000000000227 ) ;
#81761 = CARTESIAN_POINT ( 'NONE',  ( -110.7047327889479362, -285.7801002085042228, -247.5837576834900062 ) ) ;
#81762 = CARTESIAN_POINT ( 'NONE',  ( -0.9049426016482470247, -291.5826589218674485, -202.7949806477763559 ) ) ;
#81763 = CARTESIAN_POINT ( 'NONE',  ( 37.94331977287701818, -283.0396546585653823, -284.0524904631643039 ) ) ;
#81764 = CARTESIAN_POINT ( 'NONE',  ( 1.099503359059319951, -282.3570541274576158, -332.4787756473494369 ) ) ;
#81765 = CARTESIAN_POINT ( 'NONE',  ( -113.3895472435426512, -296.7041695495339582, -258.2059314512890751 ) ) ;
#81766 = CARTESIAN_POINT ( 'NONE',  ( 28.29425190653734035, -276.4215915415323366, -237.2980679554437415 ) ) ;
#81767 = CARTESIAN_POINT ( 'NONE',  ( -22.38699921989589114, -290.2646919169902731, -197.2297039364170530 ) ) ;
#81768 = CARTESIAN_POINT ( 'NONE',  ( -31.29176557035528461, -272.9251503415742377, -197.2010906507908032 ) ) ;
#81769 = VERTEX_POINT ( 'NONE', #24118 ) ;
#81770 = FACE_OUTER_BOUND ( 'NONE', #28143, .T. ) ;
#81771 = CARTESIAN_POINT ( 'NONE',  ( -33.18217398097159077, -288.0249575611264845, -195.9866133404147206 ) ) ;
#81772 = CARTESIAN_POINT ( 'NONE',  ( -95.33868696863227399, -296.9512037699159350, -320.5392210541604072 ) ) ;
#81773 = CARTESIAN_POINT ( 'NONE',  ( -87.77080910989245410, -285.9760027947467051, -217.4385553528673825 ) ) ;
#81774 = CARTESIAN_POINT ( 'NONE',  ( -65.02145387072246763, -276.4636904490992038, -342.0178748278774492 ) ) ;
#81775 = CARTESIAN_POINT ( 'NONE',  ( 24.72726607723750547, -293.6000544971045088, -224.9655651053417955 ) ) ;
#81776 = CARTESIAN_POINT ( 'NONE',  ( 35.19584521420294720, -285.9713246467692329, -292.2832870148955067 ) ) ;
#81777 = CARTESIAN_POINT ( 'NONE',  ( -22.09758208446846695, -295.1952691141890455, -345.8154827105825007 ) ) ;
#81778 = CARTESIAN_POINT ( 'NONE',  ( -72.64089133273367338, -291.9046863170812003, -206.3820421999429300 ) ) ;
#81779 = DIRECTION ( 'NONE',  ( -1.000000000000000000, 0.000000000000000000, -0.000000000000000000 ) ) ;
#81780 = CARTESIAN_POINT ( 'NONE',  ( 196.7510731661265595, -142.7221692137691775, -22.50000000000000000 ) ) ;
#81781 = CARTESIAN_POINT ( 'NONE',  ( 193.8404912567452811, 275.6304219182297288, -124.1201750204255347 ) ) ;
#81782 = CARTESIAN_POINT ( 'NONE',  ( -110.4381947116660569, -285.7944235713907233, -292.3064571030392358 ) ) ;
#81783 = CARTESIAN_POINT ( 'NONE',  ( 44.71564893372296723, -279.0523547857346784, -270.3937649182068412 ) ) ;
#81784 = ORIENTED_EDGE ( 'NONE', *, *, #742, .T. ) ;
#81785 = ADVANCED_FACE ( 'NONE', ( #88518 ), #60594, .T. ) ;
#81786 = CARTESIAN_POINT ( 'NONE',  ( -107.6924227151188518, -283.2003506976758445, -291.0215416415543359 ) ) ;
#81787 = CARTESIAN_POINT ( 'NONE',  ( -113.7457979206378127, -278.0961323147606095, -280.1725934299769278 ) ) ;
#81788 = CARTESIAN_POINT ( 'NONE',  ( 16.56273339335434969, -282.8204410233846602, -218.3800833316968237 ) ) ;
#81789 = CARTESIAN_POINT ( 'NONE',  ( 105.0249005777022830, 114.6126997019200360, -281.5807060078374207 ) ) ;
#81790 = EDGE_CURVE ( 'NONE', #77618, #43923, #2819, .T. ) ;
#81791 = CARTESIAN_POINT ( 'NONE',  ( -33.10966586809888668, -281.5745935888664917, -346.6676397022843048 ) ) ;
#81792 = CARTESIAN_POINT ( 'NONE',  ( 30.31108749893536825, -285.1557371353844132, -238.8183355138148158 ) ) ;
#81793 = CARTESIAN_POINT ( 'NONE',  ( -80.56546497701046405, -275.3338081803476030, -208.0720400864513806 ) ) ;
#81794 = CARTESIAN_POINT ( 'NONE',  ( -105.0165476886413529, -296.6759819436445014, -297.8947964356850662 ) ) ;
#81795 = CARTESIAN_POINT ( 'NONE',  ( -36.18165813180068113, -290.7517847617235702, -196.8645606999143354 ) ) ;
#81796 = CARTESIAN_POINT ( 'NONE',  ( -114.2760003891828546, -279.2238068309048344, -268.7446783730263746 ) ) ;
#81797 = CARTESIAN_POINT ( 'NONE',  ( -3.867466406026852432, -276.5976231072189648, -335.2338832752563462 ) ) ;
#81798 = CARTESIAN_POINT ( 'NONE',  ( -106.5701162009084726, -274.0565483484143670, -237.3623465369909411 ) ) ;
#81799 = CARTESIAN_POINT ( 'NONE',  ( 39.32222630230873506, -274.4469488364879339, -268.3276743101127977 ) ) ;
#81800 = CARTESIAN_POINT ( 'NONE',  ( -114.0438498157189002, -273.6021558389782058, -270.3744870444270418 ) ) ;
#81801 = CARTESIAN_POINT ( 'NONE',  ( -1.969472082924502709, -274.5836062597261389, -336.5102494578166556 ) ) ;
#81802 = CARTESIAN_POINT ( 'NONE',  ( 0.2664318177568268387, -295.9867744330525738, -336.8911040734342350 ) ) ;
#81803 = DIRECTION ( 'NONE',  ( -0.000000000000000000, 0.000000000000000000, 1.000000000000000000 ) ) ;
#81804 = LINE ( 'NONE', #88450, #12499 ) ;
#81805 = CARTESIAN_POINT ( 'NONE',  ( -110.4027120996655498, -285.5526695175209966, -276.3872778473191829 ) ) ;
#81806 = CARTESIAN_POINT ( 'NONE',  ( -106.0793285600362594, -285.8918550963797998, -302.7511233675093081 ) ) ;
#81807 = CARTESIAN_POINT ( 'NONE',  ( 20.42629911730043801, -286.2706687486016790, -225.5643443071005265 ) ) ;
#81808 = CARTESIAN_POINT ( 'NONE',  ( -29.65008982035340068, -275.3531513455819777, -343.8106704035644725 ) ) ;
#81809 = CARTESIAN_POINT ( 'NONE',  ( 34.15537272895061705, -283.6721949639400009, -290.3369547551836831 ) ) ;
#81810 = CARTESIAN_POINT ( 'NONE',  ( -105.9200193510129537, -276.6746724043322274, -297.3374387780215784 ) ) ;
#81811 = CARTESIAN_POINT ( 'NONE',  ( 18.55297594529989524, -277.3034173617404008, -317.7954015868837701 ) ) ;
#81812 = DIRECTION ( 'NONE',  ( 0.000000000000000000, 0.000000000000000000, 1.000000000000000000 ) ) ;
#81813 = CARTESIAN_POINT ( 'NONE',  ( -56.88410069332447705, -274.2857279978143197, -199.9089025418762446 ) ) ;
#81814 = CARTESIAN_POINT ( 'NONE',  ( -3.737478874769393666, -281.2871097864644412, -201.2458706343960841 ) ) ;
#81815 = CARTESIAN_POINT ( 'NONE',  ( -31.08502114258416427, -280.6214083127929371, -193.6248278700684295 ) ) ;
#81816 = ORIENTED_EDGE ( 'NONE', *, *, #28179, .F. ) ;
#81817 = EDGE_LOOP ( 'NONE', ( #84340, #62402, #91597, #58198, #71729, #44037, #47488, #10995, #19958, #30714, #25524, #6203, #72608, #58276, #8682, #58741, #10590, #72387, #82730, #67233, #55982, #8567, #93127, #70890, #34895, #40116 ) ) ;
#81818 = CARTESIAN_POINT ( 'NONE',  ( 195.0811277904324754, 39.36132622696000283, 15.19607843137254477 ) ) ;
#81819 = CARTESIAN_POINT ( 'NONE',  ( -1.573939786598276491, -288.3815594679065839, -203.5706036674124562 ) ) ;
#81820 = CARTESIAN_POINT ( 'NONE',  ( -110.4034589047474810, -295.6990532250833894, -274.1796426937573301 ) ) ;
#81821 = CARTESIAN_POINT ( 'NONE',  ( -94.62982060207428958, -290.5975093576415134, -219.0641001426003811 ) ) ;
#81822 = CARTESIAN_POINT ( 'NONE',  ( 36.14165336782868820, -286.1130108396071137, -276.5587328561424556 ) ) ;
#81823 = CARTESIAN_POINT ( 'NONE',  ( -69.02800365246380920, -288.0520120069662084, -336.7791357795305771 ) ) ;
#81824 = CARTESIAN_POINT ( 'NONE',  ( -67.72600776497776565, -286.8493510531387756, -203.5485117216191782 ) ) ;
#81825 = CARTESIAN_POINT ( 'NONE',  ( -66.94330246224842540, -275.4399410940307007, -339.2722621481120200 ) ) ;
#81826 = CARTESIAN_POINT ( 'NONE',  ( -29.08433485324762202, -287.3491754652595773, -346.1653662221929721 ) ) ;
#81827 = CARTESIAN_POINT ( 'NONE',  ( 10.77445444981035827, -288.7170840278666901, -212.7621915810391044 ) ) ;
#81828 = CARTESIAN_POINT ( 'NONE',  ( 9.075335884246451101, -286.4169884501742445, -329.5499619058292069 ) ) ;
#81829 = AXIS2_PLACEMENT_3D ( 'NONE', #63620, #71170, #50778 ) ;
#81830 = CARTESIAN_POINT ( 'NONE',  ( 5.740147648839000638, -283.3931850303210354, -329.5841104735433760 ) ) ;
#81831 = CARTESIAN_POINT ( 'NONE',  ( -112.4188885866651333, -292.5053411525380511, -274.0277509019301760 ) ) ;
#81832 = CARTESIAN_POINT ( 'NONE',  ( 82.16616378849288083, -298.1952514025611549, -193.8821863655754782 ) ) ;
#81833 = CARTESIAN_POINT ( 'NONE',  ( 201.2104617360081704, 15.00000000000000000, -9.000000000000001776 ) ) ;
#81834 = CARTESIAN_POINT ( 'NONE',  ( -107.5596446376046345, -298.8346440975439577, -242.3142239576204702 ) ) ;
#81835 = CARTESIAN_POINT ( 'NONE',  ( -27.52661224193222012, -279.3770542723340213, -197.8097042457567625 ) ) ;
#81836 = CARTESIAN_POINT ( 'NONE',  ( 36.54158805151680411, -279.3864321950910607, -257.4669185781934289 ) ) ;
#81837 = CARTESIAN_POINT ( 'NONE',  ( 15.36048956961786693, -293.5269951826068677, -326.2774664076555382 ) ) ;
#81838 = CARTESIAN_POINT ( 'NONE',  ( -50.07210710525713893, -296.2868542674112291, -197.6673964413452893 ) ) ;
#81839 = CARTESIAN_POINT ( 'NONE',  ( 31.60265774430837027, -274.0023605277337992, -298.5693183149202810 ) ) ;
#81840 = CARTESIAN_POINT ( 'NONE',  ( -45.12643243768917500, -296.4678364360436831, -343.4916276328756339 ) ) ;
#81841 = DIRECTION ( 'NONE',  ( 0.000000000000000000, 1.000000000000000000, 0.000000000000000000 ) ) ;
#81842 = CARTESIAN_POINT ( 'NONE',  ( -94.63257186325374448, -271.8168149200270705, -219.8006362846780064 ) ) ;
#81843 = CARTESIAN_POINT ( 'NONE',  ( -112.1376571302561871, -294.9618256313630695, -256.9619078844593218 ) ) ;
#81844 = CARTESIAN_POINT ( 'NONE',  ( 13.29556812846294989, -294.2026951447872989, -216.9640957840976796 ) ) ;
#81845 = CARTESIAN_POINT ( 'NONE',  ( 175.2296996224750103, 249.5000000000000568, 24.50000000000000355 ) ) ;
#81846 = CARTESIAN_POINT ( 'NONE',  ( -1.185750365669597128, -293.3478312319411430, -206.7435534227670928 ) ) ;
#81847 = DIRECTION ( 'NONE',  ( -0.9437085149785860994, 0.3307782319877048405, 0.000000000000000000 ) ) ;
#81849 = CARTESIAN_POINT ( 'NONE',  ( -35.65061426688678381, -295.0303824265330945, -343.3540239828761287 ) ) ;
#81848 = CARTESIAN_POINT ( 'NONE',  ( -109.5395023486533148, -282.2949744204166223, -291.9903268073858840 ) ) ;
#81850 = CARTESIAN_POINT ( 'NONE',  ( -52.91761354190613531, -283.2463447877308909, -345.8237721711282120 ) ) ;
#81851 = CARTESIAN_POINT ( 'NONE',  ( 35.92879161800063059, -283.2369343717919605, -251.9017236092358587 ) ) ;
#81852 = CARTESIAN_POINT ( 'NONE',  ( -89.86871470747274770, -285.0017514214624157, -214.0155652234949173 ) ) ;
#81853 = CARTESIAN_POINT ( 'NONE',  ( -93.02061219355790911, -289.2502622922914952, -220.3430877252356765 ) ) ;
#81854 = CARTESIAN_POINT ( 'NONE',  ( 21.06670925402145045, -280.6992485220796993, -319.4647376872765108 ) ) ;
#81855 = CARTESIAN_POINT ( 'NONE',  ( -27.75575714261201199, -284.8612592378886461, -197.4958095402900256 ) ) ;
#81856 = ADVANCED_FACE ( 'NONE', ( #80480 ), #8971, .F. ) ;
#81857 = CARTESIAN_POINT ( 'NONE',  ( 39.04809207600354881, -286.3800592629153812, -263.0006598632234613 ) ) ;
#81858 = DIRECTION ( 'NONE',  ( 0.5068419345592596326, 0.000000000000000000, 0.8620390091940313138 ) ) ;
#81859 = CARTESIAN_POINT ( 'NONE',  ( 21.16980649560883876, -295.7785865678103505, -315.3578538571466083 ) ) ;
#81860 = CARTESIAN_POINT ( 'NONE',  ( -110.8685469066999048, -279.7147891454112028, -291.1555666755861580 ) ) ;
#81862 = CARTESIAN_POINT ( 'NONE',  ( -72.13604744183439266, -279.2451302517991962, -206.1626687658101389 ) ) ;
#81861 = CARTESIAN_POINT ( 'NONE',  ( 25.13367469356369099, -292.1395384917993852, -312.4946479065531548 ) ) ;
#81863 = CARTESIAN_POINT ( 'NONE',  ( 23.10675043577578691, -293.0806612251284946, -222.6432482840647822 ) ) ;
#81864 = CARTESIAN_POINT ( 'NONE',  ( -46.30986967815339028, -284.0190521048506866, -195.3352149116694250 ) ) ;
#81865 = CARTESIAN_POINT ( 'NONE',  ( -83.61196066571294239, -279.6866015623040198, -329.4530489213889837 ) ) ;
#81866 = CARTESIAN_POINT ( 'NONE',  ( -92.37538662734166905, -294.9233904793816805, -318.6798700241328106 ) ) ;
#81867 = CARTESIAN_POINT ( 'NONE',  ( -40.33426559960402358, -296.0145062507014586, -195.3700666537613131 ) ) ;
#81868 = ORIENTED_EDGE ( 'NONE', *, *, #59688, .F. ) ;
#81869 = DIRECTION ( 'NONE',  ( -1.000000000000000000, 0.000000000000000000, 0.000000000000000000 ) ) ;
#81870 = CARTESIAN_POINT ( 'NONE',  ( 25.04363643110249171, -282.9751916411251500, -229.2811638800966989 ) ) ;
#81871 = CARTESIAN_POINT ( 'NONE',  ( -110.1109977801522604, -296.1530367031302262, -263.2874672295286587 ) ) ;
#81872 = CARTESIAN_POINT ( 'NONE',  ( 194.5881128153456814, 6.505213034913026604E-16, 22.08578643762690419 ) ) ;
#81873 = CARTESIAN_POINT ( 'NONE',  ( -20.19161114001082069, -277.7666405000204009, -195.3683826091709363 ) ) ;
#81874 = CARTESIAN_POINT ( 'NONE',  ( -58.06820870452099115, -272.9882866742243550, -196.3154697137528615 ) ) ;
#81875 = CARTESIAN_POINT ( 'NONE',  ( 28.48799599358683921, -289.3784775099378521, -309.3450811002564933 ) ) ;
#81876 = CARTESIAN_POINT ( 'NONE',  ( -66.33098238309098349, -289.2757625204578744, -337.4123104797594692 ) ) ;
#81877 = CARTESIAN_POINT ( 'NONE',  ( -100.0679635560566538, -280.6017478704646919, -231.5839706051217206 ) ) ;
#81878 = CARTESIAN_POINT ( 'NONE',  ( -108.7190306916724722, -274.3995554054992567, -251.4108339425437748 ) ) ;
#81879 = CARTESIAN_POINT ( 'NONE',  ( -101.1494763215244888, -277.8411810278536791, -234.0885636033075912 ) ) ;
#81880 = ORIENTED_EDGE ( 'NONE', *, *, #67502, .F. ) ;
#81881 = CARTESIAN_POINT ( 'NONE',  ( 1.197259963528528148, -274.3852407785665832, -203.6843853388399452 ) ) ;
#81882 = CARTESIAN_POINT ( 'NONE',  ( -22.47650772332466929, -294.1641104950489307, -197.4204554565887690 ) ) ;
#81883 = DIRECTION ( 'NONE',  ( -0.000000000000000000, -1.000000000000000000, -0.000000000000000000 ) ) ;
#81884 = CARTESIAN_POINT ( 'NONE',  ( -108.8119729918828256, -291.4058927102275902, -255.0023170748712573 ) ) ;
#81885 = CARTESIAN_POINT ( 'NONE',  ( 175.2296996224750103, 214.5000000000000568, 0.000000000000000000 ) ) ;
#81886 = CARTESIAN_POINT ( 'NONE',  ( 12.48426344257400444, -290.8774155372340147, -213.2850386474827360 ) ) ;
#81888 = CARTESIAN_POINT ( 'NONE',  ( -93.62715280958242658, -296.8783414987095171, -223.8224746449104714 ) ) ;
#81887 = CONICAL_SURFACE ( 'NONE', #38088, 5.751884811727114410, 0.09862129276975223346 ) ;
#81889 = CARTESIAN_POINT ( 'NONE',  ( 154.1407330040854333, 250.0000000000000568, 13.42592592592592915 ) ) ;
#81890 = AXIS2_PLACEMENT_3D ( 'NONE', #11521, #4884, #84408 ) ;
#81891 = CARTESIAN_POINT ( 'NONE',  ( -95.14845873381477759, -292.7511371824128332, -220.5306347086738867 ) ) ;
#81892 = CARTESIAN_POINT ( 'NONE',  ( -37.37352853689063181, -288.5519495502701375, -190.3611179825600175 ) ) ;
#81893 = ADVANCED_FACE ( 'NONE', ( #58730 ), #31245, .F. ) ;
#81894 = CARTESIAN_POINT ( 'NONE',  ( 5.761052669849259011, -288.6375055859787722, -209.1243513350736123 ) ) ;
#81895 = CARTESIAN_POINT ( 'NONE',  ( -26.78750629475706191, -274.9174345947448614, -344.4464567279875382 ) ) ;
#81896 = CARTESIAN_POINT ( 'NONE',  ( 22.62701544133324205, -276.8663004806123809, -226.2582002445645912 ) ) ;
#81897 = CARTESIAN_POINT ( 'NONE',  ( -34.78378499846022720, -290.1643845635553589, -195.9650746031211952 ) ) ;
#81898 = CARTESIAN_POINT ( 'NONE',  ( -81.53784422453607306, -281.3181985650274441, -208.8224608222790266 ) ) ;
#81899 = EDGE_LOOP ( 'NONE', ( #39593, #44380 ) ) ;
#81900 = CARTESIAN_POINT ( 'NONE',  ( 25.64264714001457079, -281.4108975866635660, -307.5672530217617577 ) ) ;
#81901 = CARTESIAN_POINT ( 'NONE',  ( -112.6950455080724254, -279.8117695599299282, -256.0301802651289336 ) ) ;
#81902 = CARTESIAN_POINT ( 'NONE',  ( 29.40832813381082289, -280.8384585780484599, -308.0516618248084342 ) ) ;
#81903 = CARTESIAN_POINT ( 'NONE',  ( -11.93272297255542114, -277.6707218386073919, -342.8544650504663309 ) ) ;
#81905 = CARTESIAN_POINT ( 'NONE',  ( -34.15172917704009592, -275.6117045972064830, -194.1211557628172670 ) ) ;
#81904 = B_SPLINE_CURVE_WITH_KNOTS ( 'NONE', 3,
 ( #19554, #49379, #13411, #42254, #6296, #55557, #91979, #49831 ),
 .UNSPECIFIED., .F., .F.,
 ( 4, 2, 2, 4 ),
 ( 0.000000000000000000, 0.0002353609534302478071, 0.0004707219068604956143, 0.0009414438137210617017 ),
 .UNSPECIFIED. ) ;
#81906 = CARTESIAN_POINT ( 'NONE',  ( -37.30987171927208124, -279.5519495502701375, -340.3611179825599606 ) ) ;
#81907 = ORIENTED_EDGE ( 'NONE', *, *, #15556, .T. ) ;
#81908 = VERTEX_POINT ( 'NONE', #59191 ) ;
#81909 = CARTESIAN_POINT ( 'NONE',  ( -102.9768132442638802, -299.0350594075123922, -234.0701745892964709 ) ) ;
#81910 = CARTESIAN_POINT ( 'NONE',  ( -109.2392014585838638, -291.4429157286500640, -284.7422280120297842 ) ) ;
#81911 = CARTESIAN_POINT ( 'NONE',  ( 7.356775695287544714, -290.2126114348805004, -331.8753478756458435 ) ) ;
#81912 = CARTESIAN_POINT ( 'NONE',  ( -41.59047878508010854, -291.3459532735535049, -197.3328449412940984 ) ) ;
#81913 = CARTESIAN_POINT ( 'NONE',  ( 16.63830924949025913, -287.8171335449700337, -325.2593285999844284 ) ) ;
#81914 = CARTESIAN_POINT ( 'NONE',  ( -74.94434090351494149, -232.1443419142230766, 22.50000000000000000 ) ) ;
#81915 = CARTESIAN_POINT ( 'NONE',  ( -93.17760984515453515, -282.2717416064941744, -318.6379106467322231 ) ) ;
#81916 = CARTESIAN_POINT ( 'NONE',  ( -108.9103891702190907, -292.1541548040448220, -290.2680375753525936 ) ) ;
#81917 = CARTESIAN_POINT ( 'NONE',  ( -109.3381587566622386, -283.2382603741286289, -254.5791156361851222 ) ) ;
#81918 = CARTESIAN_POINT ( 'NONE',  ( 36.01104725288168851, -282.8078356335022363, -265.8204210585134888 ) ) ;
#81919 = CARTESIAN_POINT ( 'NONE',  ( 16.52940227328300082, -289.2505017365108415, -325.1225646238522131 ) ) ;
#81920 = CARTESIAN_POINT ( 'NONE',  ( -110.4129375776936826, -279.0767773678546746, -267.9124500087638125 ) ) ;
#81921 = CARTESIAN_POINT ( 'NONE',  ( -76.95074138161147914, -290.3293231260586822, -204.7321783276440215 ) ) ;
#81922 = CARTESIAN_POINT ( 'NONE',  ( -40.81941977351774398, -286.8124147291862300, -193.5492517992728665 ) ) ;
#81923 = CARTESIAN_POINT ( 'NONE',  ( 7.502970291046463736, -287.1378008828476709, -207.7776469902497070 ) ) ;
#81924 = CARTESIAN_POINT ( 'NONE',  ( -108.9293832670439741, -284.9073413963066628, -256.0711345212769174 ) ) ;
#81925 = ORIENTED_EDGE ( 'NONE', *, *, #909, .T. ) ;
#81926 = FACE_OUTER_BOUND ( 'NONE', #64879, .T. ) ;
#81927 = CARTESIAN_POINT ( 'NONE',  ( 31.06044012695905110, -294.9867342045036480, -237.6593316390317625 ) ) ;
#81928 = CARTESIAN_POINT ( 'NONE',  ( 38.36640547815856905, -292.0937119227294261, -258.9787496378156675 ) ) ;
#81929 = CARTESIAN_POINT ( 'NONE',  ( 5.524836989298125722, -275.5146758498975714, -329.8027580354513475 ) ) ;
#81930 = CARTESIAN_POINT ( 'NONE',  ( -35.46665834869380518, -297.4236408775723817, -193.4632510446849096 ) ) ;
#81931 = CARTESIAN_POINT ( 'NONE',  ( 25.00358950345557929, -292.5708276532235459, -309.7478065793825408 ) ) ;
#81932 = CARTESIAN_POINT ( 'NONE',  ( -84.70635495581396412, -295.6292443764529594, -213.4209975048893000 ) ) ;
#81933 = CARTESIAN_POINT ( 'NONE',  ( -108.1389300001882816, -292.0116532427509810, -250.9992289203728433 ) ) ;
#81934 = CARTESIAN_POINT ( 'NONE',  ( 21.23253139735124151, -294.0153737215701995, -226.2784062279527859 ) ) ;
#81935 = CARTESIAN_POINT ( 'NONE',  ( 207.9723288469463114, 36.44590423839540705, 14.83890152313991706 ) ) ;
#81936 = CARTESIAN_POINT ( 'NONE',  ( 20.85073852395589711, -292.2064657978497166, -317.9593404461119235 ) ) ;
#81937 = CARTESIAN_POINT ( 'NONE',  ( -84.48606600356380625, -299.4036879818700072, -211.9649669003583483 ) ) ;
#81938 = CARTESIAN_POINT ( 'NONE',  ( 35.89057345946819311, -288.5021574104857791, -271.0263642303369807 ) ) ;
#81939 = CARTESIAN_POINT ( 'NONE',  ( 33.65988051194787545, -277.8593400264110755, -295.7575412167898321 ) ) ;
#81940 = CARTESIAN_POINT ( 'NONE',  ( -93.05580144302479084, -276.6248595587082377, -323.0105112299098664 ) ) ;
#81941 = CARTESIAN_POINT ( 'NONE',  ( -68.79477288089572085, -272.9980274141841505, -200.1754024032130985 ) ) ;
#81942 = CARTESIAN_POINT ( 'NONE',  ( 19.57998248787507123, -280.3005101761426090, -318.3520991093543557 ) ) ;
#81943 = CARTESIAN_POINT ( 'NONE',  ( -105.6375096225134911, -276.5117870389955783, -304.2752045577215654 ) ) ;
#81944 = CARTESIAN_POINT ( 'NONE',  ( -110.8778073330106224, -295.2226525680596296, -271.4538477544599004 ) ) ;
#81945 = CARTESIAN_POINT ( 'NONE',  ( -111.5779681219408417, -274.6939240792844430, -259.3321695784418921 ) ) ;
#81946 = CARTESIAN_POINT ( 'NONE',  ( -76.62598443508069579, -274.1624624771984600, -208.7118059462517579 ) ) ;
#81947 = FACE_OUTER_BOUND ( 'NONE', #7511, .T. ) ;
#81948 = AXIS2_PLACEMENT_3D ( 'NONE', #52255, #89153, #30483 ) ;
#81950 = CARTESIAN_POINT ( 'NONE',  ( -48.87334312926287794, -273.7346232423334413, -198.2265123423171929 ) ) ;
#81949 = CARTESIAN_POINT ( 'NONE',  ( -100.2956681714494778, -289.1296890515407085, -228.8524962540716672 ) ) ;
#81951 = TOROIDAL_SURFACE ( 'NONE', #56310, 24.50000000000000355, 0.5000000000000000000 ) ;
#81952 = CARTESIAN_POINT ( 'NONE',  ( 39.57763484180127023, -287.4953391697130769, -265.8183967183750269 ) ) ;
#81953 = CARTESIAN_POINT ( 'NONE',  ( -106.4033990180104325, -274.9410280707010088, -240.5559909656385855 ) ) ;
#81954 = CARTESIAN_POINT ( 'NONE',  ( -73.02055219059077729, -293.5259162891216533, -336.1560482086745765 ) ) ;
#81955 = CARTESIAN_POINT ( 'NONE',  ( -52.89494398800645314, -282.4436414019826884, -345.6634568889118668 ) ) ;
#81956 = DIRECTION ( 'NONE',  ( 0.000000000000000000, 0.000000000000000000, 1.000000000000000000 ) ) ;
#81957 = CIRCLE ( 'NONE', #21502, 7.999911143031724237 ) ;
#81958 = CARTESIAN_POINT ( 'NONE',  ( 33.92109166633409245, -279.2480669793171728, -246.8177455318251248 ) ) ;
#81959 = DIRECTION ( 'NONE',  ( -0.000000000000000000, -1.000000000000000000, -0.000000000000000000 ) ) ;
#81960 = CARTESIAN_POINT ( 'NONE',  ( -88.19469969223784744, -290.1160943373806163, -217.3654477346387353 ) ) ;
#81961 = CARTESIAN_POINT ( 'NONE',  ( -69.56642910586073469, -281.6204821026560694, -337.2514034628729860 ) ) ;
#81962 = CARTESIAN_POINT ( 'NONE',  ( 200.1126601882107252, 214.5000000000000568, -2.416251949619908856 ) ) ;
#81963 = PRESENTATION_STYLE_ASSIGNMENT (( #24209 ) ) ;
#81964 = CARTESIAN_POINT ( 'NONE',  ( -111.1515960138788301, -288.3811207849422544, -283.6690073778734700 ) ) ;
#81965 = CARTESIAN_POINT ( 'NONE',  ( -81.50181328099357358, -274.9594527702330424, -211.3005300510968425 ) ) ;
#81966 = CARTESIAN_POINT ( 'NONE',  ( -50.01263738428759353, -284.4153233897258133, -345.9624212027071053 ) ) ;
#81968 = CARTESIAN_POINT ( 'NONE',  ( -91.66504558039827089, -283.8540456108374315, -319.1444035656863889 ) ) ;
#81967 = CARTESIAN_POINT ( 'NONE',  ( -1.953843752632816511, -272.5969758135981920, -203.6002475459519303 ) ) ;
#81969 = CARTESIAN_POINT ( 'NONE',  ( 22.95901602566664934, -277.5619691003940375, -312.6291777055037073 ) ) ;
#81970 = CARTESIAN_POINT ( 'NONE',  ( 32.25493520775901146, -276.6536211955946101, -292.9201533543655955 ) ) ;
#81971 = CARTESIAN_POINT ( 'NONE',  ( -52.48814562653897298, -285.2461834197364396, -343.8688423207035498 ) ) ;
#81972 = ORIENTED_EDGE ( 'NONE', *, *, #50919, .F. ) ;
#81973 = CARTESIAN_POINT ( 'NONE',  ( 156.4851178187871312, 15.00000000000000000, -7.000000000000000888 ) ) ;
#81974 = CARTESIAN_POINT ( 'NONE',  ( 23.17035501552031107, -294.0224567087636842, -317.9983529183751898 ) ) ;
#81975 = CARTESIAN_POINT ( 'NONE',  ( 36.62250982825553791, -289.3974439777578027, -259.9275491606242667 ) ) ;
#81976 = CARTESIAN_POINT ( 'NONE',  ( 123.4306832106270946, -134.2391364535880882, 0.000000000000000000 ) ) ;
#81977 = CARTESIAN_POINT ( 'NONE',  ( -72.02372285203398405, -295.1237833571632336, -198.2697987213421698 ) ) ;
#81978 = CARTESIAN_POINT ( 'NONE',  ( -99.98851142236988210, -278.0602045213016140, -226.1245997568183839 ) ) ;
#81979 = CARTESIAN_POINT ( 'NONE',  ( 1.312049252156952672, -290.9588973335400510, -204.6324907156576955 ) ) ;
#81980 = CARTESIAN_POINT ( 'NONE',  ( -46.83317061714643614, -287.4497245803039505, -197.2303155561596668 ) ) ;
#81981 =( BOUNDED_CURVE ( )  B_SPLINE_CURVE ( 3, ( #46015, #10030, #16220, #82473 ),
 .UNSPECIFIED., .F., .F. ) 
 B_SPLINE_CURVE_WITH_KNOTS ( ( 4, 4 ),
 ( 0.000000000000000000, 0.5235987755982975944 ),
 .UNSPECIFIED. ) 
 CURVE ( )  GEOMETRIC_REPRESENTATION_ITEM ( )  RATIONAL_B_SPLINE_CURVE ( ( 1.000000000000000000, 0.9772838841927122822, 0.9772838841927122822, 1.000000000000000000 ) ) 
 REPRESENTATION_ITEM ( '' )  );
#81982 = CARTESIAN_POINT ( 'NONE',  ( -91.69701426713092474, -279.5999645334164825, -320.6698298519895616 ) ) ;
#81983 = CARTESIAN_POINT ( 'NONE',  ( -43.63596989400259929, -287.3995043910445020, -194.1571762311504870 ) ) ;
#81984 = CARTESIAN_POINT ( 'NONE',  ( 28.62596424251758620, -284.0261726310041013, -306.0439976796699852 ) ) ;
#81985 = CARTESIAN_POINT ( 'NONE',  ( -6.572750981931142711, -276.8258589327974732, -340.9605836434483308 ) ) ;
#81986 = CARTESIAN_POINT ( 'NONE',  ( -106.0532071854996161, -270.9421275412298087, -240.5860623452868481 ) ) ;
#81987 = CARTESIAN_POINT ( 'NONE',  ( -113.2361289795359198, -278.5480729526414621, -257.3597459846866400 ) ) ;
#81988 =( BOUNDED_CURVE ( )  B_SPLINE_CURVE ( 3, ( #62304, #55672, #32009, #89754 ),
 .UNSPECIFIED., .F., .F. ) 
 B_SPLINE_CURVE_WITH_KNOTS ( ( 4, 4 ),
 ( 4.278565243615664038, 4.712388980384691450 ),
 .UNSPECIFIED. ) 
 CURVE ( )  GEOMETRIC_REPRESENTATION_ITEM ( )  RATIONAL_B_SPLINE_CURVE ( ( 1.000000000000000000, 0.9843778111405747655, 0.9843778111405747655, 1.000000000000000000 ) ) 
 REPRESENTATION_ITEM ( '' )  );
#81989 = CARTESIAN_POINT ( 'NONE',  ( -68.67552125017202513, -299.5572776468279130, -202.8230691811378961 ) ) ;
#81990 = CARTESIAN_POINT ( 'NONE',  ( 156.4677141125678475, 15.48129629386925643, 7.027845929950953696 ) ) ;
#81991 = EDGE_CURVE ( 'NONE', #44672, #44867, #7612, .T. ) ;
#81992 = CARTESIAN_POINT ( 'NONE',  ( -4.771743288812468897, -279.1233781216988064, -337.9199732462171255 ) ) ;
#81993 = CARTESIAN_POINT ( 'NONE',  ( -90.74778589981694665, -295.4440507633330526, -216.6201142531493247 ) ) ;
#81994 = LINE ( 'NONE', #23782, #22831 ) ;
#81995 = CARTESIAN_POINT ( 'NONE',  ( -92.77741965935388180, -277.3828267383703974, -317.9517624608558322 ) ) ;
#81996 = CARTESIAN_POINT ( 'NONE',  ( -67.39407707522751423, -274.8717218198938212, -199.8993314660514216 ) ) ;
#81997 = CARTESIAN_POINT ( 'NONE',  ( 27.65852530215709493, -280.0734236964347588, -229.4228801387190799 ) ) ;
#81998 = CARTESIAN_POINT ( 'NONE',  ( -5.334197129653129643, -290.3852100296180652, -337.0956200676806702 ) ) ;
#81999 = CARTESIAN_POINT ( 'NONE',  ( -102.5132835257025903, -297.5492595903598954, -310.0520800404493684 ) ) ;
#82000 = CARTESIAN_POINT ( 'NONE',  ( -113.8363059277430551, -297.6947739397306805, -275.3289945141840462 ) ) ;
#82001 = CARTESIAN_POINT ( 'NONE',  ( 31.53337820212854226, -295.1675051219065722, -240.9668696124453220 ) ) ;
#82002 = CARTESIAN_POINT ( 'NONE',  ( 37.39565679682894483, -279.6007446362789324, -274.1500365170583677 ) ) ;
#82003 = CARTESIAN_POINT ( 'NONE',  ( -41.14881242091294666, -281.9240118109325977, -196.0185319670774504 ) ) ;
#82004 = CARTESIAN_POINT ( 'NONE',  ( -39.17984955077309195, -296.1087858823657371, -195.9311581210084228 ) ) ;
#82005 = CARTESIAN_POINT ( 'NONE',  ( -113.5276546315382831, -286.1926276178770649, -267.1684642221741228 ) ) ;
#82006 = CARTESIAN_POINT ( 'NONE',  ( 33.69148388100780522, -286.2336494736513828, -252.1854886667417190 ) ) ;
#82007 = CARTESIAN_POINT ( 'NONE',  ( -98.09277876945984076, -248.9093811562096903, -333.9997278395424019 ) ) ;
#82008 = ORIENTED_EDGE ( 'NONE', *, *, #57977, .T. ) ;
#82009 = CARTESIAN_POINT ( 'NONE',  ( 29.83594339479149582, -286.6028097845501179, -306.8828598634932519 ) ) ;
#82010 = CARTESIAN_POINT ( 'NONE',  ( 17.79494098031452154, -286.5365691460364701, -222.4858812299608815 ) ) ;
#82011 = ORIENTED_EDGE ( 'NONE', *, *, #7720, .F. ) ;
#82012 = CARTESIAN_POINT ( 'NONE',  ( -111.9153293960401072, -285.4064035991736432, -288.3126544640929296 ) ) ;
#82013 = CARTESIAN_POINT ( 'NONE',  ( 11.55753433926364870, -275.0860068397330451, -216.0624895750014787 ) ) ;
#82014 = EDGE_CURVE ( 'NONE', #4883, #47327, #67070, .T. ) ;
#82015 = CARTESIAN_POINT ( 'NONE',  ( -66.88361849078992805, -290.5942973018921975, -199.5884709384627627 ) ) ;
#82016 = CARTESIAN_POINT ( 'NONE',  ( 38.04725899704824599, -282.3934068725969837, -285.5208550841853707 ) ) ;
#82017 = CARTESIAN_POINT ( 'NONE',  ( -88.48125708762592012, -280.8704605134516896, -213.7267338582360310 ) ) ;
#82018 = CARTESIAN_POINT ( 'NONE',  ( 39.59880616501320816, -281.9158260488990777, -272.7906823057586507 ) ) ;
#82019 = CARTESIAN_POINT ( 'NONE',  ( 7.142324975062856574, -280.6772154670964028, -212.4164943776545442 ) ) ;
#82020 = CARTESIAN_POINT ( 'NONE',  ( 30.89617123739170168, -291.2666405000203440, -285.9686137636504668 ) ) ;
#82021 = CARTESIAN_POINT ( 'NONE',  ( -113.3215480562446658, -274.3158145202488072, -270.3835736289650526 ) ) ;
#82022 = EDGE_LOOP ( 'NONE', ( #33313, #2764, #58350, #45293 ) ) ;
#82023 = CARTESIAN_POINT ( 'NONE',  ( 6.490750052572844098, -278.4556149095211026, -331.0777790653958732 ) ) ;
#82024 = CARTESIAN_POINT ( 'NONE',  ( -71.96233075983749927, -195.6174374264305413, -359.8130507035538130 ) ) ;
#82025 = CARTESIAN_POINT ( 'NONE',  ( 37.16309042514302519, -279.5132999550452837, -265.7913275264203321 ) ) ;
#82026 = CARTESIAN_POINT ( 'NONE',  ( -90.11371190002310527, -296.6304481117311980, -219.7020522695422073 ) ) ;
#82027 = CARTESIAN_POINT ( 'NONE',  ( 1.674307107433533837, -292.0664998206391374, -203.9882551612451209 ) ) ;
#82028 = CARTESIAN_POINT ( 'NONE',  ( 150.6539576904058606, 293.9636489450775230, 0.000000000000000000 ) ) ;
#82029 = VECTOR ( 'NONE', #37756, 1000.000000000000000 ) ;
#82031 = CARTESIAN_POINT ( 'NONE',  ( -110.4179503107032616, -288.8162978539924666, -280.7622457466610513 ) ) ;
#82030 = CARTESIAN_POINT ( 'NONE',  ( -40.39836935881152158, -296.5893015249340010, -193.9597787784593663 ) ) ;
#82032 = CARTESIAN_POINT ( 'NONE',  ( -108.7852277242770498, -298.1504164546531115, -290.5276210609516738 ) ) ;
#82033 = CARTESIAN_POINT ( 'NONE',  ( -8.073843208075505373, -287.7589408186571518, -202.9472022800918865 ) ) ;
#82034 = EDGE_LOOP ( 'NONE', ( #84213, #52013, #56790, #52695 ) ) ;
#82035 = CARTESIAN_POINT ( 'NONE',  ( 15.26815831641564003, -293.7144415564771407, -214.3862379636885862 ) ) ;
#82036 = CIRCLE ( 'NONE', #33649, 4.499999999999990230 ) ;
#82037 = CARTESIAN_POINT ( 'NONE',  ( -109.6740326450353393, -285.1802179702024205, -260.0644139302452231 ) ) ;
#82038 = CARTESIAN_POINT ( 'NONE',  ( -89.32751306955358928, -296.1348258943406222, -214.0266428071479652 ) ) ;
#82039 = CARTESIAN_POINT ( 'NONE',  ( -39.21801796046428024, -292.8320275124491445, -193.5324982138299390 ) ) ;
#82040 = CARTESIAN_POINT ( 'NONE',  ( -94.66964200860503809, -291.7410850516274081, -219.0480204045339008 ) ) ;
#82041 = CARTESIAN_POINT ( 'NONE',  ( -90.59130243329686039, -289.9995744522460654, -320.3696907042939301 ) ) ;
#82042 = EDGE_LOOP ( 'NONE', ( #37293, #36888, #7473, #10164 ) ) ;
#82043 = CARTESIAN_POINT ( 'NONE',  ( 157.4851178187871312, 15.28877977928702236, 6.999999999998999023 ) ) ;
#82044 = CARTESIAN_POINT ( 'NONE',  ( -94.65256039330974147, -299.0935287128514801, -220.7270525447967202 ) ) ;
#82045 = CARTESIAN_POINT ( 'NONE',  ( -96.61899181487805777, -272.0021148594323108, -221.8204370528361835 ) ) ;
#82046 = CARTESIAN_POINT ( 'NONE',  ( 34.56755605576303481, -280.4276044773031913, -256.4217376337435326 ) ) ;
#82047 = VERTEX_POINT ( 'NONE', #74797 ) ;
#82048 = CARTESIAN_POINT ( 'NONE',  ( -2.758393568358715964, -276.1149841649949508, -339.1036660766311002 ) ) ;
#82049 = CARTESIAN_POINT ( 'NONE',  ( -111.1417001269576730, -270.9522812833232024, -270.3407916626836709 ) ) ;
#82050 = CARTESIAN_POINT ( 'NONE',  ( -99.03308318034230240, -280.9775889039833601, -228.9776851961528621 ) ) ;
#82051 = CARTESIAN_POINT ( 'NONE',  ( -71.03423050132707317, -275.6412904287990386, -336.5100324117742048 ) ) ;
#82052 = CARTESIAN_POINT ( 'NONE',  ( -79.97106840304445541, -298.6658550758359638, -210.6127501027602875 ) ) ;
#82053 = CARTESIAN_POINT ( 'NONE',  ( 95.09830598555298309, -300.8281214179230574, -197.0271103297674813 ) ) ;
#82054 = CARTESIAN_POINT ( 'NONE',  ( -80.19216316353535490, -299.0830228283499537, -207.2875222114244025 ) ) ;
#82055 = CARTESIAN_POINT ( 'NONE',  ( 0.3940681800939942470, -272.5723212446074513, -205.1202525051882333 ) ) ;
#82056 = CARTESIAN_POINT ( 'NONE',  ( 21.07025797407371570, -293.5871847924900067, -226.4073261193454698 ) ) ;
#82057 = CARTESIAN_POINT ( 'NONE',  ( 23.08204006807817521, -291.5458836830696328, -228.3347825882860036 ) ) ;
#82058 = CARTESIAN_POINT ( 'NONE',  ( 193.8056763105550147, 214.8829733828359849, 16.96953521546779697 ) ) ;
#82059 = CARTESIAN_POINT ( 'NONE',  ( -31.44871836864349746, -277.4721050401014395, -347.1261470677173406 ) ) ;
#82060 = CARTESIAN_POINT ( 'NONE',  ( -56.86365599382574487, -273.9601132543831454, -199.9671383623970371 ) ) ;
#82061 = CARTESIAN_POINT ( 'NONE',  ( -3.128495950987585150, -281.2945866025168016, -338.8063339251074240 ) ) ;
#82062 = AXIS2_PLACEMENT_3D ( 'NONE', #73509, #24222, #39340 ) ;
#82063 = CARTESIAN_POINT ( 'NONE',  ( -27.95100427542504917, -296.9334926527635048, -344.9909090803030267 ) ) ;
#82064 = CARTESIAN_POINT ( 'NONE',  ( 208.4306832106271088, -142.7221692137691775, 0.000000000000000000 ) ) ;
#82065 = CARTESIAN_POINT ( 'NONE',  ( -61.59788182152129821, -282.5725472605432174, -339.4379448474290939 ) ) ;
#82066 = CARTESIAN_POINT ( 'NONE',  ( -95.76396267262362016, -281.9020240531446575, -317.6768880052978830 ) ) ;
#82067 = CARTESIAN_POINT ( 'NONE',  ( 16.01269113468555361, -274.8516610959954960, -321.0433027240094361 ) ) ;
#82068 = CARTESIAN_POINT ( 'NONE',  ( -2.946393120940041577, -282.5067821597840521, -203.6988334198388486 ) ) ;
#82069 = CARTESIAN_POINT ( 'NONE',  ( 154.1772290835186539, 20.65814982784575449, 13.49254024716540812 ) ) ;
#82070 = CARTESIAN_POINT ( 'NONE',  ( 160.6539576904058606, 293.9636489450775230, 0.000000000000000000 ) ) ;
#82071 = CARTESIAN_POINT ( 'NONE',  ( -49.57055690205050524, -272.2987273795579881, -195.0955372750555341 ) ) ;
#82072 = CARTESIAN_POINT ( 'NONE',  ( -110.9281324447398873, -280.7495242648145108, -254.9671001587985302 ) ) ;
#82073 = CARTESIAN_POINT ( 'NONE',  ( 165.0427047786672290, 215.0000000000000568, 23.37680765314704701 ) ) ;
#82074 = CARTESIAN_POINT ( 'NONE',  ( -1.671352019772091246, -288.4412879387947442, -203.7507549311218895 ) ) ;
#82075 = CARTESIAN_POINT ( 'NONE',  ( 157.9772837799833383, 17.93151222991821214, -10.94239627425337602 ) ) ;
#82076 = CARTESIAN_POINT ( 'NONE',  ( -104.7567830899720605, -288.1174226417805926, -303.3445663842726958 ) ) ;
#82077 = DIRECTION ( 'NONE',  ( -0.000000000000000000, -0.000000000000000000, -1.000000000000000000 ) ) ;
#82078 = CARTESIAN_POINT ( 'NONE',  ( -109.2769426472226684, -295.1550138320130259, -284.9994838495284739 ) ) ;
#82079 = CARTESIAN_POINT ( 'NONE',  ( 20.46059208423668707, -286.3393909041870415, -316.9418060296706585 ) ) ;
#82080 = CARTESIAN_POINT ( 'NONE',  ( 196.7445862410842778, 294.2657832282549748, -82.73034305482168804 ) ) ;
#82081 = CARTESIAN_POINT ( 'NONE',  ( -78.59127603965620779, -295.4969896299979268, -207.6610904924703220 ) ) ;
#82082 = CARTESIAN_POINT ( 'NONE',  ( 36.70872738699967641, -285.7995137569665189, -251.9425963325003863 ) ) ;
#82083 = CARTESIAN_POINT ( 'NONE',  ( 28.87780597464708876, -283.5903332957850580, -303.0565577872225163 ) ) ;
#82084 = CARTESIAN_POINT ( 'NONE',  ( -30.33099509431403717, -281.2044791313864494, -346.0236848713168456 ) ) ;
#82085 = CARTESIAN_POINT ( 'NONE',  ( -108.7105680981734679, -290.7545849382271967, -255.0156077379456292 ) ) ;
#82086 = AXIS2_PLACEMENT_3D ( 'NONE', #92792, #930, #87084 ) ;
#82087 = CARTESIAN_POINT ( 'NONE',  ( 23.07884904121814529, -283.5582309932527210, -312.3698332182628405 ) ) ;
#82088 = CARTESIAN_POINT ( 'NONE',  ( 32.38833408974344508, -282.6498862780698005, -292.6694504346328927 ) ) ;
#82089 = CARTESIAN_POINT ( 'NONE',  ( 22.00795887290809105, -290.1663917648011193, -316.8149171160421247 ) ) ;
#82090 = AXIS2_PLACEMENT_3D ( 'NONE', #20503, #42247, #5369 ) ;
#82091 = CARTESIAN_POINT ( 'NONE',  ( 7.986968146524043632, -298.7716743175183751, -193.3598638625616957 ) ) ;
#82092 = TOROIDAL_SURFACE ( 'NONE', #1948, 8.222204860432942297, 1.000000000000000000 ) ;
#82093 = CARTESIAN_POINT ( 'NONE',  ( 38.73575424438563886, -275.7049586598034239, -282.5794011309642997 ) ) ;
#82094 = CARTESIAN_POINT ( 'NONE',  ( -0.4655609963800500517, -294.5247008367717285, -205.4464179428558737 ) ) ;
#82095 = LINE ( 'NONE', #60809, #71188 ) ;
#82096 = CARTESIAN_POINT ( 'NONE',  ( -20.25526795762937127, -282.7662352645560304, -195.3538533559490702 ) ) ;
#82097 = VECTOR ( 'NONE', #3368, 1000.000000000000000 ) ;
#82098 = CARTESIAN_POINT ( 'NONE',  ( 33.46518172348125830, -273.8799286651936313, -295.7416329638515435 ) ) ;
#82099 = CARTESIAN_POINT ( 'NONE',  ( -23.40286736638519471, -134.2391364535880598, 22.50000000000000000 ) ) ;
#82100 = CARTESIAN_POINT ( 'NONE',  ( -109.0906698790647624, -295.2793660700268106, -244.6993613384723005 ) ) ;
#82101 = CARTESIAN_POINT ( 'NONE',  ( -68.15356948044015439, -293.2407799932713601, -203.2870407263492893 ) ) ;
#82102 = CARTESIAN_POINT ( 'NONE',  ( 0.6725464450685151307, -273.9222637228679105, -207.9206685476900986 ) ) ;
#82103 = VECTOR ( 'NONE', #45632, 1000.000000000000000 ) ;
#82104 = CARTESIAN_POINT ( 'NONE',  ( -69.33596237181502886, -293.1435359469183481, -203.9613785948843656 ) ) ;
#82105 = CARTESIAN_POINT ( 'NONE',  ( -44.33456818686888568, -292.9029330361613006, -197.4094620365269463 ) ) ;
#82106 = CARTESIAN_POINT ( 'NONE',  ( -111.2414875306717761, -286.3765952599508182, -265.4195759632858085 ) ) ;
#82107 = CARTESIAN_POINT ( 'NONE',  ( -112.0675905779172155, -292.1792724512033033, -254.3416348630592267 ) ) ;
#82108 = CARTESIAN_POINT ( 'NONE',  ( -6.103715620221827898, -293.7692909668433003, -200.5079179685447741 ) ) ;
#82109 = CARTESIAN_POINT ( 'NONE',  ( 20.52190693189797344, -294.0120640264001963, -314.8877966234297219 ) ) ;
#82110 = CARTESIAN_POINT ( 'NONE',  ( 34.58086250074265422, -289.2779139203096861, -249.0521506466539563 ) ) ;
#82111 = CARTESIAN_POINT ( 'NONE',  ( 6.926743768686855596, -282.6348991959138743, -333.4287393679612705 ) ) ;
#82112 = CARTESIAN_POINT ( 'NONE',  ( -32.01114943876781638, -296.1982380766883693, -194.8028378855136964 ) ) ;
#82113 = CARTESIAN_POINT ( 'NONE',  ( -111.4920438856211007, -284.1254119646054050, -291.1150700196210437 ) ) ;
#82114 = AXIS2_PLACEMENT_3D ( 'NONE', #82546, #47006, #22564 ) ;
#82115 = CARTESIAN_POINT ( 'NONE',  ( 35.50384725203758762, -277.7429538309397685, -286.7096000896301575 ) ) ;
#82116 = ADVANCED_FACE ( 'NONE', ( #88971 ), #12604, .T. ) ;
#82117 = CARTESIAN_POINT ( 'NONE',  ( -99.37480345308760832, -282.8067672581210559, -309.6866999271533132 ) ) ;
#82118 = CARTESIAN_POINT ( 'NONE',  ( 36.33050929770327997, -285.3715910787586267, -256.3109859636529109 ) ) ;
#82119 = CARTESIAN_POINT ( 'NONE',  ( -111.8552238822559701, -276.5165395997362339, -284.1452945737259483 ) ) ;
#82120 = CARTESIAN_POINT ( 'NONE',  ( 17.06571399127465583, -89.54582641780471874, 22.50000000000000000 ) ) ;
#82121 = CARTESIAN_POINT ( 'NONE',  ( -26.74003697949952496, -282.4214522944017745, -342.7007248049748682 ) ) ;
#82122 = AXIS2_PLACEMENT_3D ( 'NONE', #82208, #17363, #75118 ) ;
#82123 = CARTESIAN_POINT ( 'NONE',  ( -28.28724677181754643, -281.3695499766986927, -194.2418413332855209 ) ) ;
#82124 = CARTESIAN_POINT ( 'NONE',  ( 36.15663519833373840, -286.8903402198855588, -292.5610913724917168 ) ) ;
#82125 = CARTESIAN_POINT ( 'NONE',  ( -28.75648742360392873, -296.7021008025943161, -343.9265685650195223 ) ) ;
#82126 = CARTESIAN_POINT ( 'NONE',  ( 19.42611638585554346, -276.4548932462366793, -219.4519631878720531 ) ) ;
#82127 = CARTESIAN_POINT ( 'NONE',  ( -10.53619142669411879, -275.7096897475483388, -198.6475026056864124 ) ) ;
#82128 = CARTESIAN_POINT ( 'NONE',  ( -96.09426739027080089, -277.7779894194200665, -313.7079971486831482 ) ) ;
#82129 = CARTESIAN_POINT ( 'NONE',  ( -110.7518782995152691, -274.7100404944453658, -256.5640544879563549 ) ) ;
#82130 = CARTESIAN_POINT ( 'NONE',  ( 30.48204292126207449, -285.1354721065071658, -238.7388425717042537 ) ) ;
#82131 = CARTESIAN_POINT ( 'NONE',  ( -104.4417740241912327, -291.6804689559690473, -306.4723419537276072 ) ) ;
#82132 = AXIS2_PLACEMENT_3D ( 'NONE', #17023, #67237, #29847 ) ;
#82133 = CARTESIAN_POINT ( 'NONE',  ( 20.75981818490537378, -293.0992203979575379, -315.0855773402889781 ) ) ;
#82134 = ORIENTED_EDGE ( 'NONE', *, *, #11662, .F. ) ;
#82135 = CARTESIAN_POINT ( 'NONE',  ( -70.22643930907140941, -291.2730325280579677, -205.1638679189195216 ) ) ;
#82136 = VERTEX_POINT ( 'NONE', #10369 ) ;
#82137 = CARTESIAN_POINT ( 'NONE',  ( -62.64862278765789938, -290.4534736357731504, -342.8123836119005432 ) ) ;
#82138 = CARTESIAN_POINT ( 'NONE',  ( -109.7239409426571086, -279.3429944211504221, -259.7771122502529693 ) ) ;
#82139 = ADVANCED_FACE ( 'NONE', ( #53473 ), #17500, .F. ) ;
#82140 = CARTESIAN_POINT ( 'NONE',  ( -80.43990177356813831, -296.4036545708666495, -206.8619732081066900 ) ) ;
#82141 = CARTESIAN_POINT ( 'NONE',  ( 34.75577602402540123, -287.8649821034501315, -243.6166471730477099 ) ) ;
#82142 = CARTESIAN_POINT ( 'NONE',  ( 38.95374992914764789, -287.7573982976631441, -260.1264420195140588 ) ) ;
#82143 = CARTESIAN_POINT ( 'NONE',  ( -107.4110120342696604, -284.6130751241904022, -290.9576144652219796 ) ) ;
#82144 = CARTESIAN_POINT ( 'NONE',  ( -112.7898643569067900, -271.0197764341745597, -296.3298465391405330 ) ) ;
#82145 = CARTESIAN_POINT ( 'NONE',  ( 192.2886581304107096, 278.8240533624382351, -125.2388310753975418 ) ) ;
#82146 = CARTESIAN_POINT ( 'NONE',  ( 44.79179776835351845, 11.33544171671844580, -328.3433051430387195 ) ) ;
#82147 = ADVANCED_FACE ( 'NONE', ( #15630 ), #17956, .T. ) ;
#82148 = CARTESIAN_POINT ( 'NONE',  ( -80.92374628910054923, -276.8584106975106920, -329.1251118808432352 ) ) ;
#82149 = CARTESIAN_POINT ( 'NONE',  ( -108.2681701242387220, -277.7167875131541450, -251.7737250035820864 ) ) ;
#82150 = CARTESIAN_POINT ( 'NONE',  ( -26.21448397584709156, -297.6956243422372950, -193.4235562049308612 ) ) ;
#82151 = CARTESIAN_POINT ( 'NONE',  ( 202.7398265782193221, 290.0209625311386503, -82.55066922910880578 ) ) ;
#82152 = CARTESIAN_POINT ( 'NONE',  ( -8.088789376390691288, -275.3617651508644713, -341.0687710340085346 ) ) ;
#82153 = ORIENTED_EDGE ( 'NONE', *, *, #66952, .T. ) ;
#82154 = CARTESIAN_POINT ( 'NONE',  ( -108.9978554447150003, -290.8556865092985504, -284.6863532519028013 ) ) ;
#82155 = CARTESIAN_POINT ( 'NONE',  ( -37.26403528140092902, -298.8559311974310617, -193.5218205314156137 ) ) ;
#82156 = CARTESIAN_POINT ( 'NONE',  ( 34.19417533085546523, -286.0154989581392329, -253.4584735647162290 ) ) ;
#82157 = CARTESIAN_POINT ( 'NONE',  ( -83.52550538733954966, -274.0891177587608354, -208.8097631244746140 ) ) ;
#82158 = CARTESIAN_POINT ( 'NONE',  ( -47.79093832560312194, -295.3552761443186228, -342.6606740253980661 ) ) ;
#82159 = ORIENTED_EDGE ( 'NONE', *, *, #44158, .T. ) ;
#82160 = CARTESIAN_POINT ( 'NONE',  ( -106.2525905069612833, -280.0674473281030714, -301.4819427822596367 ) ) ;
#82161 = CARTESIAN_POINT ( 'NONE',  ( 25.05370473753441374, -281.6574099407159224, -315.3983698282480077 ) ) ;
#82162 = CIRCLE ( 'NONE', #20202, 1.000000000000007105 ) ;
#82163 = AXIS2_PLACEMENT_3D ( 'NONE', #66356, #44554, #1937 ) ;
#82164 = CARTESIAN_POINT ( 'NONE',  ( -110.7012053438168380, -279.6279966159377750, -270.6529480603770139 ) ) ;
#82165 = CARTESIAN_POINT ( 'NONE',  ( -112.0047537040155845, -280.4921293873322838, -256.1704305727635642 ) ) ;
#82166 = CARTESIAN_POINT ( 'NONE',  ( -82.28978495796707193, -296.0000757693032369, -212.0295361154890941 ) ) ;
#82167 = CARTESIAN_POINT ( 'NONE',  ( 198.6884013828325521, 64.61450673763174279, -9.555809373750800972 ) ) ;
#82168 = CARTESIAN_POINT ( 'NONE',  ( -94.79217245488219135, -279.3540500217516751, -225.3027557184658463 ) ) ;
#82169 = CIRCLE ( 'NONE', #41335, 24.00000000000000355 ) ;
#82170 = CARTESIAN_POINT ( 'NONE',  ( -2.639636848006202907, -275.3020532080696512, -201.7904432705693694 ) ) ;
#82171 = CARTESIAN_POINT ( 'NONE',  ( 37.62171321351074482, -286.4294392609133979, -285.6511452717745101 ) ) ;
#82172 = CARTESIAN_POINT ( 'NONE',  ( -4.719667921906985697, -276.4819619247717242, -202.8132667201391826 ) ) ;
#82173 = CARTESIAN_POINT ( 'NONE',  ( 30.01501722445966536, -274.5980689000616053, -306.5515775254915525 ) ) ;
#82174 = CARTESIAN_POINT ( 'NONE',  ( 197.2644541368101159, 214.9596432740807757, -12.42446933126076480 ) ) ;
#82175 = CIRCLE ( 'NONE', #15691, 24.00000000000001066 ) ;
#82176 = CARTESIAN_POINT ( 'NONE',  ( -110.4681864251881507, -289.7026469068417214, -273.9066104233913848 ) ) ;
#82177 = CARTESIAN_POINT ( 'NONE',  ( -102.8356115009131031, -283.3733664604519049, -310.6582687441062944 ) ) ;
#82178 = CARTESIAN_POINT ( 'NONE',  ( 8.402911710312698901, -280.6563475136866259, -328.6107861503588765 ) ) ;
#82180 = CARTESIAN_POINT ( 'NONE',  ( -46.88573168073287434, -284.0100027414964075, -196.4836983738666163 ) ) ;
#82179 = CARTESIAN_POINT ( 'NONE',  ( -4.065012856411942543, -279.0745545272598633, -204.7114752265621291 ) ) ;
#82181 = CARTESIAN_POINT ( 'NONE',  ( -16.17990006150293780, -290.7788601638627028, -342.3672611418575116 ) ) ;
#82182 = CARTESIAN_POINT ( 'NONE',  ( -49.22120863500471444, -281.1024542151716901, -197.9317884155463503 ) ) ;
#82183 = CARTESIAN_POINT ( 'NONE',  ( -101.0074826914384971, -271.0844958151715218, -230.7168399829901091 ) ) ;
#82184 = CARTESIAN_POINT ( 'NONE',  ( -31.71589676564785165, -281.3821648384673608, -346.3662920569153698 ) ) ;
#82185 = CARTESIAN_POINT ( 'NONE',  ( 36.84216627480963524, -295.6939918879463676, -281.3953653382101834 ) ) ;
#82187 = CARTESIAN_POINT ( 'NONE',  ( -106.4875885432006726, -277.2015908731663103, -238.7254681870155082 ) ) ;
#82186 = VECTOR ( 'NONE', #64345, 1000.000000000000000 ) ;
#82188 = CARTESIAN_POINT ( 'NONE',  ( -107.9165083132562586, -278.9522213974703391, -289.4160154648022854 ) ) ;
#82189 = CARTESIAN_POINT ( 'NONE',  ( -67.13079451278326815, -285.4419288387170468, -339.3729885893371261 ) ) ;
#82190 = CARTESIAN_POINT ( 'NONE',  ( 153.4178427586908811, 19.62198520651892863, 10.83765028963029842 ) ) ;
#82191 = CARTESIAN_POINT ( 'NONE',  ( -93.65474649989067757, -293.1686613232927243, -219.9810127070461476 ) ) ;
#82192 = CARTESIAN_POINT ( 'NONE',  ( -32.31117604997904635, -274.9886833389989533, -345.2435600996745961 ) ) ;
#82193 = CARTESIAN_POINT ( 'NONE',  ( 36.22782511701549879, -287.0287372871783305, -292.5807393657402145 ) ) ;
#82194 = CARTESIAN_POINT ( 'NONE',  ( -34.80964736120277792, -290.4843585089363955, -196.6045648799531875 ) ) ;
#82195 = CARTESIAN_POINT ( 'NONE',  ( -43.37475307536850266, -265.5729591849662938, -435.3257326888780199 ) ) ;
#82196 = CARTESIAN_POINT ( 'NONE',  ( 34.06169929642377525, -274.4656557973740405, -287.8151726627178846 ) ) ;
#82197 = CARTESIAN_POINT ( 'NONE',  ( -64.03490053994069342, -293.5434939620507748, -339.6856312753361635 ) ) ;
#82198 = CARTESIAN_POINT ( 'NONE',  ( -105.5646293371883360, -291.5023805375322468, -297.8266441504850945 ) ) ;
#82199 = CARTESIAN_POINT ( 'NONE',  ( 2.197429475817664013, -229.5268262511776527, 21.50000000000000000 ) ) ;
#82200 = CARTESIAN_POINT ( 'NONE',  ( 38.53885564606073189, -291.9242801084453163, -261.8229028761807058 ) ) ;
#82201 = CARTESIAN_POINT ( 'NONE',  ( -104.2189597646516432, -286.5705348472563401, -239.0329722847220637 ) ) ;
#82202 = CARTESIAN_POINT ( 'NONE',  ( -26.31405430414769242, -287.1534919365759038, -345.5433302373552351 ) ) ;
#82203 = EDGE_CURVE ( 'NONE', #75996, #64501, #70019, .T. ) ;
#82204 = CARTESIAN_POINT ( 'NONE',  ( 31.51959912646978879, -288.6321722757145380, -244.2655592401592344 ) ) ;
#82205 = PLANE ( 'NONE',  #87905 ) ;
#82206 = CARTESIAN_POINT ( 'NONE',  ( 16.08541515327904392, -287.6373231571927249, -220.3611861522408901 ) ) ;
#82207 = CARTESIAN_POINT ( 'NONE',  ( -55.64582352358044659, -297.2665151344614856, -343.4594481038606659 ) ) ;
#82208 = CARTESIAN_POINT ( 'NONE',  ( 175.2296996224750103, 250.5000000000000568, 0.000000000000000000 ) ) ;
#82209 = CARTESIAN_POINT ( 'NONE',  ( -32.34771155020516886, -287.3188496449234890, -193.9080509642015215 ) ) ;
#82210 = CARTESIAN_POINT ( 'NONE',  ( -64.59887507751042790, -275.4849463048752796, -340.8887702656103897 ) ) ;
#82211 = CARTESIAN_POINT ( 'NONE',  ( -93.31570017795620231, -278.1629683249696541, -323.2831854781044854 ) ) ;
#82212 = ORIENTED_EDGE ( 'NONE', *, *, #90310, .F. ) ;
#82213 = CARTESIAN_POINT ( 'NONE',  ( 1.367014395040615948, -280.2208655637672905, -203.7618696849826563 ) ) ;
#82214 = CARTESIAN_POINT ( 'NONE',  ( -110.0855082842366102, -298.7479889569253828, -253.6223849895250453 ) ) ;
#82215 = CARTESIAN_POINT ( 'NONE',  ( -102.7226632636031525, -283.0426510472877339, -233.5079086041955634 ) ) ;
#82216 = CARTESIAN_POINT ( 'NONE',  ( 193.9535050655732675, 215.0000000000000568, 17.26454883540666430 ) ) ;
#82217 = CARTESIAN_POINT ( 'NONE',  ( -57.42499831240692743, -277.9297467150012153, -198.8941563019513126 ) ) ;
#82218 = CARTESIAN_POINT ( 'NONE',  ( -69.63273108474551520, -281.4769820148094936, -338.0678196151921497 ) ) ;
#82219 = FACE_OUTER_BOUND ( 'NONE', #14667, .T. ) ;
#82220 = CARTESIAN_POINT ( 'NONE',  ( -28.69896665040271344, -275.4244658673873687, -346.2298475127841471 ) ) ;
#82221 = CARTESIAN_POINT ( 'NONE',  ( -101.8305640059499666, -298.5550981857519446, -234.6974924434329353 ) ) ;
#82222 = CARTESIAN_POINT ( 'NONE',  ( -38.74074939013102181, -281.9896487476350444, -347.0392450602047916 ) ) ;
#82223 = CARTESIAN_POINT ( 'NONE',  ( -104.9841060373679795, -297.8686091136740970, -242.2913233571277374 ) ) ;
#82224 = CARTESIAN_POINT ( 'NONE',  ( -109.3921034050367922, -298.1941986321468789, -244.6310254897033190 ) ) ;
#82225 = CARTESIAN_POINT ( 'NONE',  ( 21.50073740742153916, -274.6132294701671412, -227.1216102180505914 ) ) ;
#82226 = CARTESIAN_POINT ( 'NONE',  ( 19.98939996131778685, -294.8835905186925288, -222.0067426427277724 ) ) ;
#82227 = CARTESIAN_POINT ( 'NONE',  ( 32.86574627786668401, -288.1227413223216445, -301.9825422648518156 ) ) ;
#82228 = CARTESIAN_POINT ( 'NONE',  ( -58.86806092695453430, -277.8556478550650581, -197.9323254586728638 ) ) ;
#82229 = CARTESIAN_POINT ( 'NONE',  ( -112.3167853997882304, -290.6048716608109430, -252.8186953152983847 ) ) ;
#82230 = CARTESIAN_POINT ( 'NONE',  ( -110.5420538426909189, -289.5642497742517207, -273.9084403105201773 ) ) ;
#82231 = CARTESIAN_POINT ( 'NONE',  ( 34.78790591727006642, -291.2869794194224369, -249.7638253195496816 ) ) ;
#82232 = EDGE_LOOP ( 'NONE', ( #66313, #75178, #84836, #50623 ) ) ;
#82233 = CARTESIAN_POINT ( 'NONE',  ( 121.1498776811041438, 150.0802918209077177, -263.8330885344481658 ) ) ;
#82234 = CIRCLE ( 'NONE', #12718, 0.5000000000000004441 ) ;
#82235 = CARTESIAN_POINT ( 'NONE',  ( 35.18454678552089376, -287.1761590439653560, -279.1890254501961408 ) ) ;
#82236 = DIRECTION ( 'NONE',  ( -0.3307782319877045629, -0.9437085149785860994, 0.000000000000000000 ) ) ;
#82237 = CARTESIAN_POINT ( 'NONE',  ( -109.0787770382201103, -285.1447895710801390, -297.8333793970257375 ) ) ;
#82238 = CARTESIAN_POINT ( 'NONE',  ( 30.69595308386004007, -292.1495782416866973, -234.6981213144351841 ) ) ;
#82239 = CARTESIAN_POINT ( 'NONE',  ( 34.85670431790524049, -282.5442070462915467, -244.8911605663836326 ) ) ;
#82240 = CARTESIAN_POINT ( 'NONE',  ( -18.73768537273358348, -282.6392845644988938, -341.0031145581434089 ) ) ;
#82241 = CARTESIAN_POINT ( 'NONE',  ( -112.6004999004516378, -296.7565056689679182, -254.0172837666562771 ) ) ;
#82242 = CIRCLE ( 'NONE', #53526, 3.842139515347647638 ) ;
#82243 = CARTESIAN_POINT ( 'NONE',  ( -101.1542196670626623, -274.3647325816482407, -233.8004663928502964 ) ) ;
#82244 = CARTESIAN_POINT ( 'NONE',  ( -19.65860351893262248, -290.3006097881522010, -197.7876357410340233 ) ) ;
#82245 = CARTESIAN_POINT ( 'NONE',  ( 21.00648153819410879, -273.7240670479724258, -225.8138015972125743 ) ) ;
#82246 = ORIENTED_EDGE ( 'NONE', *, *, #88732, .T. ) ;
#82247 = DIRECTION ( 'NONE',  ( 1.000000000000000000, 0.000000000000000000, 0.000000000000000000 ) ) ;
#82248 = CARTESIAN_POINT ( 'NONE',  ( -70.64824542843378197, -287.5296596061101013, -203.7737172930530676 ) ) ;
#82249 = AXIS2_PLACEMENT_3D ( 'NONE', #37368, #25042, #24093 ) ;
#82250 = CARTESIAN_POINT ( 'NONE',  ( -19.34641712159132965, -295.9056945844068878, -344.9655158664165242 ) ) ;
#82251 = CARTESIAN_POINT ( 'NONE',  ( -99.11273405775577316, -284.6629569783329998, -309.5484746508861917 ) ) ;
#82252 = CARTESIAN_POINT ( 'NONE',  ( 39.38765851782513749, -274.6571107568639150, -274.0446642464561364 ) ) ;
#82253 = CARTESIAN_POINT ( 'NONE',  ( 34.36476604325291362, -293.8495615741924212, -242.4381990131205953 ) ) ;
#82254 = CARTESIAN_POINT ( 'NONE',  ( 31.59810485164540239, -285.2820247840532488, -238.8084931115682537 ) ) ;
#82255 = CARTESIAN_POINT ( 'NONE',  ( 28.09019071872619122, -294.4170334845036905, -311.0126208583176322 ) ) ;
#82256 = CARTESIAN_POINT ( 'NONE',  ( -75.87629644515328664, -289.9156054348987936, -332.3866963630273972 ) ) ;
#82257 = CARTESIAN_POINT ( 'NONE',  ( 165.0427047786672290, 250.5000000000000568, 23.37680765314704701 ) ) ;
#82258 = AXIS2_PLACEMENT_3D ( 'NONE', #15701, #569, #44563 ) ;
#82259 = CARTESIAN_POINT ( 'NONE',  ( 152.4536156746142410, 130.6065089285656313, 11.50000000000000000 ) ) ;
#82260 = CARTESIAN_POINT ( 'NONE',  ( -97.62287679132212759, -246.6820661265134618, -331.3632087810060511 ) ) ;
#82261 = CARTESIAN_POINT ( 'NONE',  ( -69.51827648917475244, -287.1564686476422708, -201.1560164551064247 ) ) ;
#82262 = CARTESIAN_POINT ( 'NONE',  ( 13.84574458161073807, -272.1952119285918457, -206.2264541496106460 ) ) ;
#82263 = ORIENTED_EDGE ( 'NONE', *, *, #7928, .F. ) ;
#82264 = CARTESIAN_POINT ( 'NONE',  ( -99.29961629950494739, -282.9321513775680046, -309.6409040358457219 ) ) ;
#82265 = CARTESIAN_POINT ( 'NONE',  ( -102.0815077564833047, -277.6711939574131520, -312.1057407934236494 ) ) ;
#82266 = CARTESIAN_POINT ( 'NONE',  ( 25.20109864939744426, -282.9954566653009920, -229.1772441344316178 ) ) ;
#82267 = CARTESIAN_POINT ( 'NONE',  ( 123.5090149810071409, 147.7087541737730589, -262.2547634134738814 ) ) ;
#82268 = CARTESIAN_POINT ( 'NONE',  ( -93.97473387653838017, -282.4245377288726218, -321.6767844689586013 ) ) ;
#82269 = CARTESIAN_POINT ( 'NONE',  ( 1.035469685148925123, -284.5867330593611655, -206.2771044218037275 ) ) ;
#82270 = CARTESIAN_POINT ( 'NONE',  ( -95.10165138745190916, -275.0844489056009365, -221.3095783874864821 ) ) ;
#82271 = CARTESIAN_POINT ( 'NONE',  ( -95.64965695262473844, -296.4263334051639163, -314.4063843879839624 ) ) ;
#82273 = VERTEX_POINT ( 'NONE', #39696 ) ;
#82272 = EDGE_CURVE ( 'NONE', #87519, #44024, #76129, .T. ) ;
#82274 = CARTESIAN_POINT ( 'NONE',  ( 11.26946036199136891, -291.4269564559353967, -215.1733394214647603 ) ) ;
#82275 = CARTESIAN_POINT ( 'NONE',  ( -71.51808368431464658, -278.1431766711897353, -339.2471658741003466 ) ) ;
#82276 = CARTESIAN_POINT ( 'NONE',  ( 31.11831592997810603, -275.2142228917865623, -245.0189357298367554 ) ) ;
#82277 = CARTESIAN_POINT ( 'NONE',  ( 24.11168832294763575, -275.0853003909469408, -316.2411088120010163 ) ) ;
#82278 = DIRECTION ( 'NONE',  ( -0.000000000000000000, -1.000000000000000000, -0.000000000000000000 ) ) ;
#82279 = CARTESIAN_POINT ( 'NONE',  ( 34.30264110741431693, -273.2639606469523414, -248.0078303435984424 ) ) ;
#82280 = EDGE_CURVE ( 'NONE', #38685, #80899, #76187, .T. ) ;
#82281 = CARTESIAN_POINT ( 'NONE',  ( -22.19645008584052803, -296.2870844745876866, -345.2558954538642979 ) ) ;
#82282 = CARTESIAN_POINT ( 'NONE',  ( 222.4306832106270804, -141.7221692137691775, -21.50000000000000000 ) ) ;
#82283 = DIRECTION ( 'NONE',  ( -1.000000000000000000, 0.000000000000000000, 0.000000000000000000 ) ) ;
#82284 = CARTESIAN_POINT ( 'NONE',  ( -108.3894215080576373, -285.3943564332374194, -288.4289723431415382 ) ) ;
#82285 = CARTESIAN_POINT ( 'NONE',  ( -100.5634172967669571, -285.7489543623862573, -312.6098302468755605 ) ) ;
#82286 = CARTESIAN_POINT ( 'NONE',  ( -96.00850166457308887, -283.2898546975542331, -313.9741787090850380 ) ) ;
#82287 = CARTESIAN_POINT ( 'NONE',  ( -70.83387214650075236, -275.9015358793878931, -336.1236820343060003 ) ) ;
#82288 = CARTESIAN_POINT ( 'NONE',  ( 1.771926599659222168, -284.3838233492475638, -333.5162375429878239 ) ) ;
#82289 = CARTESIAN_POINT ( 'NONE',  ( -16.20030696877190479, -275.2538314592206916, -341.0103004042298380 ) ) ;
#82290 = CARTESIAN_POINT ( 'NONE',  ( -16.27895970187977426, -277.8532062922993191, -340.6324934970108416 ) ) ;
#82291 = DIRECTION ( 'NONE',  ( -1.000000000000000000, 0.000000000000000000, 0.000000000000000000 ) ) ;
#82292 = CARTESIAN_POINT ( 'NONE',  ( -111.5776778699178209, -279.6043489408739902, -250.4815674253345605 ) ) ;
#82293 = CARTESIAN_POINT ( 'NONE',  ( -14.25220602997345587, -280.8359709879707680, -196.9131516146023841 ) ) ;
#82294 = ORIENTED_EDGE ( 'NONE', *, *, #27622, .F. ) ;
#82295 = ORIENTED_EDGE ( 'NONE', *, *, #33928, .T. ) ;
#82296 = CARTESIAN_POINT ( 'NONE',  ( 208.4306832106271088, 42.44233620800392970, 0.000000000000000000 ) ) ;
#82297 = CARTESIAN_POINT ( 'NONE',  ( 35.60175027823817118, -289.6739781245664744, -290.8918786898855160 ) ) ;
#82298 = CARTESIAN_POINT ( 'NONE',  ( -82.03469701510771017, -296.6224153325352404, -212.3733665212719472 ) ) ;
#82299 = CARTESIAN_POINT ( 'NONE',  ( -65.41754804382519239, -288.7581548384026178, -342.0069105027736214 ) ) ;
#82300 = CARTESIAN_POINT ( 'NONE',  ( 34.01207602265371577, -285.5357545185896129, -250.6986500786932481 ) ) ;
#82302 = CARTESIAN_POINT ( 'NONE',  ( -107.9251798957282631, -288.4988496950435888, -292.8006498307749439 ) ) ;
#82301 = CARTESIAN_POINT ( 'NONE',  ( 7.298654567911541768, -285.2485953140867991, -211.7936144675054777 ) ) ;
#82303 = CARTESIAN_POINT ( 'NONE',  ( -86.00080711093296770, -286.5653003968828330, -215.3439092773986374 ) ) ;
#82304 = CARTESIAN_POINT ( 'NONE',  ( -53.71996759329717719, -275.2620294225641260, -343.6041849123693623 ) ) ;
#82305 = CARTESIAN_POINT ( 'NONE',  ( -8.554443554831648200, -287.0815046340810568, -340.9282941819097914 ) ) ;
#82306 = AXIS2_PLACEMENT_3D ( 'NONE', #44215, #81595, #73122 ) ;
#82307 = CARTESIAN_POINT ( 'NONE',  ( 23.07660013466603388, -288.9462714987811864, -225.9243129156368184 ) ) ;
#82308 = CARTESIAN_POINT ( 'NONE',  ( 15.04027593969662391, -284.7889119940051614, -216.4523338357290640 ) ) ;
#82309 = CARTESIAN_POINT ( 'NONE',  ( 34.93771068095600185, -282.6484886582146032, -282.1549817048996260 ) ) ;
#82310 = CARTESIAN_POINT ( 'NONE',  ( -104.3808280628871898, -293.0019800063693083, -236.2494582837441897 ) ) ;
#82311 = CARTESIAN_POINT ( 'NONE',  ( 208.6208076322478746, 32.98517505407394168, 15.00000000000000000 ) ) ;
#82312 = AXIS2_PLACEMENT_3D ( 'NONE', #11293, #76629, #54832 ) ;
#82313 = CARTESIAN_POINT ( 'NONE',  ( -59.74490947996399370, -299.6844623816042485, -198.1442386401996600 ) ) ;
#82314 = CARTESIAN_POINT ( 'NONE',  ( -49.15794227921451665, -279.0948691807164437, -198.1601612854873622 ) ) ;
#82315 = CARTESIAN_POINT ( 'NONE',  ( 35.40147729201559201, -279.3168326698464057, -252.0487799954543959 ) ) ;
#82316 = CARTESIAN_POINT ( 'NONE',  ( 0.4521515363631591899, -293.7590292533312208, -337.2775621255710803 ) ) ;
#82317 = CARTESIAN_POINT ( 'NONE',  ( -106.3530803599599750, -271.1461859268238186, -243.4728301319110813 ) ) ;
#82318 = CARTESIAN_POINT ( 'NONE',  ( 33.21268639048580695, -279.9666248977115401, -249.7863270577234402 ) ) ;
#82319 = CARTESIAN_POINT ( 'NONE',  ( -57.22314067331819132, -271.8736150133341880, -198.5714445264189862 ) ) ;
#82320 = CARTESIAN_POINT ( 'NONE',  ( -28.82229586794989018, -296.2572052988252267, -343.4101705109846421 ) ) ;
#82321 = CARTESIAN_POINT ( 'NONE',  ( -35.82564250435292053, -296.5506922128299720, -194.0548301270989100 ) ) ;
#82322 = CARTESIAN_POINT ( 'NONE',  ( -2.452966189433204658, -292.8368583064619202, -337.8648235127503767 ) ) ;
#82323 = CIRCLE ( 'NONE', #15759, 4.103083949679980691 ) ;
#82324 = CARTESIAN_POINT ( 'NONE',  ( -69.28969707544821688, -293.0487016373118081, -204.0546654968482301 ) ) ;
#82325 = DIRECTION ( 'NONE',  ( 0.000000000000000000, 0.000000000000000000, 1.000000000000000000 ) ) ;
#82326 = CARTESIAN_POINT ( 'NONE',  ( -12.21432891148207212, -293.1903133549178051, -201.5960120414245011 ) ) ;
#82327 = CARTESIAN_POINT ( 'NONE',  ( 195.4048939377254612, 20.66407592107141511, 13.00192971195525260 ) ) ;
#82329 = CARTESIAN_POINT ( 'NONE',  ( 19.69376410264296240, -294.1959615334767477, -315.9437032427257463 ) ) ;
#82328 = CARTESIAN_POINT ( 'NONE',  ( -71.02661073327266195, -281.5145903600248971, -337.7683401800813385 ) ) ;
#82330 = CARTESIAN_POINT ( 'NONE',  ( -44.41921528159145538, -283.1392056562684161, -347.0885178160152122 ) ) ;
#82331 = CARTESIAN_POINT ( 'NONE',  ( 18.08688398155689825, -282.7594143343150677, -219.0095234404410292 ) ) ;
#82332 = CARTESIAN_POINT ( 'NONE',  ( -15.41541560388288268, -285.9950106876013933, -196.5156162487277811 ) ) ;
#82333 = CARTESIAN_POINT ( 'NONE',  ( -96.54968594335289822, -289.1805867965553603, -224.5960347188872106 ) ) ;
#82334 = CARTESIAN_POINT ( 'NONE',  ( 8.774264289413407525, -280.9125225619765160, -331.1560649499425040 ) ) ;
#82335 = AXIS2_PLACEMENT_3D ( 'NONE', #58290, #80041, #28008 ) ;
#82336 = CARTESIAN_POINT ( 'NONE',  ( 22.40219264894185258, -285.6417616310222343, -227.4744668200887077 ) ) ;
#82337 = CARTESIAN_POINT ( 'NONE',  ( -36.10566880880616480, -287.9573632209215361, -347.0551039967792235 ) ) ;
#82338 = CARTESIAN_POINT ( 'NONE',  ( 209.7513585654922679, 305.7026273589066818, -40.00000000000000711 ) ) ;
#82339 = CARTESIAN_POINT ( 'NONE',  ( 25.11505198095997926, -295.6905751152608559, -309.7712034197534763 ) ) ;
#82340 = CARTESIAN_POINT ( 'NONE',  ( -6.793467250638665078, -278.0842477673292024, -340.4139116144750119 ) ) ;
#82342 = CARTESIAN_POINT ( 'NONE',  ( -69.74585591249896765, -279.2800294973382051, -204.9098319310765248 ) ) ;
#82341 = CARTESIAN_POINT ( 'NONE',  ( 38.06569873877572263, -291.5719387353748289, -270.3362162858428519 ) ) ;
#82343 = CARTESIAN_POINT ( 'NONE',  ( 1.698269939996603028, -292.7254207456073800, -203.9309096179724747 ) ) ;
#82344 = CARTESIAN_POINT ( 'NONE',  ( -86.78877972638498761, -283.4509864546686799, -213.1578123247464873 ) ) ;
#82345 = CARTESIAN_POINT ( 'NONE',  ( -87.84604204900279001, -279.7582887888356140, -325.8075975232892461 ) ) ;
#82346 = CARTESIAN_POINT ( 'NONE',  ( 8.365698332263766801, -293.4677985638718951, -327.6472782796748788 ) ) ;
#82347 = CARTESIAN_POINT ( 'NONE',  ( -112.5083667949886461, -270.5523135770945373, -270.3357088371093937 ) ) ;
#82348 = ORIENTED_EDGE ( 'NONE', *, *, #78116, .T. ) ;
#82349 = CARTESIAN_POINT ( 'NONE',  ( 175.2296996224750103, 247.0000000000001137, 0.000000000000000000 ) ) ;
#82350 = CARTESIAN_POINT ( 'NONE',  ( 36.18295524096621563, -283.3658419134645214, -257.4781114522689904 ) ) ;
#82351 = CARTESIAN_POINT ( 'NONE',  ( 34.77569810849829679, -292.9044577444097399, -258.5751844807919042 ) ) ;
#82352 = CARTESIAN_POINT ( 'NONE',  ( 164.2231345125756263, 264.6571197653884155, -7.500000000000000000 ) ) ;
#82353 = CARTESIAN_POINT ( 'NONE',  ( 26.53690525259170840, -296.4086741954485547, -200.3901485728259502 ) ) ;
#82354 = CARTESIAN_POINT ( 'NONE',  ( -37.24182466774747979, -297.1121290728679583, -193.5956645125883142 ) ) ;
#82355 = CARTESIAN_POINT ( 'NONE',  ( -36.07808213071292158, -290.3518211694541833, -346.8705593816237069 ) ) ;
#82356 = CARTESIAN_POINT ( 'NONE',  ( 1.309783167006689730, -288.3533245194732899, -332.2890021995091843 ) ) ;
#82357 = CARTESIAN_POINT ( 'NONE',  ( -4.051520344647697058, -282.0194722664597293, -204.6015894868916121 ) ) ;
#82358 = CARTESIAN_POINT ( 'NONE',  ( -90.79299233280737269, -299.0416136491614907, -219.0926954798472366 ) ) ;
#82359 = CARTESIAN_POINT ( 'NONE',  ( -85.73453516167337796, -278.1592304967379050, -215.1772070919432167 ) ) ;
#82360 = ORIENTED_EDGE ( 'NONE', *, *, #27217, .F. ) ;
#82361 = CARTESIAN_POINT ( 'NONE',  ( -89.59083614453417965, -297.0064800756047703, -213.7577536588895271 ) ) ;
#82362 = CARTESIAN_POINT ( 'NONE',  ( -1.772462948257002679, -294.4473627420438788, -204.9544162125113189 ) ) ;
#82363 = CARTESIAN_POINT ( 'NONE',  ( 27.43669690149172524, -295.6836765490610333, -310.5875840072461642 ) ) ;
#82364 = CARTESIAN_POINT ( 'NONE',  ( 114.7448031289451222, -299.5541904835127980, -195.3611179825600175 ) ) ;
#82365 = CARTESIAN_POINT ( 'NONE',  ( -110.4699854496919329, -291.2285162601526167, -268.4673839537786648 ) ) ;
#82366 = DIRECTION ( 'NONE',  ( 0.4999999999999966693, 0.8660254037844405950, 0.000000000000000000 ) ) ;
#82367 = ORIENTED_EDGE ( 'NONE', *, *, #33815, .T. ) ;
#82368 = CARTESIAN_POINT ( 'NONE',  ( 8.128853119374587877, -290.8056646032590606, -209.6925369026090209 ) ) ;
#82369 = CARTESIAN_POINT ( 'NONE',  ( -107.9979751857916312, -272.3074194226331883, -251.5747286257295059 ) ) ;
#82370 = CARTESIAN_POINT ( 'NONE',  ( 196.0143093133015384, 20.19615242270663913, -11.99999999999998579 ) ) ;
#82371 = CARTESIAN_POINT ( 'NONE',  ( 195.4790382475684680, 26.04803379143200104, 14.66351318240304558 ) ) ;
#82372 = CARTESIAN_POINT ( 'NONE',  ( -112.2481029937105603, -292.2567656670873930, -255.7417230204102623 ) ) ;
#82373 = CARTESIAN_POINT ( 'NONE',  ( -37.30987171927208124, -297.5519495502701375, -350.3611179825600175 ) ) ;
#82374 = CARTESIAN_POINT ( 'NONE',  ( -1.325855163764886324, -288.5307547953036647, -204.7065888023394109 ) ) ;
#82375 = CARTESIAN_POINT ( 'NONE',  ( 22.15424010287022938, -272.9291109023894251, -224.9499129657051242 ) ) ;
#82376 = CARTESIAN_POINT ( 'NONE',  ( 36.13243484384660320, -277.6309709322517847, -282.6258391460973485 ) ) ;
#82377 = CARTESIAN_POINT ( 'NONE',  ( 11.90135421255370041, -290.8220737860941085, -214.4672679067443255 ) ) ;
#82378 = CARTESIAN_POINT ( 'NONE',  ( -105.0820021792415702, -280.8575107608771759, -236.3096018622354677 ) ) ;
#82379 = VERTEX_POINT ( 'NONE', #77588 ) ;
#82380 = CARTESIAN_POINT ( 'NONE',  ( -66.60798983522049355, -282.7944856228870663, -337.3625954408391863 ) ) ;
#82381 = CARTESIAN_POINT ( 'NONE',  ( -103.1534298860790102, -280.1484552695858383, -230.8838705315120023 ) ) ;
#82382 = CARTESIAN_POINT ( 'NONE',  ( -14.33232856959805979, -279.1388214160971302, -197.2399322328401183 ) ) ;
#82383 = VECTOR ( 'NONE', #80016, 1000.000000000000000 ) ;
#82384 = CARTESIAN_POINT ( 'NONE',  ( -111.5680120584095363, -268.0791262347229917, -295.3987848039294590 ) ) ;
#82385 = CARTESIAN_POINT ( 'NONE',  ( 19.85252384393870884, -275.7961232425344065, -219.0810537184380564 ) ) ;
#82386 = EDGE_CURVE ( 'NONE', #783, #30831, #11096, .T. ) ;
#82387 = SHAPE_DEFINITION_REPRESENTATION ( #48138, #30030 ) ;
#82388 = CARTESIAN_POINT ( 'NONE',  ( -24.29734724329654583, -275.7357690683512601, -195.1239819704289005 ) ) ;
#82389 = CARTESIAN_POINT ( 'NONE',  ( -110.4683760289727132, -299.2662352645559167, -253.7030783399848985 ) ) ;
#82390 = ORIENTED_EDGE ( 'NONE', *, *, #51997, .T. ) ;
#82391 = EDGE_LOOP ( 'NONE', ( #71192, #27191, #80062, #74102 ) ) ;
#82392 = CARTESIAN_POINT ( 'NONE',  ( -61.34329307534394360, -290.4510202371023411, -339.6297949535154430 ) ) ;
#82393 = CARTESIAN_POINT ( 'NONE',  ( -12.53310460084819233, -290.4941845545233718, -342.2390122968308219 ) ) ;
#82394 = CARTESIAN_POINT ( 'NONE',  ( -77.30395300483738197, -290.8490545257827193, -209.1491010820159318 ) ) ;
#82395 = CARTESIAN_POINT ( 'NONE',  ( -63.17486536149112197, -285.2321353220696096, -197.8892304868761016 ) ) ;
#82396 = CARTESIAN_POINT ( 'NONE',  ( 197.7672738693491965, 26.00182986903273274, 10.01345434887959662 ) ) ;
#82397 = CARTESIAN_POINT ( 'NONE',  ( 6.046154686107807485, -280.8522137280722859, -330.0598153541484976 ) ) ;
#82398 = CARTESIAN_POINT ( 'NONE',  ( 33.49936643192386043, -289.7037721265573964, -292.7226674005448785 ) ) ;
#82399 = CARTESIAN_POINT ( 'NONE',  ( -87.41399834689386239, -282.2453534015842251, -324.5000960783352184 ) ) ;
#82400 = CARTESIAN_POINT ( 'NONE',  ( 20.05069849074380173, -282.2231019863413621, -224.4551699962655107 ) ) ;
#82401 = CARTESIAN_POINT ( 'NONE',  ( 3.066503686219371527, -289.4652134990666923, -335.6921350426601975 ) ) ;
#82402 = CARTESIAN_POINT ( 'NONE',  ( -92.25883456660780269, -279.7318883752008674, -222.1539447692411215 ) ) ;
#82403 = CARTESIAN_POINT ( 'NONE',  ( -47.67456082792981675, -290.7186301013121010, -194.4047646367734217 ) ) ;
#82404 = AXIS2_PLACEMENT_3D ( 'NONE', #39166, #89836, #68078 ) ;
#82405 = CARTESIAN_POINT ( 'NONE',  ( -96.14013522136471579, -284.6872832165995533, -319.8476514505357500 ) ) ;
#82406 = CARTESIAN_POINT ( 'NONE',  ( -43.66746537090856606, -286.4667297865374849, -193.6299278297640285 ) ) ;
#82407 = CARTESIAN_POINT ( 'NONE',  ( -36.19140285010022495, -283.2040122275516296, -343.3520545480408259 ) ) ;
#82408 = EDGE_LOOP ( 'NONE', ( #32526, #38468, #54561, #31241 ) ) ;
#82409 = CARTESIAN_POINT ( 'NONE',  ( 139.6925840978351516, -0.9999999999999991118, 21.50000000000000000 ) ) ;
#82410 = CARTESIAN_POINT ( 'NONE',  ( 21.23890289750610094, -294.7567841826703443, -222.3130333863156807 ) ) ;
#82411 = CARTESIAN_POINT ( 'NONE',  ( 38.32631535113828392, -292.3791924145763232, -281.6593349319833237 ) ) ;
#82412 = CARTESIAN_POINT ( 'NONE',  ( 18.48000754087588149, -275.2828207700454755, -317.7672927031441645 ) ) ;
#82413 = CARTESIAN_POINT ( 'NONE',  ( -50.45830788761586660, -294.5638708112776953, -346.1861437054520252 ) ) ;
#82414 = CARTESIAN_POINT ( 'NONE',  ( -6.966949695409581977, -290.9380486166039645, -203.2188638474794971 ) ) ;
#82415 = CARTESIAN_POINT ( 'NONE',  ( -12.69159266024655786, -292.9672450212768808, -340.2029740491024086 ) ) ;
#82416 = CARTESIAN_POINT ( 'NONE',  ( -86.20475253174726049, -292.5617293144588871, -215.5247079408773914 ) ) ;
#82417 = CARTESIAN_POINT ( 'NONE',  ( 2.396559803831197932, -293.6777613780329261, -208.6966338344543885 ) ) ;
#82418 = CARTESIAN_POINT ( 'NONE',  ( 194.7510731661265595, 15.36528803885690664, 21.50000000000000000 ) ) ;
#82419 = CARTESIAN_POINT ( 'NONE',  ( 24.19867358784602374, -292.1369262863266840, -313.5438630105738866 ) ) ;
#82420 = CARTESIAN_POINT ( 'NONE',  ( -111.1737870672073996, -298.3821100613930639, -283.6168362630506294 ) ) ;
#82421 = CARTESIAN_POINT ( 'NONE',  ( 24.44326591872133747, -289.0353032477154898, -309.6806604337058957 ) ) ;
#82422 = CARTESIAN_POINT ( 'NONE',  ( -9.789223836702888093, -278.6739310197044688, -340.4986104771514306 ) ) ;
#82423 = CARTESIAN_POINT ( 'NONE',  ( -2.917370278473610412, -275.4023709352172204, -338.8079792516905968 ) ) ;
#82424 = CARTESIAN_POINT ( 'NONE',  ( -46.86014843659808804, -273.2828821998430158, -194.0544214992168577 ) ) ;
#82425 = CARTESIAN_POINT ( 'NONE',  ( 31.66036271606739660, -279.9987828457924479, -298.2901265364556025 ) ) ;
#82426 = CARTESIAN_POINT ( 'NONE',  ( -106.8547622138593880, -276.5477313686046728, -301.7045630273628944 ) ) ;
#82427 = CARTESIAN_POINT ( 'NONE',  ( -109.0768573479720374, -295.0276082819629551, -286.3395627853093970 ) ) ;
#82428 = CARTESIAN_POINT ( 'NONE',  ( 154.7659666677267580, 19.56018909072085066, 12.94946946941272437 ) ) ;
#82429 = CARTESIAN_POINT ( 'NONE',  ( -92.10001089432864774, -273.8945109453640612, -221.9315808135544046 ) ) ;
#82430 = CARTESIAN_POINT ( 'NONE',  ( 211.1232656141943949, 0.000000000000000000, 7.000000000000000000 ) ) ;
#82432 = CARTESIAN_POINT ( 'NONE',  ( 34.12178154374939254, -275.1881280873132027, -255.4014008279607424 ) ) ;
#82431 = CARTESIAN_POINT ( 'NONE',  ( 27.47583976550490092, -286.0839420963176281, -308.7940898036301292 ) ) ;
#82433 = CARTESIAN_POINT ( 'NONE',  ( -14.95224843126578662, -288.7700580054889770, -344.0898795096062486 ) ) ;
#82434 = CARTESIAN_POINT ( 'NONE',  ( -82.49951617655160874, -275.4376479921858163, -210.2060239856061798 ) ) ;
#82435 = CARTESIAN_POINT ( 'NONE',  ( -109.5994094017950289, -294.8033588208400033, -250.8476857577201429 ) ) ;
#82436 = EDGE_CURVE ( 'NONE', #48386, #52785, #59510, .T. ) ;
#82437 = CARTESIAN_POINT ( 'NONE',  ( -5.531717702487208399, -281.8414302763886781, -340.3059808331532281 ) ) ;
#82438 = ADVANCED_FACE ( 'NONE', ( #5162 ), #34037, .F. ) ;
#82439 = CARTESIAN_POINT ( 'NONE',  ( 82.68073018288104947, -297.0543924324409204, -195.4120394483015559 ) ) ;
#82440 = CARTESIAN_POINT ( 'NONE',  ( 36.74826726560811352, -279.7056617040976789, -282.3293288460289432 ) ) ;
#82441 = CARTESIAN_POINT ( 'NONE',  ( 195.4048939377254612, 20.66407592107141511, -13.00192971195525260 ) ) ;
#82442 = CARTESIAN_POINT ( 'NONE',  ( -67.95288029525517004, -290.4360297557573745, -203.6383445090889666 ) ) ;
#82443 = CARTESIAN_POINT ( 'NONE',  ( -36.19786556952487189, -281.1772442848348987, -344.5875090164536232 ) ) ;
#82444 = CARTESIAN_POINT ( 'NONE',  ( 197.8829252751895069, 41.74573726702125498, 11.20279836830544795 ) ) ;
#82445 = DIRECTION ( 'NONE',  ( 0.000000000000000000, 0.000000000000000000, 1.000000000000000000 ) ) ;
#82446 = CARTESIAN_POINT ( 'NONE',  ( -75.98894803118911057, -289.5362158942540418, -206.0246006044155251 ) ) ;
#82447 = CARTESIAN_POINT ( 'NONE',  ( 11.99648687322780560, -276.2726565792751785, -215.5525755127405318 ) ) ;
#82448 = CARTESIAN_POINT ( 'NONE',  ( -66.41128102162380742, -284.6294906515863659, -341.2481309384935457 ) ) ;
#82450 = CARTESIAN_POINT ( 'NONE',  ( -108.9794944755538069, -284.3669859658438668, -284.3977280088179782 ) ) ;
#82449 = CARTESIAN_POINT ( 'NONE',  ( -27.16577893794107013, -272.2602384215733764, -195.4370302956241687 ) ) ;
#82451 = CARTESIAN_POINT ( 'NONE',  ( 35.96346016646441512, -276.8856398335441327, -263.3466719203497064 ) ) ;
#82452 = CARTESIAN_POINT ( 'NONE',  ( -24.29077734957826351, -277.6842273968209156, -342.4007043862353044 ) ) ;
#82453 = CARTESIAN_POINT ( 'NONE',  ( 12.37458611862648716, -284.3604744053404829, -326.5844448629242152 ) ) ;
#82454 = ORIENTED_EDGE ( 'NONE', *, *, #76975, .T. ) ;
#82455 = CARTESIAN_POINT ( 'NONE',  ( 204.7105398379021040, 292.9631599619078202, -53.99999999999737810 ) ) ;
#82456 = CARTESIAN_POINT ( 'NONE',  ( 39.65608403047398411, -293.3489238575383524, -267.4387204345877080 ) ) ;
#82457 = DIRECTION ( 'NONE',  ( -0.000000000000000000, 1.000000000000000000, -0.000000000000000000 ) ) ;
#82458 = CARTESIAN_POINT ( 'NONE',  ( 19.08544293954241766, -290.2386823636759345, -319.7867301798541462 ) ) ;
#82459 = CARTESIAN_POINT ( 'NONE',  ( -88.47809603358389552, -288.9094976428775681, -206.1857440867352693 ) ) ;
#82460 = CARTESIAN_POINT ( 'NONE',  ( -77.73872415856457962, -276.7767824746940164, -335.7853221518901137 ) ) ;
#82461 = CARTESIAN_POINT ( 'NONE',  ( -69.26917854255420082, -290.0389958407305926, -201.1582244431931485 ) ) ;
#82462 = CARTESIAN_POINT ( 'NONE',  ( -90.17329783333302373, -286.8088472991352091, -218.9115122137386891 ) ) ;
#82463 = VECTOR ( 'NONE', #92636, 1000.000000000000000 ) ;
#82464 = CARTESIAN_POINT ( 'NONE',  ( -96.89521200831394765, -279.7044992259339438, -314.3295175566887565 ) ) ;
#82465 = CARTESIAN_POINT ( 'NONE',  ( -26.72109892221409666, -287.6098473805943172, -194.6389530431369508 ) ) ;
#82466 = CARTESIAN_POINT ( 'NONE',  ( 34.14519963821470583, -283.8470210495419224, -293.2157675015203040 ) ) ;
#82467 = CARTESIAN_POINT ( 'NONE',  ( 39.62351893222895427, -275.7648644548721109, -274.0418474908827875 ) ) ;
#82468 = CARTESIAN_POINT ( 'NONE',  ( -62.40799748749950027, -277.2026169686447474, -343.2232009398261994 ) ) ;
#82469 = CARTESIAN_POINT ( 'NONE',  ( -35.80224228992085500, -299.9917209434586880, -195.9206014286108086 ) ) ;
#82470 = CARTESIAN_POINT ( 'NONE',  ( 156.1243321211828743, 16.88031981475914023, 7.577257116167345430 ) ) ;
#82471 = CARTESIAN_POINT ( 'NONE',  ( -20.19161114001083490, -279.3376638359844719, -345.3538533559490702 ) ) ;
#82472 = CARTESIAN_POINT ( 'NONE',  ( -84.42992257984572291, -295.5513200389712551, -211.0062126747269531 ) ) ;
#82473 = CARTESIAN_POINT ( 'NONE',  ( 196.0143093133015384, 73.40565171261609123, -11.99999999999998046 ) ) ;
#82474 = CARTESIAN_POINT ( 'NONE',  ( -45.92154307301868954, -276.6713879772625546, -342.9677976229069145 ) ) ;
#82475 = CARTESIAN_POINT ( 'NONE',  ( 9.256585017003372329, -275.8815282660360140, -209.5613767083460459 ) ) ;
#82476 = CARTESIAN_POINT ( 'NONE',  ( 26.51947287183731916, -281.1733385392578271, -312.9588972198923216 ) ) ;
#82477 = CARTESIAN_POINT ( 'NONE',  ( 28.55021068458711042, -288.8592404642445217, -236.5401726730200380 ) ) ;
#82478 = CARTESIAN_POINT ( 'NONE',  ( -105.3310694831036898, -297.6207611210693926, -305.1206862837325957 ) ) ;
#82479 = CARTESIAN_POINT ( 'NONE',  ( -97.95083187663782098, -297.1286502173527992, -317.2070555743242721 ) ) ;
#82480 = CARTESIAN_POINT ( 'NONE',  ( -47.26209866149315530, -293.9259653719904577, -196.1882515306018036 ) ) ;
#82481 = CARTESIAN_POINT ( 'NONE',  ( 22.81763154704554708, -278.9430459116272232, -225.8324271297751693 ) ) ;
#82482 = CARTESIAN_POINT ( 'NONE',  ( 12.24724870204911120, -282.6689241379756936, -214.8430997424370901 ) ) ;
#82483 = CARTESIAN_POINT ( 'NONE',  ( -60.94986093148587969, -295.8233386440902564, -199.7093702652381637 ) ) ;
#82484 = CARTESIAN_POINT ( 'NONE',  ( -108.2911461885014575, -286.5099392827481779, -242.4215404325482268 ) ) ;
#82485 = CARTESIAN_POINT ( 'NONE',  ( 35.98995588070685159, -286.4456292925386833, -268.3175028324865252 ) ) ;
#82486 = CARTESIAN_POINT ( 'NONE',  ( 12.93180314520840390, -280.0814861625955245, -212.1727372273141725 ) ) ;
#82487 = CARTESIAN_POINT ( 'NONE',  ( 195.6606144031773624, 277.6437891327478837, -125.5779349732042931 ) ) ;
#82488 = VERTEX_POINT ( 'NONE', #91774 ) ;
#82489 = CARTESIAN_POINT ( 'NONE',  ( -5.785668917394137800, -286.1455220606764556, -204.4967079756274018 ) ) ;
#82490 = VERTEX_POINT ( 'NONE', #68621 ) ;
#82491 = CARTESIAN_POINT ( 'NONE',  ( -44.37710816238698897, -284.2187029469874915, -346.7817639628316329 ) ) ;
#82492 = CARTESIAN_POINT ( 'NONE',  ( 33.52867671504472469, -275.6533577303742391, -252.7691546761126062 ) ) ;
#82493 = CARTESIAN_POINT ( 'NONE',  ( -21.05335969569015475, -285.0516084391568370, -195.5099410818497745 ) ) ;
#82494 = CARTESIAN_POINT ( 'NONE',  ( -72.02014421385571552, -290.5248190885428698, -201.9441074920214305 ) ) ;
#82495 = CARTESIAN_POINT ( 'NONE',  ( 14.99213384018927897, -281.7097151317625503, -214.1280680830554388 ) ) ;
#82496 = DIRECTION ( 'NONE',  ( -0.000000000000000000, 1.000000000000000000, -0.000000000000000000 ) ) ;
#82497 = CARTESIAN_POINT ( 'NONE',  ( -36.77730032759365031, -281.5792412576677748, -194.0436084626722391 ) ) ;
#82498 = CARTESIAN_POINT ( 'NONE',  ( 23.38885489124345796, -282.5177557511680106, -317.6851052038866783 ) ) ;
#82499 = CARTESIAN_POINT ( 'NONE',  ( 7.450504543161054372, -290.1952119285918457, -214.2458315076590907 ) ) ;
#82500 = CARTESIAN_POINT ( 'NONE',  ( -38.96138201640420107, -140.0153644756211690, -364.8523457303913347 ) ) ;
#82501 = VERTEX_POINT ( 'NONE', #32637 ) ;
#82502 = CARTESIAN_POINT ( 'NONE',  ( -0.5471318346057595372, -278.5625625246000254, -335.5825473192836625 ) ) ;
#82503 = CARTESIAN_POINT ( 'NONE',  ( -40.57655935219229093, -139.1380882315665986, -364.1107628283134545 ) ) ;
#82504 = CARTESIAN_POINT ( 'NONE',  ( 32.62056299121131531, -279.2311140906252263, -244.1909987935560480 ) ) ;
#82505 = CARTESIAN_POINT ( 'NONE',  ( -70.50638936266145151, -296.9514916630077437, -205.2012279533325625 ) ) ;
#82506 = CARTESIAN_POINT ( 'NONE',  ( -30.69633000902539166, -291.6415512030366699, -193.6574660430720769 ) ) ;
#82507 = DIRECTION ( 'NONE',  ( 0.000000000000000000, 0.000000000000000000, 1.000000000000000000 ) ) ;
#82509 = CARTESIAN_POINT ( 'NONE',  ( 31.22093536719553342, -286.3150514432832097, -297.8046255616397389 ) ) ;
#82508 = CARTESIAN_POINT ( 'NONE',  ( -34.76575678976643502, -296.6585409844428796, -193.9509524979931996 ) ) ;
#82510 = CARTESIAN_POINT ( 'NONE',  ( 2.248281095152399711, -296.3765907232597669, -333.2192939629504167 ) ) ;
#82511 = CARTESIAN_POINT ( 'NONE',  ( -70.21796471413269103, -286.9247774450184352, -204.6173688880804207 ) ) ;
#82512 = CARTESIAN_POINT ( 'NONE',  ( 32.02256854360830829, -294.9175076157478088, -303.3699990487363607 ) ) ;
#82513 = B_SPLINE_CURVE_WITH_KNOTS ( 'NONE', 3,
 ( #72510, #62027, #24158, #60173, #68197, #68666, #53520, #32206 ),
 .UNSPECIFIED., .F., .F.,
 ( 4, 2, 2, 4 ),
 ( 0.0006959094422096703380, 0.002907332141605427356, 0.005118754841001184157, 0.009541600239792700361 ),
 .UNSPECIFIED. ) ;
#82514 = CARTESIAN_POINT ( 'NONE',  ( -101.8225919313987049, -284.5754438083872628, -304.8228607998860298 ) ) ;
#82515 = CARTESIAN_POINT ( 'NONE',  ( -101.9731046116610003, -295.8888496526600420, -229.2418977489899135 ) ) ;
#82516 = CARTESIAN_POINT ( 'NONE',  ( -74.60954791432716604, -292.3720246158036957, -203.1653864064323614 ) ) ;
#82517 = CARTESIAN_POINT ( 'NONE',  ( -69.60308056145483135, -292.1311322703077167, -200.4988796696016209 ) ) ;
#82518 = CARTESIAN_POINT ( 'NONE',  ( -95.76704589989074634, -290.1042463191600405, -314.1481634469123492 ) ) ;
#82519 = ORIENTED_EDGE ( 'NONE', *, *, #51459, .F. ) ;
#82520 = CARTESIAN_POINT ( 'NONE',  ( 150.6539576904058606, 293.9636489450775230, 0.000000000000000000 ) ) ;
#82521 = CARTESIAN_POINT ( 'NONE',  ( -43.21797973049908848, -299.8392521455532460, -194.7721816118493052 ) ) ;
#82522 = CARTESIAN_POINT ( 'NONE',  ( -100.8706084217704557, -271.9150025699899516, -227.4638311334730076 ) ) ;
#82523 = CARTESIAN_POINT ( 'NONE',  ( -7.167449183939760715, -281.7050822454705781, -337.1051002758651407 ) ) ;
#82524 = ORIENTED_EDGE ( 'NONE', *, *, #59598, .T. ) ;
#82525 = CARTESIAN_POINT ( 'NONE',  ( 19.82727180492823038, -275.7594858833610374, -321.8709823898286686 ) ) ;
#82526 = CARTESIAN_POINT ( 'NONE',  ( -46.25542043764335176, -272.3370527488094694, -197.1014018725825849 ) ) ;
#82527 = CARTESIAN_POINT ( 'NONE',  ( -84.23605247048401168, -281.2601017368796192, -212.7464547270773778 ) ) ;
#82528 = CARTESIAN_POINT ( 'NONE',  ( -24.13270432275103872, -275.0214075023241094, -343.4640216112316011 ) ) ;
#82529 = CARTESIAN_POINT ( 'NONE',  ( -110.1966948570239566, -297.6350803071970290, -279.6713539545851859 ) ) ;
#82530 = CARTESIAN_POINT ( 'NONE',  ( -40.54518219594275763, -299.0906332331567228, -197.1094297797922650 ) ) ;
#82531 = CARTESIAN_POINT ( 'NONE',  ( -99.28325899652840292, -298.7465347038093455, -225.9799992343394877 ) ) ;
#82532 = CARTESIAN_POINT ( 'NONE',  ( -68.14807520117722106, -271.6697632744218254, -201.5765881853824908 ) ) ;
#82533 = CARTESIAN_POINT ( 'NONE',  ( 19.77860531266616917, -294.8472692415576830, -316.0008455415297703 ) ) ;
#82534 = CARTESIAN_POINT ( 'NONE',  ( -25.29489728844791685, -290.7833046504463823, -197.7127380761053814 ) ) ;
#82535 = CARTESIAN_POINT ( 'NONE',  ( 179.7289557593406357, 249.5000000000000568, -24.91818181818183575 ) ) ;
#82536 = CARTESIAN_POINT ( 'NONE',  ( 37.57355239530809854, -275.8244566266408810, -252.7757981883405023 ) ) ;
#82537 = CARTESIAN_POINT ( 'NONE',  ( -87.33484883728418424, -273.4984532070666887, -217.0971217899188446 ) ) ;
#82538 = CARTESIAN_POINT ( 'NONE',  ( 29.32391031239793477, -280.7283780216035893, -308.0056250998787846 ) ) ;
#82539 = CARTESIAN_POINT ( 'NONE',  ( 208.4306832106271656, 1.063508326895939327, -7.500000000000014211 ) ) ;
#82540 = CARTESIAN_POINT ( 'NONE',  ( -110.2575368903987254, -283.6704687388914294, -276.3513163007959861 ) ) ;
#82541 = CARTESIAN_POINT ( 'NONE',  ( -89.19237935618261304, -281.7789361055441759, -324.8525023825768017 ) ) ;
#82542 = CARTESIAN_POINT ( 'NONE',  ( 34.95575594754692617, -273.9472338617135279, -256.6333081294811223 ) ) ;
#82543 = CARTESIAN_POINT ( 'NONE',  ( -18.37500761558206008, -282.2965549838534685, -197.7458778143534346 ) ) ;
#82544 = EDGE_CURVE ( 'NONE', #26494, #18590, #83681, .T. ) ;
#82545 = CARTESIAN_POINT ( 'NONE',  ( 209.5770068336137797, 1.043152431597804020, 7.415392722555408156 ) ) ;
#82546 = CARTESIAN_POINT ( 'NONE',  ( 121.3395553409046670, -299.5541904835127980, -195.3611179825600175 ) ) ;
#82547 = CARTESIAN_POINT ( 'NONE',  ( 4.441702967271813129, -273.0051304735683857, -206.5757633865261482 ) ) ;
#82548 = CARTESIAN_POINT ( 'NONE',  ( -98.15124213503874273, -279.9515046995883267, -314.5670193432101769 ) ) ;
#82549 = EDGE_CURVE ( 'NONE', #8050, #64275, #10560, .T. ) ;
#82550 = DIRECTION ( 'NONE',  ( 0.000000000000000000, 0.000000000000000000, -1.000000000000000000 ) ) ;
#82551 = CARTESIAN_POINT ( 'NONE',  ( -78.35716676517075996, -285.5195928006980921, -333.8201259565773285 ) ) ;
#82552 = ORIENTED_EDGE ( 'NONE', *, *, #66060, .T. ) ;
#82553 = CARTESIAN_POINT ( 'NONE',  ( 156.3466120839444216, 16.19322481500736188, -7.221609175748793241 ) ) ;
#82554 = CARTESIAN_POINT ( 'NONE',  ( -108.6127905447404061, -288.8555574166600763, -246.8444638832748126 ) ) ;
#82555 = DIRECTION ( 'NONE',  ( 1.000000000000000000, 0.000000000000000000, 0.000000000000000000 ) ) ;
#82556 = CARTESIAN_POINT ( 'NONE',  ( -94.75236337395298847, -295.9893873475351143, -224.6320653799195100 ) ) ;
#82557 = CARTESIAN_POINT ( 'NONE',  ( -89.54625175619254662, -287.9371772843049939, -323.1394304648690650 ) ) ;
#82558 = CARTESIAN_POINT ( 'NONE',  ( 157.2832821354339501, 16.68119283998691316, -9.201835683359409046 ) ) ;
#82559 = CARTESIAN_POINT ( 'NONE',  ( -94.24566304080687473, -295.2291774487622433, -221.4850559888845396 ) ) ;
#82560 = CARTESIAN_POINT ( 'NONE',  ( 25.27160399030096016, -286.6147049481688214, -314.0669675456417167 ) ) ;
#82561 = CARTESIAN_POINT ( 'NONE',  ( 33.88033775284389293, -282.8990588323061388, -250.9773150130828583 ) ) ;
#82562 = CARTESIAN_POINT ( 'NONE',  ( -93.66333683618501027, -282.0897228687630331, -321.3887287345775690 ) ) ;
#82563 = CARTESIAN_POINT ( 'NONE',  ( 3.614607755860435478, -288.4844018644666335, -330.8503828652974903 ) ) ;
#82564 = CARTESIAN_POINT ( 'NONE',  ( 26.07596077042461147, -283.4872486566332555, -307.7924733455990349 ) ) ;
#82565 = CARTESIAN_POINT ( 'NONE',  ( 35.84866676538538854, -282.3314068456118662, -268.5694435731335261 ) ) ;
#82566 = CARTESIAN_POINT ( 'NONE',  ( 35.91158350479658168, -289.7585610763740647, -288.0895074394872495 ) ) ;
#82567 = CARTESIAN_POINT ( 'NONE',  ( -78.20426114684735808, -297.6853195782457533, -205.0981797136934688 ) ) ;
#82568 = CARTESIAN_POINT ( 'NONE',  ( -63.55709447827728553, -273.7197109947475155, -197.9611656409754517 ) ) ;
#82569 = CARTESIAN_POINT ( 'NONE',  ( 14.01698657334408971, -294.7572256928926322, -216.1934883399696616 ) ) ;
#82570 = CARTESIAN_POINT ( 'NONE',  ( 208.4306832106270804, -147.7221692137691775, 0.000000000000000000 ) ) ;
#82571 = CARTESIAN_POINT ( 'NONE',  ( 31.98288692825981272, -284.4805209788416960, -303.7098442033569654 ) ) ;
#82572 = ORIENTED_EDGE ( 'NONE', *, *, #28796, .T. ) ;
#82573 = CARTESIAN_POINT ( 'NONE',  ( 36.10863148312927962, -273.7573775827134455, -286.3922995662848052 ) ) ;
#82574 = CARTESIAN_POINT ( 'NONE',  ( 197.5016171081239236, 69.66454985082778251, 11.63779655374072242 ) ) ;
#82575 = CARTESIAN_POINT ( 'NONE',  ( -112.8066049457675746, -295.0866563836123078, -259.7080953377011383 ) ) ;
#82576 = CARTESIAN_POINT ( 'NONE',  ( -102.3381664136654905, -291.6794734305941574, -305.4250944542794173 ) ) ;
#82577 = CARTESIAN_POINT ( 'NONE',  ( 7.399835882282070010, -274.0295742914274228, -212.5503264012068314 ) ) ;
#82578 = CARTESIAN_POINT ( 'NONE',  ( -97.10970357946827392, -291.4750224174902087, -313.4713663806534214 ) ) ;
#82579 = CARTESIAN_POINT ( 'NONE',  ( -38.91461170556577542, -292.9731931671891516, -197.1427159379056491 ) ) ;
#82580 = CARTESIAN_POINT ( 'NONE',  ( -74.28339403856894307, -285.3101900770944894, -334.5544118177253381 ) ) ;
#82581 = CARTESIAN_POINT ( 'NONE',  ( -112.3500599257388473, -292.1619313333140440, -255.7205636520275505 ) ) ;
#82582 = CARTESIAN_POINT ( 'NONE',  ( -98.81838416704960082, -292.4768482241271386, -224.7989022750655579 ) ) ;
#82583 = CARTESIAN_POINT ( 'NONE',  ( 27.15707567323472560, -293.8525071746819322, -304.6584254100509384 ) ) ;
#82584 = CARTESIAN_POINT ( 'NONE',  ( 35.65334380386608615, -289.7734966758292785, -287.5868027192905743 ) ) ;
#82585 = CARTESIAN_POINT ( 'NONE',  ( 24.59047896289302315, -281.1107767252492522, -224.6073728072628626 ) ) ;
#82586 = CARTESIAN_POINT ( 'NONE',  ( -112.8977929396748152, -294.6417942402715653, -269.5923304998602248 ) ) ;
#82587 = CARTESIAN_POINT ( 'NONE',  ( -63.91400756646391557, -283.2226280652972719, -342.6308383494057921 ) ) ;
#82588 = CARTESIAN_POINT ( 'NONE',  ( 37.01431119181969365, -277.4401703778087835, -263.2392892275520921 ) ) ;
#82589 = CARTESIAN_POINT ( 'NONE',  ( -1.891800215404187080, -284.5216069148665952, -204.2679621557210226 ) ) ;
#82590 = CARTESIAN_POINT ( 'NONE',  ( -17.70129934298482510, -274.9410343472310956, -343.5359779752348572 ) ) ;
#82591 = DIRECTION ( 'NONE',  ( 0.000000000000000000, 0.000000000000000000, 1.000000000000000000 ) ) ;
#82592 = CARTESIAN_POINT ( 'NONE',  ( 7.827089652886396465, -281.9239375541179129, -327.8519300419252431 ) ) ;
#82593 = CARTESIAN_POINT ( 'NONE',  ( -97.39522090471874094, -280.3968677798985709, -222.8050104575527541 ) ) ;
#82594 = CARTESIAN_POINT ( 'NONE',  ( 11.93574416855805964, -285.7761448799196842, -211.4312863813052275 ) ) ;
#82595 = CARTESIAN_POINT ( 'NONE',  ( -38.33369865619360439, -296.8248972015235267, -344.3678065667407964 ) ) ;
#82596 = CARTESIAN_POINT ( 'NONE',  ( 25.41968024469691656, -277.7297915252465828, -313.6664750327792035 ) ) ;
#82597 = CARTESIAN_POINT ( 'NONE',  ( 39.06077961077273386, -276.8055662932858922, -265.4546053573145628 ) ) ;
#82598 = CARTESIAN_POINT ( 'NONE',  ( -109.0436849915936932, -278.2038091855637276, -284.1321152679568058 ) ) ;
#82599 = CARTESIAN_POINT ( 'NONE',  ( -37.86015303360545659, -300.0458004339149056, -195.5295762530892603 ) ) ;
#82600 = CARTESIAN_POINT ( 'NONE',  ( -8.770429384935741979, -284.4266351339829839, -201.1828923952035950 ) ) ;
#82601 = CARTESIAN_POINT ( 'NONE',  ( 39.21557064413320859, -293.3256510229967375, -278.8967413848646970 ) ) ;
#82602 = CARTESIAN_POINT ( 'NONE',  ( -80.07494018488009146, -291.2197485293272052, -333.5145528107659061 ) ) ;
#82603 = CARTESIAN_POINT ( 'NONE',  ( -32.12160937787644599, -291.0398354033779924, -197.2254196230580874 ) ) ;
#82604 = EDGE_LOOP ( 'NONE', ( #69033, #75612, #38583, #87004 ) ) ;
#82605 = CARTESIAN_POINT ( 'NONE',  ( 30.84965138493864956, -292.8701859719204776, -244.2454700766830911 ) ) ;
#82606 = ORIENTED_EDGE ( 'NONE', *, *, #57340, .T. ) ;
#82607 = CARTESIAN_POINT ( 'NONE',  ( -69.21623923897220720, -290.5413702480978486, -340.1286633109422155 ) ) ;
#82608 = CARTESIAN_POINT ( 'NONE',  ( -34.31740431005579950, -280.7425553907566496, -197.3092092615671049 ) ) ;
#82609 = CARTESIAN_POINT ( 'NONE',  ( -70.58257500928206696, -296.5443779058055043, -201.2486245488751706 ) ) ;
#82610 = CARTESIAN_POINT ( 'NONE',  ( 23.77536475374988001, -287.5802677178115232, -223.6702998242654417 ) ) ;
#82611 = CARTESIAN_POINT ( 'NONE',  ( 38.65479868520689166, -288.0428418929850523, -282.9440296418400180 ) ) ;
#82612 = CARTESIAN_POINT ( 'NONE',  ( -97.54737581831494708, -284.3093522370493247, -311.7694993780186223 ) ) ;
#82613 = CARTESIAN_POINT ( 'NONE',  ( -108.0627147292182570, -262.2579186427456648, -317.5738021120234862 ) ) ;
#82614 = CARTESIAN_POINT ( 'NONE',  ( 195.4949434911534922, 284.6999941648707022, -111.1574007831435154 ) ) ;
#82615 = CARTESIAN_POINT ( 'NONE',  ( -63.17214948145560527, -182.5205970719807738, -358.6122145540047086 ) ) ;
#82616 = CARTESIAN_POINT ( 'NONE',  ( -87.21305541279318163, -276.9660883578187622, -323.8910128888574604 ) ) ;
#82617 = CARTESIAN_POINT ( 'NONE',  ( 22.71118079196729411, -275.0574298264636468, -312.4943834877149129 ) ) ;
#82618 = CARTESIAN_POINT ( 'NONE',  ( -70.11890833012333246, -273.2988161754577732, -200.6947246028664438 ) ) ;
#82619 = CARTESIAN_POINT ( 'NONE',  ( -11.41673792228423601, -92.95531928750351369, -356.8092562351845345 ) ) ;
#82620 = CARTESIAN_POINT ( 'NONE',  ( -5.505355017525573658, -275.3268730155184585, -339.9293967055468215 ) ) ;
#82621 = ORIENTED_EDGE ( 'NONE', *, *, #64250, .F. ) ;
#82622 = CARTESIAN_POINT ( 'NONE',  ( -53.41597137761358027, -289.7563088466230852, -341.6324743976787772 ) ) ;
#82623 = CARTESIAN_POINT ( 'NONE',  ( -103.7154863750676697, -297.8609436063642306, -231.5434584901159667 ) ) ;
#82624 = CARTESIAN_POINT ( 'NONE',  ( -110.2853717116281445, -296.7361208981710092, -294.8304391642227529 ) ) ;
#82625 = CARTESIAN_POINT ( 'NONE',  ( -39.68691106817787784, -295.2490684964203069, -343.3358674342650829 ) ) ;
#82626 = ORIENTED_EDGE ( 'NONE', *, *, #91723, .F. ) ;
#82627 = CARTESIAN_POINT ( 'NONE',  ( -99.27099385811067123, -279.8890961074330335, -313.6517263983822090 ) ) ;
#82628 = CARTESIAN_POINT ( 'NONE',  ( 39.64889698460557810, -281.0544958251629168, -269.9368704188668175 ) ) ;
#82629 = CARTESIAN_POINT ( 'NONE',  ( -108.1151075438105948, -279.3804103635697516, -289.4752718236618421 ) ) ;
#82630 = CARTESIAN_POINT ( 'NONE',  ( -23.10646233388825266, -278.6327681548443707, -345.0559482293683686 ) ) ;
#82631 = CARTESIAN_POINT ( 'NONE',  ( -96.56380144823381784, -295.7344619146651326, -226.6578447667980640 ) ) ;
#82632 = CARTESIAN_POINT ( 'NONE',  ( 198.3009384528458270, 65.29331921385960413, -9.735304354939227522 ) ) ;
#82633 = CARTESIAN_POINT ( 'NONE',  ( -102.1568603758254312, -279.1769078233310211, -236.6654606890924697 ) ) ;
#82634 = CARTESIAN_POINT ( 'NONE',  ( -94.03305062971648454, -274.0620831594770266, -218.4740720280185542 ) ) ;
#82635 = CARTESIAN_POINT ( 'NONE',  ( -51.60985992745454354, -287.9158295728792609, -345.5257232660986801 ) ) ;
#82636 = CARTESIAN_POINT ( 'NONE',  ( -11.07262430503478967, -276.3945657468199784, -200.0567740324949852 ) ) ;
#82637 = CARTESIAN_POINT ( 'NONE',  ( 37.60089007749757428, -274.3147539457711446, -285.2679777379279926 ) ) ;
#82638 = FACE_OUTER_BOUND ( 'NONE', #66434, .T. ) ;
#82639 = CARTESIAN_POINT ( 'NONE',  ( -107.1091775830442003, -289.4560039153885782, -292.5537591798423591 ) ) ;
#82640 = CARTESIAN_POINT ( 'NONE',  ( -87.67694735806045969, -284.7195231201136494, -212.1556522290955229 ) ) ;
#82641 = EDGE_CURVE ( 'NONE', #77260, #19571, #74823, .T. ) ;
#82642 = CARTESIAN_POINT ( 'NONE',  ( 12.58394688920153826, -280.5845251003603948, -324.9999666293288669 ) ) ;
#82644 = CARTESIAN_POINT ( 'NONE',  ( -97.72894036780775195, -283.2292077500413825, -226.8112825950305478 ) ) ;
#82643 = CARTESIAN_POINT ( 'NONE',  ( 30.87399498264696973, -280.4935849232745682, -297.9653541863594910 ) ) ;
#82645 = CARTESIAN_POINT ( 'NONE',  ( -24.29099974948256957, -290.8858280170737771, -344.2688895372364186 ) ) ;
#82646 = CARTESIAN_POINT ( 'NONE',  ( -109.4303925683215652, -279.5753431878352444, -284.2242261654769777 ) ) ;
#82647 = CARTESIAN_POINT ( 'NONE',  ( -104.5910534586188589, -255.9060656293385989, -326.6254513314219139 ) ) ;
#82648 = CARTESIAN_POINT ( 'NONE',  ( -38.73852839177641982, -281.4692759706787228, -346.5483169648414901 ) ) ;
#82649 = CARTESIAN_POINT ( 'NONE',  ( -17.02356063911942030, -296.7901157087697470, -342.6103087162557017 ) ) ;
#82650 = CARTESIAN_POINT ( 'NONE',  ( -107.5674965909905012, -277.1658173271779901, -241.3385143299554727 ) ) ;
#82651 = CARTESIAN_POINT ( 'NONE',  ( -69.65825519134533295, -285.4766550003523093, -338.2403106449377788 ) ) ;
#82652 = CARTESIAN_POINT ( 'NONE',  ( 198.0297899315801260, 67.77535909854674401, 9.842341523430512495 ) ) ;
#82653 = CARTESIAN_POINT ( 'NONE',  ( -37.47405358822830124, -290.9739089115015531, -345.9338338305279308 ) ) ;
#82654 = CARTESIAN_POINT ( 'NONE',  ( 38.39942985181230029, -286.5861810557560148, -257.3437913080956605 ) ) ;
#82655 = CARTESIAN_POINT ( 'NONE',  ( -111.0433154238982780, -289.0132993949669071, -265.6646214354952349 ) ) ;
#82656 = CARTESIAN_POINT ( 'NONE',  ( -48.18343439339133027, -276.2535042660651925, -436.4286699060542674 ) ) ;
#82657 = CARTESIAN_POINT ( 'NONE',  ( 35.84357901833165272, -274.3250249106911838, -277.0811175013301408 ) ) ;
#82658 = CARTESIAN_POINT ( 'NONE',  ( 19.76843211831537772, -292.3532529700270857, -317.7878855092637878 ) ) ;
#82659 = FACE_OUTER_BOUND ( 'NONE', #36042, .T. ) ;
#82660 = DIRECTION ( 'NONE',  ( -0.000000000000000000, -0.000000000000000000, -1.000000000000000000 ) ) ;
#82661 = CARTESIAN_POINT ( 'NONE',  ( 37.67206707051568770, -292.2094440787570875, -284.4188511318005226 ) ) ;
#82662 = CARTESIAN_POINT ( 'NONE',  ( -33.21407053015408906, -287.7049835599435710, -196.6262679367014812 ) ) ;
#82663 = CARTESIAN_POINT ( 'NONE',  ( -84.55285909274054745, -287.9316533694936879, -329.9688450384134057 ) ) ;
#82664 = EDGE_CURVE ( 'NONE', #11917, #37641, #80716, .T. ) ;
#82665 = CARTESIAN_POINT ( 'NONE',  ( -14.39939831981606844, -287.7806520233210676, -200.3861085171127741 ) ) ;
#82666 = CARTESIAN_POINT ( 'NONE',  ( 196.8803347170859865, 20.19615242270636557, -12.49999999999999289 ) ) ;
#82667 = CARTESIAN_POINT ( 'NONE',  ( 18.77906285491499716, -287.6900201410286400, -223.4048200442942971 ) ) ;
#82668 = CARTESIAN_POINT ( 'NONE',  ( 19.12900634803856192, -294.8414104928188522, -220.4470812307741028 ) ) ;
#82669 = DIRECTION ( 'NONE',  ( -0.000000000000000000, -0.000000000000000000, -1.000000000000000000 ) ) ;
#82670 = CARTESIAN_POINT ( 'NONE',  ( 34.47660204158474784, -288.4185554214476497, -243.7126622799101483 ) ) ;
#82671 = CARTESIAN_POINT ( 'NONE',  ( -111.0844966203669770, -276.4220775833927064, -286.8327350287990498 ) ) ;
#82672 = CARTESIAN_POINT ( 'NONE',  ( -45.64311740325929634, -277.4877798357739493, -346.9440955677438865 ) ) ;
#82673 = CARTESIAN_POINT ( 'NONE',  ( -6.452805671416432354, -290.5344860512749392, -201.3892056776026322 ) ) ;
#82674 = CARTESIAN_POINT ( 'NONE',  ( -100.2489854180985134, -279.1397015698619271, -225.9575881967378450 ) ) ;
#82675 = CARTESIAN_POINT ( 'NONE',  ( -93.08972448126661448, -299.2261675601404249, -220.7223772155265920 ) ) ;
#82676 = CARTESIAN_POINT ( 'NONE',  ( -48.18343439339132317, -270.8128065642191018, -505.3008612166128728 ) ) ;
#82677 = CARTESIAN_POINT ( 'NONE',  ( -82.66756569741487226, -283.4324854704220229, -210.6069000886882918 ) ) ;
#82678 = CYLINDRICAL_SURFACE ( 'NONE', #54130, 5.568361562975243650 ) ;
#82679 = CARTESIAN_POINT ( 'NONE',  ( -95.43420940212885739, -276.0497198911135115, -316.5996718223453286 ) ) ;
#82680 = CARTESIAN_POINT ( 'NONE',  ( 34.27374110199472312, -279.2646916449808145, -248.0849148375886557 ) ) ;
#82681 = FACE_OUTER_BOUND ( 'NONE', #1104, .T. ) ;
#82682 = CARTESIAN_POINT ( 'NONE',  ( 7.815040061342853228, -274.9281341120441766, -331.9373103461265941 ) ) ;
#82683 = CARTESIAN_POINT ( 'NONE',  ( -108.9683648724278129, -297.8451196095738851, -287.7442685108308069 ) ) ;
#82684 = CARTESIAN_POINT ( 'NONE',  ( -58.41506468419694187, -282.2385559931179273, -344.1551638674872038 ) ) ;
#82685 = CARTESIAN_POINT ( 'NONE',  ( -106.0306805115512532, -297.8327591180453169, -244.8133516173032547 ) ) ;
#82686 = CARTESIAN_POINT ( 'NONE',  ( -112.4081001270483853, -298.0541567665791831, -255.5175469707473610 ) ) ;
#82687 = CARTESIAN_POINT ( 'NONE',  ( -2.899937073685689093, -274.1874127323891912, -205.9728236695579540 ) ) ;
#82688 = CARTESIAN_POINT ( 'NONE',  ( 27.53513763808576797, -296.0547708550434436, -307.9908478255579212 ) ) ;
#82689 = CARTESIAN_POINT ( 'NONE',  ( 23.28877289939664763, -288.3534731135702032, -317.8475547658508162 ) ) ;
#82690 = CARTESIAN_POINT ( 'NONE',  ( -111.8130237502571589, -276.7948821461369562, -257.5808144914827267 ) ) ;
#82691 = CARTESIAN_POINT ( 'NONE',  ( -114.1877049332714336, -290.4463460359769442, -265.4937213509765570 ) ) ;
#82692 = CARTESIAN_POINT ( 'NONE',  ( 27.23229400141799772, -287.0816336101535171, -305.0176455083908422 ) ) ;
#82693 = CARTESIAN_POINT ( 'NONE',  ( -78.47566196037180930, -289.4987559711255471, -207.5854330217459562 ) ) ;
#82694 = ORIENTED_EDGE ( 'NONE', *, *, #85679, .T. ) ;
#82695 = CARTESIAN_POINT ( 'NONE',  ( 201.2104617360081704, 41.21457449016152452, 9.000000000000000000 ) ) ;
#82696 = CARTESIAN_POINT ( 'NONE',  ( 33.13960303141829655, -287.3160736852578339, -289.7939093406765778 ) ) ;
#82697 = FACE_OUTER_BOUND ( 'NONE', #8091, .T. ) ;
#82698 = CARTESIAN_POINT ( 'NONE',  ( -104.2061576972415651, -285.0013527830554381, -308.1776965268672939 ) ) ;
#82699 = CARTESIAN_POINT ( 'NONE',  ( -34.95568146608258786, -291.1401528551502906, -193.6203917491107518 ) ) ;
#82700 = CARTESIAN_POINT ( 'NONE',  ( 21.34144319582575733, -282.4919482016939014, -221.7532059971955221 ) ) ;
#82701 = CARTESIAN_POINT ( 'NONE',  ( 20.68108636255614741, -282.1896745242881366, -220.4748362914795621 ) ) ;
#82702 = CARTESIAN_POINT ( 'NONE',  ( -40.23648350190087086, -282.9228696131830247, -343.3036997420605871 ) ) ;
#82703 = CARTESIAN_POINT ( 'NONE',  ( -112.2743570698698932, -296.7738131870418101, -252.6383381880629031 ) ) ;
#82704 = CARTESIAN_POINT ( 'NONE',  ( -72.15602567404700096, -274.8970573560998787, -205.5803303280068235 ) ) ;
#82705 = CARTESIAN_POINT ( 'NONE',  ( -55.38609741380400209, -289.8389449761008905, -197.9301403126762295 ) ) ;
#82706 = CARTESIAN_POINT ( 'NONE',  ( -34.45088070096986854, -297.0095029632991555, -197.0525493443111316 ) ) ;
#82707 = ORIENTED_EDGE ( 'NONE', *, *, #35999, .F. ) ;
#82708 = CARTESIAN_POINT ( 'NONE',  ( 153.9133111279456045, 20.47222690886501795, -13.06183683676589524 ) ) ;
#82709 = CARTESIAN_POINT ( 'NONE',  ( -70.84148295216125746, -285.4176892182586016, -336.8515221404543922 ) ) ;
#82710 = CARTESIAN_POINT ( 'NONE',  ( -55.98179343265648811, -296.3664392228982365, -344.7522426580285355 ) ) ;
#82711 = CARTESIAN_POINT ( 'NONE',  ( -108.1294409584828600, -285.4441195427221487, -252.1131477773129745 ) ) ;
#82712 = CARTESIAN_POINT ( 'NONE',  ( 37.36011244662669384, -274.8333051002460365, -288.0942205086595322 ) ) ;
#82713 = CARTESIAN_POINT ( 'NONE',  ( -0.8595405818749501936, -293.1750667910442871, -202.6679512547323156 ) ) ;
#82714 = CARTESIAN_POINT ( 'NONE',  ( 32.72629322408224084, -285.3179313603616265, -241.4006673775781451 ) ) ;
#82715 = CARTESIAN_POINT ( 'NONE',  ( -70.89233285013889940, -291.9548175736801454, -201.0783687903830810 ) ) ;
#82716 = CARTESIAN_POINT ( 'NONE',  ( -90.60527286799126045, -290.1661487132856792, -320.3857224790692158 ) ) ;
#82717 = CARTESIAN_POINT ( 'NONE',  ( 196.2176501911084472, 72.73677621079856692, 11.64780326838285873 ) ) ;
#82718 = CARTESIAN_POINT ( 'NONE',  ( 193.4945526529483004, 275.6671624809070522, -124.0448087994775506 ) ) ;
#82719 = CARTESIAN_POINT ( 'NONE',  ( -97.05009447858296312, -286.7141478988249332, -222.8467475244120521 ) ) ;
#82720 = CARTESIAN_POINT ( 'NONE',  ( -117.3417001280813423, -270.0523547857346784, -270.3292895737509980 ) ) ;
#82721 = ORIENTED_EDGE ( 'NONE', *, *, #22274, .F. ) ;
#82722 = CARTESIAN_POINT ( 'NONE',  ( -33.49369145353480093, -281.9229382103779926, -343.5817960136208171 ) ) ;
#82723 = CARTESIAN_POINT ( 'NONE',  ( -100.2292613782641268, -278.8064742117943524, -225.9663104984124402 ) ) ;
#82724 = CARTESIAN_POINT ( 'NONE',  ( -66.81463839377062186, -281.6652702852802008, -201.5621477225321030 ) ) ;
#82725 = CARTESIAN_POINT ( 'NONE',  ( -87.50854530310770940, -231.0822326819537125, -346.2094061126495035 ) ) ;
#82726 = CARTESIAN_POINT ( 'NONE',  ( 19.33417293193931386, -280.8288916774297945, -321.6874255993433849 ) ) ;
#82727 = CARTESIAN_POINT ( 'NONE',  ( 12.24512182097605439, -284.7659169116992643, -214.4974397944724274 ) ) ;
#82728 = CARTESIAN_POINT ( 'NONE',  ( -36.57621667797722864, -299.8217447531536664, -194.3742189733497412 ) ) ;
#82729 = CARTESIAN_POINT ( 'NONE',  ( -15.56851597490403094, -295.2551345107175393, -340.1561228152332319 ) ) ;
#82730 = ORIENTED_EDGE ( 'NONE', *, *, #35371, .F. ) ;
#82731 = CARTESIAN_POINT ( 'NONE',  ( 31.29489413764245143, -291.8884512872410824, -244.0882916261481910 ) ) ;
#82732 = CARTESIAN_POINT ( 'NONE',  ( -20.14082370990913518, -277.4882817183074621, -345.3653664877197116 ) ) ;
#82733 = CARTESIAN_POINT ( 'NONE',  ( 17.28555423567391003, -274.8595207988013840, -221.8624298593667845 ) ) ;
#82734 = CARTESIAN_POINT ( 'NONE',  ( 18.66802608855529755, -275.1899028931458133, -322.7481686620251935 ) ) ;
#82735 = DIRECTION ( 'NONE',  ( 1.124465274301078281E-16, 1.000000000000000000, -0.000000000000000000 ) ) ;
#82736 = CARTESIAN_POINT ( 'NONE',  ( -92.87566169342767353, -271.2553444005300776, -219.9341805632221565 ) ) ;
#82737 = CARTESIAN_POINT ( 'NONE',  ( 23.57033717333462519, -295.5967514715791253, -316.4949451208443634 ) ) ;
#82738 = DIRECTION ( 'NONE',  ( 1.000000000000000000, 0.000000000000000000, 0.000000000000000000 ) ) ;
#82739 = CARTESIAN_POINT ( 'NONE',  ( -43.43031340896369130, -259.9895260090733586, -498.9919023260428048 ) ) ;
#82740 = CARTESIAN_POINT ( 'NONE',  ( -85.05258610946458475, -284.8088302575832813, -326.0198767863370790 ) ) ;
#82741 = CARTESIAN_POINT ( 'NONE',  ( 31.09889243830337335, -282.8817270379560114, -237.2271233592184103 ) ) ;
#82742 = CARTESIAN_POINT ( 'NONE',  ( -109.6004073896432089, -283.7506106202282012, -281.7573351787241904 ) ) ;
#82743 = CARTESIAN_POINT ( 'NONE',  ( -72.04823335984063704, -275.9189552488670643, -335.5052208242718166 ) ) ;
#82744 = CARTESIAN_POINT ( 'NONE',  ( -13.10406117072809629, -284.5944561863594799, -340.5825965516420979 ) ) ;
#82745 = CARTESIAN_POINT ( 'NONE',  ( -110.9736808483926751, -276.9927348496441368, -273.3676385437074714 ) ) ;
#82746 = CARTESIAN_POINT ( 'NONE',  ( 15.66081065149025520, -275.9036331025588993, -219.6422165792442343 ) ) ;
#82747 = CARTESIAN_POINT ( 'NONE',  ( 156.9431851590352665, 249.5000000000000568, 17.51463615629799975 ) ) ;
#82748 = CARTESIAN_POINT ( 'NONE',  ( -42.42959129426654385, -280.7923453722279419, -193.6912269948513483 ) ) ;
#82749 = EDGE_LOOP ( 'NONE', ( #82134, #7931, #84568 ) ) ;
#82750 = ORIENTED_EDGE ( 'NONE', *, *, #3777, .T. ) ;
#82751 = DIRECTION ( 'NONE',  ( -1.000000000000000000, 0.000000000000000000, 0.000000000000000000 ) ) ;
#82752 = CARTESIAN_POINT ( 'NONE',  ( -84.75860719134092847, -287.2668094311005120, -211.2684585202955247 ) ) ;
#82753 = CARTESIAN_POINT ( 'NONE',  ( -67.37081589559861072, -294.6535087023048618, -337.0895759557257634 ) ) ;
#82754 = CARTESIAN_POINT ( 'NONE',  ( -108.7069508600283427, -289.5367807159792051, -299.0022383218778259 ) ) ;
#82755 = EDGE_CURVE ( 'NONE', #72640, #74021, #55351, .T. ) ;
#82756 = CARTESIAN_POINT ( 'NONE',  ( -6.575102009894068900, -284.7016297095457844, -203.0315949599066698 ) ) ;
#82758 = CARTESIAN_POINT ( 'NONE',  ( -107.9618679548543412, -289.0820992842319015, -248.1652288727090081 ) ) ;
#82757 = CARTESIAN_POINT ( 'NONE',  ( -1.886686672506649787, -285.1058752426429237, -205.8189243368559289 ) ) ;
#82759 = B_SPLINE_CURVE_WITH_KNOTS ( 'NONE', 3,
 ( #68150, #10832, #26460, #39233 ),
 .UNSPECIFIED., .F., .F.,
 ( 4, 4 ),
 ( 3.469446951953613804E-18, 0.0008421770481696917027 ),
 .UNSPECIFIED. ) ;
#82760 = CARTESIAN_POINT ( 'NONE',  ( -99.95603228407691176, -286.2832018467763078, -231.9683527268942953 ) ) ;
#82761 = CARTESIAN_POINT ( 'NONE',  ( -111.7844347963764164, -276.4295217774460980, -279.8992098705120952 ) ) ;
#82762 = CARTESIAN_POINT ( 'NONE',  ( -34.71501785021659003, -287.4195387998131537, -346.5158352187889932 ) ) ;
#82763 = CARTESIAN_POINT ( 'NONE',  ( -59.93241545100775625, -287.7597293104752225, -198.7901258682998105 ) ) ;
#82764 = CARTESIAN_POINT ( 'NONE',  ( 35.71634548336695048, -285.7791524837772954, -288.0945093259146006 ) ) ;
#82765 = CARTESIAN_POINT ( 'NONE',  ( -42.93897668876243756, -284.0656428959548521, -343.4324517478227108 ) ) ;
#82766 = CARTESIAN_POINT ( 'NONE',  ( 21.85966918795955394, -290.1866567733507054, -316.6984390386710970 ) ) ;
#82767 = DIRECTION ( 'NONE',  ( 0.000000000000000000, 0.000000000000000000, -1.000000000000000000 ) ) ;
#82768 = CARTESIAN_POINT ( 'NONE',  ( 195.4583199688989339, 39.99286515677976439, 13.91341927790974431 ) ) ;
#82769 = CARTESIAN_POINT ( 'NONE',  ( -86.54348102956033983, -299.2954201383030863, -212.9466892647377847 ) ) ;
#82770 = CARTESIAN_POINT ( 'NONE',  ( 20.39153895366267477, -278.8910007581684454, -222.4676585399201656 ) ) ;
#82771 = CARTESIAN_POINT ( 'NONE',  ( -66.94377033987781545, -290.8710914066187456, -199.4535989180087370 ) ) ;
#82772 = CARTESIAN_POINT ( 'NONE',  ( -92.42861545285818181, -295.6467252407230148, -221.2503027160147440 ) ) ;
#82773 = CARTESIAN_POINT ( 'NONE',  ( 34.96766585705044861, -280.4100423591858089, -283.5692441020132151 ) ) ;
#82774 = CARTESIAN_POINT ( 'NONE',  ( 23.47107851813291646, -273.0441217582940112, -227.4074676085840849 ) ) ;
#82775 = CARTESIAN_POINT ( 'NONE',  ( -18.07520203310480866, -296.1137166878982043, -341.2839318569509715 ) ) ;
#82776 = CARTESIAN_POINT ( 'NONE',  ( -36.17789667918795260, -296.5463577611643586, -194.0547409687907816 ) ) ;
#82777 = CARTESIAN_POINT ( 'NONE',  ( 37.35691069979294809, -291.9694636143319144, -284.3629889643822253 ) ) ;
#82778 = ADVANCED_FACE ( 'NONE', ( #76649 ), #67150, .F. ) ;
#82779 = CARTESIAN_POINT ( 'NONE',  ( 31.37215227949393537, -294.6284562002351208, -244.0213874712032123 ) ) ;
#82780 = DIRECTION ( 'NONE',  ( -0.000000000000000000, -0.000000000000000000, -1.000000000000000000 ) ) ;
#82781 = CARTESIAN_POINT ( 'NONE',  ( 19.46471694001170860, -293.7039029141920992, -224.2367232595827033 ) ) ;
#82782 = DIRECTION ( 'NONE',  ( -1.000000000000000000, 0.000000000000000000, 0.000000000000000000 ) ) ;
#82784 = CARTESIAN_POINT ( 'NONE',  ( -58.40823811073137506, -295.3322039903329141, -340.2553307431710437 ) ) ;
#82783 = CARTESIAN_POINT ( 'NONE',  ( -64.67949926195328203, -281.4274201874051187, -340.5964669230062896 ) ) ;
#82785 = CARTESIAN_POINT ( 'NONE',  ( -47.25636174880325768, -283.1748236534072589, -346.7201350332435936 ) ) ;
#82786 = CARTESIAN_POINT ( 'NONE',  ( -1.834159632218011149, -282.4389747927017993, -203.6638259229042944 ) ) ;
#82787 = CARTESIAN_POINT ( 'NONE',  ( -111.6996801312540981, -284.4705698404659415, -250.2451169168295451 ) ) ;
#82788 = CARTESIAN_POINT ( 'NONE',  ( -109.5002789043550138, -288.2942020714835394, -290.3807832907983766 ) ) ;
#82789 = DIRECTION ( 'NONE',  ( -0.000000000000000000, 1.000000000000000000, 0.000000000000000000 ) ) ;
#82790 = CARTESIAN_POINT ( 'NONE',  ( 37.73986327910122895, -280.2048168028057944, -284.0522067300307185 ) ) ;
#82791 = CARTESIAN_POINT ( 'NONE',  ( 21.24395799978772814, -287.1419309063351193, -319.8506438687795708 ) ) ;
#82792 = CARTESIAN_POINT ( 'NONE',  ( 207.1704462279909649, 29.87979000412345698, 14.95737379494775077 ) ) ;
#82793 = CARTESIAN_POINT ( 'NONE',  ( -0.3393806837994166603, -296.1519040673607606, -334.2729459834377508 ) ) ;
#82794 = CARTESIAN_POINT ( 'NONE',  ( -8.093261221506073966, -278.1017688909275307, -340.9666196044255457 ) ) ;
#82795 = CARTESIAN_POINT ( 'NONE',  ( -11.73175743242412317, -280.0615956521529029, -201.9247634153635431 ) ) ;
#82796 = CARTESIAN_POINT ( 'NONE',  ( 32.18505200082140760, -293.2932708431480364, -237.1459647922381748 ) ) ;
#82797 = CARTESIAN_POINT ( 'NONE',  ( -67.89562980136560100, -283.7341030547903529, -201.2400554045759691 ) ) ;
#82798 = ADVANCED_FACE ( 'NONE', ( #11774, #48684 ), #25064, .F. ) ;
#82799 = CARTESIAN_POINT ( 'NONE',  ( -98.81132755655988831, -279.9690896055897724, -313.3318702873985444 ) ) ;
#82800 = CARTESIAN_POINT ( 'NONE',  ( 35.14232812948045392, -292.4733153081567139, -259.8981310393356239 ) ) ;
#82801 = CARTESIAN_POINT ( 'NONE',  ( 6.552430141662815899, -296.6014479846594440, -195.3760751224127148 ) ) ;
#82802 = ORIENTED_EDGE ( 'NONE', *, *, #8182, .T. ) ;
#82803 = CARTESIAN_POINT ( 'NONE',  ( 197.8477145984406889, 64.61450673763175701, -7.741079165001063522 ) ) ;
#82804 = CARTESIAN_POINT ( 'NONE',  ( 20.56814955047110516, -293.6864495690679178, -314.9286281643392726 ) ) ;
#82805 = CARTESIAN_POINT ( 'NONE',  ( 175.2296996224750103, 149.6461846693799487, 24.00000000000001066 ) ) ;
#82806 = CARTESIAN_POINT ( 'NONE',  ( -67.74223827176246004, -286.9809262143061233, -333.4151289067050357 ) ) ;
#82807 = CARTESIAN_POINT ( 'NONE',  ( 75.96719185516560913, -298.4969465617371043, -193.6139409516525234 ) ) ;
#82808 = CARTESIAN_POINT ( 'NONE',  ( -63.05157882450594542, -287.0393651260587831, -198.3034993037626350 ) ) ;
#82809 = CARTESIAN_POINT ( 'NONE',  ( 10.11365232749199983, -288.2099638290789585, -325.8985728698052071 ) ) ;
#82810 = CARTESIAN_POINT ( 'NONE',  ( -110.9720947877023605, -280.0324894246721783, -273.4062342281841325 ) ) ;
#82811 = CARTESIAN_POINT ( 'NONE',  ( -104.6493277493149634, -298.7232165756729501, -239.4536348703825013 ) ) ;
#82812 = CARTESIAN_POINT ( 'NONE',  ( -104.8010204009342772, -277.7334801601004415, -241.4410451597475458 ) ) ;
#82813 = ORIENTED_EDGE ( 'NONE', *, *, #80432, .T. ) ;
#82814 = CARTESIAN_POINT ( 'NONE',  ( -95.55232274525623382, -296.9001860716596184, -219.9102700484123432 ) ) ;
#82815 = CARTESIAN_POINT ( 'NONE',  ( -106.0412880239350102, -292.8509435957824394, -241.5618981299570862 ) ) ;
#82816 = CARTESIAN_POINT ( 'NONE',  ( 37.27433847888814711, -294.9561397021130915, -254.8412711491692733 ) ) ;
#82817 = CARTESIAN_POINT ( 'NONE',  ( 199.2296996224750103, 68.12454877777268791, -4.263256414560601746E-14 ) ) ;
#82818 = CARTESIAN_POINT ( 'NONE',  ( -103.6522603921755632, -291.6183337501316259, -239.5909658007630867 ) ) ;
#82819 = CARTESIAN_POINT ( 'NONE',  ( -48.18343439339133027, -254.9491769968546464, -455.0632279659918140 ) ) ;
#82820 = CARTESIAN_POINT ( 'NONE',  ( -37.76398388588894051, -290.1865063346749594, -194.5974910816274814 ) ) ;
#82821 = CARTESIAN_POINT ( 'NONE',  ( -114.2801616667020568, -273.0444201233731860, -270.3673729185637171 ) ) ;
#82822 = CARTESIAN_POINT ( 'NONE',  ( 8.949707485552313102, -298.3140883898317384, -197.3426842153452867 ) ) ;
#82823 = CARTESIAN_POINT ( 'NONE',  ( 196.9534188175200029, 25.84350552936208700, 12.42857142857141817 ) ) ;
#82824 = CARTESIAN_POINT ( 'NONE',  ( 199.9311642430735105, 312.1715086799357550, 9.103929867429130240 ) ) ;
#82825 = CARTESIAN_POINT ( 'NONE',  ( -84.71891230408671447, -291.2113887296227972, -330.2458053272778784 ) ) ;
#82826 = CARTESIAN_POINT ( 'NONE',  ( -72.02372285203398405, -291.9805209788416391, -342.4524372437778652 ) ) ;
#82827 = CARTESIAN_POINT ( 'NONE',  ( -68.32954631163414660, -287.6443072018306566, -202.2451740420654858 ) ) ;
#82828 = CARTESIAN_POINT ( 'NONE',  ( -16.09638144493141709, -272.3271897830597936, -198.5528820329859343 ) ) ;
#82829 = CARTESIAN_POINT ( 'NONE',  ( 37.14004552369136292, -277.4881418609043067, -271.5847058174951485 ) ) ;
#82830 = CARTESIAN_POINT ( 'NONE',  ( 5.349099744935768896, -290.7142536620367537, -209.3158710174173223 ) ) ;
#82831 = CARTESIAN_POINT ( 'NONE',  ( -94.26682881378687284, -279.7248798894365791, -320.3594700176080892 ) ) ;
#82832 = ORIENTED_EDGE ( 'NONE', *, *, #59261, .F. ) ;
#82833 = CARTESIAN_POINT ( 'NONE',  ( -13.50395444968439129, -282.0830317907792164, -339.5209057938412229 ) ) ;
#82834 = CARTESIAN_POINT ( 'NONE',  ( -72.68594492187368417, -278.5886958296883336, -338.4365937331575083 ) ) ;
#82835 = CARTESIAN_POINT ( 'NONE',  ( 36.09360050014341681, -280.6240876018016479, -292.3440534225474039 ) ) ;
#82836 = CARTESIAN_POINT ( 'NONE',  ( 200.9738562183072474, 293.9635619827958521, -68.33775802212525718 ) ) ;
#82837 = CARTESIAN_POINT ( 'NONE',  ( 37.01383218315248769, -276.7329161312991346, -289.4418681884037028 ) ) ;
#82838 = EDGE_CURVE ( 'NONE', #59807, #55580, #53936, .T. ) ;
#82839 = SHAPE_DEFINITION_REPRESENTATION ( #33796, #49383 ) ;
#82840 = CARTESIAN_POINT ( 'NONE',  ( -83.17920394262922912, -274.9576867143214258, -209.2898013239136503 ) ) ;
#82841 = CARTESIAN_POINT ( 'NONE',  ( -4.771743288812468897, -297.1233781216987495, -337.9199732462171255 ) ) ;
#82842 = ORIENTED_EDGE ( 'NONE', *, *, #72401, .F. ) ;
#82843 = ORIENTED_EDGE ( 'NONE', *, *, #43223, .F. ) ;
#82844 = AXIS2_PLACEMENT_3D ( 'NONE', #27265, #55685, #78397 ) ;
#82845 = CARTESIAN_POINT ( 'NONE',  ( 185.8264795993290193, 275.0000000000000568, 23.09031830825835385 ) ) ;
#82846 = CARTESIAN_POINT ( 'NONE',  ( -107.2426829067761531, -291.3382042320095593, -292.6214190276682530 ) ) ;
#82847 = CARTESIAN_POINT ( 'NONE',  ( 17.60306940398386999, -288.5842140994150782, -217.7967233374841953 ) ) ;
#82848 = CARTESIAN_POINT ( 'NONE',  ( -98.20012630852826874, -289.3390732673936441, -310.8826094177516666 ) ) ;
#82849 = CARTESIAN_POINT ( 'NONE',  ( -76.07031722933484730, -285.0572425008053301, -203.8195384250526274 ) ) ;
#82850 = DIRECTION ( 'NONE',  ( 0.000000000000000000, 0.000000000000000000, 1.000000000000000000 ) ) ;
#82851 = CARTESIAN_POINT ( 'NONE',  ( -40.28645832146423089, -281.4896529617341798, -344.1023467206119903 ) ) ;
#82852 = CARTESIAN_POINT ( 'NONE',  ( 29.91928312765815434, -288.9954272338254100, -238.9473374250240454 ) ) ;
#82853 = CARTESIAN_POINT ( 'NONE',  ( -10.74342010822718052, -281.1788777656065577, -339.1410272446179306 ) ) ;
#82854 = CARTESIAN_POINT ( 'NONE',  ( -51.94160243309939773, -281.1767062965874402, -198.2806642820031016 ) ) ;
#82855 = CARTESIAN_POINT ( 'NONE',  ( 38.05681653991658209, -288.3125280606246861, -255.9429385616485604 ) ) ;
#82856 = CARTESIAN_POINT ( 'NONE',  ( -108.9488124987978210, -279.2365199699106029, -255.7927547593441489 ) ) ;
#82857 = CARTESIAN_POINT ( 'NONE',  ( -113.4210864942452162, -289.2291710279001222, -279.7403461860976677 ) ) ;
#82858 = CARTESIAN_POINT ( 'NONE',  ( -106.8552068454959283, -284.9347005174121250, -303.1030055861094183 ) ) ;
#82859 = CARTESIAN_POINT ( 'NONE',  ( 25.49122324765116687, -287.4561764159402060, -225.9362590690421655 ) ) ;
#82860 = CARTESIAN_POINT ( 'NONE',  ( -106.9852210808287225, -284.4288143238493376, -292.2421598638657088 ) ) ;
#82861 = VERTEX_POINT ( 'NONE', #34505 ) ;
#82862 = DIRECTION ( 'NONE',  ( -0.000000000000000000, -1.000000000000000000, -0.000000000000000000 ) ) ;
#82863 = CARTESIAN_POINT ( 'NONE',  ( -67.85342050438482886, -293.5163700382292973, -200.9975711372078990 ) ) ;
#82864 = CARTESIAN_POINT ( 'NONE',  ( 38.11709185191537586, -292.3968304082155214, -283.0605761411659955 ) ) ;
#82865 = CARTESIAN_POINT ( 'NONE',  ( 32.28925653025581255, -274.3088159758841584, -247.5056463809646914 ) ) ;
#82866 = CARTESIAN_POINT ( 'NONE',  ( -96.43841348009480896, -295.2378757575384611, -319.5841488532150265 ) ) ;
#82867 = CARTESIAN_POINT ( 'NONE',  ( -107.2226762753320628, -289.3398327128709866, -246.9654575967048231 ) ) ;
#82868 = CARTESIAN_POINT ( 'NONE',  ( -95.58454925547236769, -294.1568676487491416, -316.0310702710178816 ) ) ;
#82869 = CARTESIAN_POINT ( 'NONE',  ( -67.98086079002540316, -292.8457912551282902, -203.6511879908065055 ) ) ;
#82870 = CARTESIAN_POINT ( 'NONE',  ( 209.0052894622294843, 36.56177042507920305, 14.71714099304908885 ) ) ;
#82871 = CARTESIAN_POINT ( 'NONE',  ( 32.76242524983368298, -291.1984148614406536, -243.0981544195494450 ) ) ;
#82872 = CARTESIAN_POINT ( 'NONE',  ( 35.79085035455404551, -295.3380261309167167, -253.6722784129947854 ) ) ;
#82873 = CARTESIAN_POINT ( 'NONE',  ( 18.01122167145736341, -289.1752535489105753, -318.3897726907940182 ) ) ;
#82874 = CARTESIAN_POINT ( 'NONE',  ( -59.16407481432300131, -279.3131125422462446, -342.4873321041928307 ) ) ;
#82875 = CARTESIAN_POINT ( 'NONE',  ( -103.2719060889329370, -276.8351851906664933, -309.4679511510514658 ) ) ;
#82876 = CARTESIAN_POINT ( 'NONE',  ( -114.0786925784668426, -271.9725663770910273, -264.6255720052324705 ) ) ;
#82877 = CARTESIAN_POINT ( 'NONE',  ( -90.48480492610471515, -277.3726647232768983, -218.1620475782953861 ) ) ;
#82878 = CARTESIAN_POINT ( 'NONE',  ( -62.16484288454407192, -275.7693996101311313, -342.4602504512316727 ) ) ;
#82879 = CARTESIAN_POINT ( 'NONE',  ( -72.37430366501205015, -294.2107920970579471, -334.9816778319416244 ) ) ;
#82880 = CARTESIAN_POINT ( 'NONE',  ( 201.2104617360081704, 250.0000000000000568, -15.00000000000000000 ) ) ;
#82881 = CARTESIAN_POINT ( 'NONE',  ( -47.30483389811862338, -298.7252911876861958, -197.8298809920019607 ) ) ;
#82882 = CYLINDRICAL_SURFACE ( 'NONE', #64053, 7.500000000000007105 ) ;
#82884 = CARTESIAN_POINT ( 'NONE',  ( -14.06343239113549082, -274.1960378574045194, -201.1720852124626617 ) ) ;
#82883 = CARTESIAN_POINT ( 'NONE',  ( -37.52348523585912687, -287.0744941639107424, -345.7288951395824483 ) ) ;
#82885 = CARTESIAN_POINT ( 'NONE',  ( 38.10828887158677247, -287.7444005567593308, -285.7331432216089979 ) ) ;
#82886 = CARTESIAN_POINT ( 'NONE',  ( -111.7337341645214224, -274.6947677405504464, -259.2417493320547806 ) ) ;
#82887 = CARTESIAN_POINT ( 'NONE',  ( -110.6865639051041370, -294.3600576711411918, -285.2762801390736627 ) ) ;
#82888 = CARTESIAN_POINT ( 'NONE',  ( -79.08060362343434235, -282.7970449268407265, -334.8748588072818961 ) ) ;
#82889 = CYLINDRICAL_SURFACE ( 'NONE', #54719, 1.000000000000000888 ) ;
#82890 = CARTESIAN_POINT ( 'NONE',  ( -110.4912698441195857, -276.7652465324424611, -253.7470599693036775 ) ) ;
#82891 = CARTESIAN_POINT ( 'NONE',  ( -92.84677292810179949, -290.0277077080850177, -222.3369844751966298 ) ) ;
#82892 = EDGE_CURVE ( 'NONE', #38685, #19715, #21803, .T. ) ;
#82893 = CARTESIAN_POINT ( 'NONE',  ( 198.1257640572240177, 41.66869203097355268, 11.52974254711191726 ) ) ;
#82894 = PLANE ( 'NONE',  #42771 ) ;
#82895 = CARTESIAN_POINT ( 'NONE',  ( -93.14465668288772804, -289.2502622911157459, -220.2317313248454980 ) ) ;
#82896 = CARTESIAN_POINT ( 'NONE',  ( 25.86059285657968587, -276.5547126012588137, -232.3653812212576781 ) ) ;
#82897 = CARTESIAN_POINT ( 'NONE',  ( 39.12071280703885634, -282.9718067455380037, -269.9154489091039864 ) ) ;
#82899 = CARTESIAN_POINT ( 'NONE',  ( -109.4983578076280537, -284.4019186885770409, -281.7496367240956374 ) ) ;
#82898 = CARTESIAN_POINT ( 'NONE',  ( -37.23015791734167834, -296.0736571015398226, -195.0051995546122896 ) ) ;
#82900 = CARTESIAN_POINT ( 'NONE',  ( -69.76681120801868019, -275.0418136991972347, -204.3006374325418051 ) ) ;
#82901 = CARTESIAN_POINT ( 'NONE',  ( 19.97564167922274336, -275.7143841713226493, -224.8732406555960495 ) ) ;
#82902 = ADVANCED_FACE ( 'NONE', ( #13668 ), #56286, .F. ) ;
#82903 = CARTESIAN_POINT ( 'NONE',  ( -38.67088039133047062, -285.0689823389383264, -345.3493432741486231 ) ) ;
#82905 = CARTESIAN_POINT ( 'NONE',  ( -103.4780545064313344, -271.8984004651559871, -238.7350416819934935 ) ) ;
#82904 = VECTOR ( 'NONE', #61832, 1000.000000000000000 ) ;
#82906 = EDGE_LOOP ( 'NONE', ( #67125, #44668 ) ) ;
#82907 = CARTESIAN_POINT ( 'NONE',  ( 204.5657207964215445, 292.7458577622498979, -53.99999999999736389 ) ) ;
#82908 = CARTESIAN_POINT ( 'NONE',  ( 30.90136434622678152, -293.8455866754657109, -306.0246028885624128 ) ) ;
#82909 = CARTESIAN_POINT ( 'NONE',  ( -101.8092751909148745, -286.0269856118743519, -307.9879510425555509 ) ) ;
#82910 = DIRECTION ( 'NONE',  ( -0.5729786897769871823, -0.000000000000000000, -0.8195702660915947790 ) ) ;
#82911 = CARTESIAN_POINT ( 'NONE',  ( -37.30987171927208834, -277.5523547857346784, -190.3611179825600175 ) ) ;
#82912 = CARTESIAN_POINT ( 'NONE',  ( -35.72517803117905544, -276.2295613201834499, -347.1957324716757967 ) ) ;
#82913 = CARTESIAN_POINT ( 'NONE',  ( -80.10864855193611334, -288.0200071071984667, -333.4917299870747911 ) ) ;
#82914 = CARTESIAN_POINT ( 'NONE',  ( -78.75038536192575123, -285.1415307291730414, -331.3203546768234560 ) ) ;
#82915 = CARTESIAN_POINT ( 'NONE',  ( -93.48081967303208728, -279.6349510195247490, -318.5936098536361101 ) ) ;
#82916 = CARTESIAN_POINT ( 'NONE',  ( -78.22265636648576503, -286.9390093056048840, -205.8060739570703390 ) ) ;
#82917 = CARTESIAN_POINT ( 'NONE',  ( 21.22217843365140766, -282.9079775522235991, -223.5073798014388444 ) ) ;
#82918 = CARTESIAN_POINT ( 'NONE',  ( -45.64750751806379725, -277.3212055509485481, -346.9649018755663974 ) ) ;
#82919 = CARTESIAN_POINT ( 'NONE',  ( -71.57275758701008783, -277.3252158139546282, -339.3338278740602618 ) ) ;
#82920 = CARTESIAN_POINT ( 'NONE',  ( -37.85654053871942892, -299.9658069587518980, -195.9228943259563493 ) ) ;
#82921 = CARTESIAN_POINT ( 'NONE',  ( 185.8264795993290477, 214.9910457053126720, 23.09031830825835385 ) ) ;
#82922 = CARTESIAN_POINT ( 'NONE',  ( -37.37352853689063892, -282.5519495502701943, -195.3611179825600175 ) ) ;
#82923 = CARTESIAN_POINT ( 'NONE',  ( -37.57961816093836660, -296.1887933535771822, -194.5966878062021408 ) ) ;
#82924 = DIRECTION ( 'NONE',  ( 0.000000000000000000, 1.000000000000000000, 0.000000000000000000 ) ) ;
#82925 = CARTESIAN_POINT ( 'NONE',  ( -107.8813114569306748, -277.8086458707166457, -289.3914010959801999 ) ) ;
#82926 = CARTESIAN_POINT ( 'NONE',  ( 19.72972639834207698, -276.0599043855773971, -219.1866000003836348 ) ) ;
#82927 = CARTESIAN_POINT ( 'NONE',  ( 2.980564240251267982, -288.3618441425858236, -208.2959183258687688 ) ) ;
#82928 = ADVANCED_FACE ( 'NONE', ( #64820 ), #79259, .T. ) ;
#82929 = CARTESIAN_POINT ( 'NONE',  ( -111.9269719779286305, -298.2763813322272313, -254.1834513782348495 ) ) ;
#82930 = CARTESIAN_POINT ( 'NONE',  ( -71.88119407151741314, -296.7036348078074184, -338.7353242168666156 ) ) ;
#82931 = CARTESIAN_POINT ( 'NONE',  ( -41.72506823871402304, -293.9970988160546881, -195.6051711001187812 ) ) ;
#82932 = CARTESIAN_POINT ( 'NONE',  ( -97.05976604789536566, -277.1702440471496516, -225.2423953955258185 ) ) ;
#82933 = CARTESIAN_POINT ( 'NONE',  ( -37.02629225820091818, -281.9762850454551426, -195.9217821460108837 ) ) ;
#82934 = CARTESIAN_POINT ( 'NONE',  ( -99.63954569464875988, -295.1868963525335516, -229.5211940012381149 ) ) ;
#82935 = CARTESIAN_POINT ( 'NONE',  ( -71.16569700766235940, -285.3542770351278364, -338.1567131140929519 ) ) ;
#82936 = CARTESIAN_POINT ( 'NONE',  ( 7.125291890327223321, -285.5941405984553398, -212.0139310223021312 ) ) ;
#82937 = CARTESIAN_POINT ( 'NONE',  ( -102.1811274640376865, -256.8422514774185288, -326.3129529855307851 ) ) ;
#82938 = EDGE_LOOP ( 'NONE', ( #63521, #3794 ) ) ;
#82939 = CARTESIAN_POINT ( 'NONE',  ( 33.05077913577997606, -286.9623839932718283, -250.9449816543256020 ) ) ;
#82940 = ORIENTED_EDGE ( 'NONE', *, *, #12809, .T. ) ;
#82941 = CARTESIAN_POINT ( 'NONE',  ( -81.37279428861049269, -284.7148439251893137, -333.2170790613274676 ) ) ;
#82942 = CARTESIAN_POINT ( 'NONE',  ( -5.302608857870863446, -274.8190544746449859, -204.7303404095251551 ) ) ;
#82943 = CARTESIAN_POINT ( 'NONE',  ( 38.39532273392931927, -286.2015967047595382, -258.7883699367978920 ) ) ;
#82944 = CARTESIAN_POINT ( 'NONE',  ( -50.49974841359250632, -290.8082246478630850, -194.8074398836162686 ) ) ;
#82945 = CARTESIAN_POINT ( 'NONE',  ( 39.29509305955217968, -282.5595336807039075, -275.6327610395879333 ) ) ;
#82946 = CARTESIAN_POINT ( 'NONE',  ( -35.37348967407040590, -281.5965192417962726, -194.0668177912773729 ) ) ;
#82947 = CARTESIAN_POINT ( 'NONE',  ( 26.26074999568484358, -281.3122758400177190, -226.9036998771602498 ) ) ;
#82948 = CARTESIAN_POINT ( 'NONE',  ( -82.13390479932374433, -287.1952119285918457, -326.4764044574609443 ) ) ;
#82949 = CARTESIAN_POINT ( 'NONE',  ( 200.5823919207504957, 289.1423781782043534, -97.54666654485188815 ) ) ;
#82950 = ORIENTED_EDGE ( 'NONE', *, *, #77701, .F. ) ;
#82951 = CARTESIAN_POINT ( 'NONE',  ( 29.68361825208949512, -277.9938789039737799, -303.7591681900066192 ) ) ;
#82952 = CARTESIAN_POINT ( 'NONE',  ( 202.6186562182569446, 295.9433822784108656, -54.00000000003930722 ) ) ;
#82953 = CARTESIAN_POINT ( 'NONE',  ( 21.83500341415685142, -278.9458730661058325, -224.8434706309899980 ) ) ;
#82954 = CARTESIAN_POINT ( 'NONE',  ( -27.85186621224607606, -296.6935120600264213, -345.8054672735639770 ) ) ;
#82955 = CARTESIAN_POINT ( 'NONE',  ( -86.56472507778320846, -295.1066510823423528, -324.4072693970779255 ) ) ;
#82956 = CARTESIAN_POINT ( 'NONE',  ( -99.97730205154380201, -290.6520775086311232, -225.6810522372269929 ) ) ;
#82957 = FACE_OUTER_BOUND ( 'NONE', #58674, .T. ) ;
#82958 = EDGE_CURVE ( 'NONE', #52628, #88979, #5630, .T. ) ;
#82960 = CARTESIAN_POINT ( 'NONE',  ( 8.460684806095072119, -286.8126780845325356, -328.2280510906520021 ) ) ;
#82959 = CARTESIAN_POINT ( 'NONE',  ( -107.2267193329290507, -295.5256344314885268, -239.3323049370431193 ) ) ;
#82961 = CARTESIAN_POINT ( 'NONE',  ( 36.85515211788651868, -295.3816246364115159, -267.9752021470371801 ) ) ;
#82962 = EDGE_CURVE ( 'NONE', #15639, #18551, #7476, .T. ) ;
#82963 = CARTESIAN_POINT ( 'NONE',  ( -40.00847226590351369, -287.3331214738880135, -196.9163645589655687 ) ) ;
#82964 = ORIENTED_EDGE ( 'NONE', *, *, #45009, .T. ) ;
#82965 = CARTESIAN_POINT ( 'NONE',  ( 36.05847788520018327, -294.2102941850820912, -247.8837053059766333 ) ) ;
#82966 = CARTESIAN_POINT ( 'NONE',  ( -107.4492024774435066, -284.7721154562861443, -290.9709514711556153 ) ) ;
#82967 = CARTESIAN_POINT ( 'NONE',  ( -110.4255970676042722, -295.0566925533191238, -293.3561456304659032 ) ) ;
#82968 = CARTESIAN_POINT ( 'NONE',  ( -114.2284332157901616, -291.3440045306941784, -271.2371421148016566 ) ) ;
#82969 = CARTESIAN_POINT ( 'NONE',  ( -64.37306049884874426, -292.2011410416391755, -198.2714367176935468 ) ) ;
#82970 = CARTESIAN_POINT ( 'NONE',  ( -98.84062306416483068, -290.1748068505127094, -309.6915449088135119 ) ) ;
#82971 = ORIENTED_EDGE ( 'NONE', *, *, #64747, .T. ) ;
#82972 = CARTESIAN_POINT ( 'NONE',  ( 157.0248177074852549, 17.42562647115544650, 9.460300111312282212 ) ) ;
#82973 = CARTESIAN_POINT ( 'NONE',  ( -101.2868036239908776, -298.9538471154485251, -229.7245677050963479 ) ) ;
#82974 = CARTESIAN_POINT ( 'NONE',  ( -109.7216363701928969, -271.6649544303252810, -245.2781845875908289 ) ) ;
#82975 = CARTESIAN_POINT ( 'NONE',  ( -38.90207356077544176, -282.1309129630747634, -343.5923192902827168 ) ) ;
#82976 = ORIENTED_EDGE ( 'NONE', *, *, #47924, .F. ) ;
#82977 = ORIENTED_EDGE ( 'NONE', *, *, #43977, .T. ) ;
#82978 = CARTESIAN_POINT ( 'NONE',  ( 32.49983504887008934, -274.6451257940422011, -237.9590512205796244 ) ) ;
#82979 = CIRCLE ( 'NONE', #42152, 8.000000000000000000 ) ;
#82980 = CARTESIAN_POINT ( 'NONE',  ( -108.6452998610043323, -294.7879861088735538, -289.0256908439316703 ) ) ;
#82981 = CARTESIAN_POINT ( 'NONE',  ( -56.90322168860227237, -279.1673876500581173, -342.0260367288996122 ) ) ;
#82982 = CARTESIAN_POINT ( 'NONE',  ( -24.35748700101493824, -272.3590913321365292, -197.2177809007490339 ) ) ;
#82983 = CARTESIAN_POINT ( 'NONE',  ( -75.42975153439516589, -298.7374008306391033, -207.5612038908421937 ) ) ;
#82984 = CARTESIAN_POINT ( 'NONE',  ( -36.49263605649073838, -299.1426998675393065, -197.0518431955534027 ) ) ;
#82985 = CARTESIAN_POINT ( 'NONE',  ( 208.4306832106270804, -124.2391364535881024, 0.000000000000000000 ) ) ;
#82986 = CARTESIAN_POINT ( 'NONE',  ( -111.8188846858725327, -297.9486585888502077, -286.4728962416030527 ) ) ;
#82987 = CARTESIAN_POINT ( 'NONE',  ( -112.6959634789780154, -270.6084402209360746, -267.5297528916812553 ) ) ;
#82988 = CARTESIAN_POINT ( 'NONE',  ( 21.41333505682168692, -294.8125336984953151, -313.8552383768067671 ) ) ;
#82989 = CARTESIAN_POINT ( 'NONE',  ( 17.18691141796513477, -291.4238177060104817, -220.8697069695756170 ) ) ;
#82990 = CARTESIAN_POINT ( 'NONE',  ( 207.7670128149124196, 29.57000807141141507, 14.83937854961792979 ) ) ;
#82991 = CARTESIAN_POINT ( 'NONE',  ( 15.97987084479417597, -275.2763064673926010, -214.8963816891093188 ) ) ;
#82992 = CARTESIAN_POINT ( 'NONE',  ( -105.4170100565923178, -273.0726969286934036, -243.8635163332248510 ) ) ;
#82993 = CARTESIAN_POINT ( 'NONE',  ( 10.46891458260228625, -284.3761273425995455, -328.6742764961313128 ) ) ;
#82994 = CARTESIAN_POINT ( 'NONE',  ( -19.05262094601881273, -281.5064867038660736, -344.7044000765649230 ) ) ;
#82995 = DIRECTION ( 'NONE',  ( 1.000000000000000000, 0.000000000000000000, 0.000000000000000000 ) ) ;
#82996 = CARTESIAN_POINT ( 'NONE',  ( -100.5457617325614166, -283.2447090212887701, -307.2101115010094645 ) ) ;
#82997 = CARTESIAN_POINT ( 'NONE',  ( -112.5220644747407022, -282.5211962470778531, -272.7645800835308023 ) ) ;
#82998 = CARTESIAN_POINT ( 'NONE',  ( -8.524532518911451362, -275.2421546850213758, -338.0869956019382698 ) ) ;
#82999 = CARTESIAN_POINT ( 'NONE',  ( 37.14632992430246361, -283.6701436698289172, -279.5379070930167700 ) ) ;
#83000 = DIRECTION ( 'NONE',  ( 0.000000000000000000, 0.000000000000000000, 1.000000000000000000 ) ) ;
#83001 = LINE ( 'NONE', #2558, #65536 ) ;
#83002 = CARTESIAN_POINT ( 'NONE',  ( -78.39324101171074233, -271.9093927553378762, -206.1644560332355525 ) ) ;
#83003 = CARTESIAN_POINT ( 'NONE',  ( -112.5501289269125209, -280.5363918658530338, -271.6041192208650159 ) ) ;
#83004 = CARTESIAN_POINT ( 'NONE',  ( 184.8939426562960193, 2.965303559109565334, 10.00000000000000000 ) ) ;
#83005 = CARTESIAN_POINT ( 'NONE',  ( -112.0671467456183734, -286.6194417750330103, -258.8161717505068395 ) ) ;
#83006 = ORIENTED_EDGE ( 'NONE', *, *, #65700, .F. ) ;
#83007 = CARTESIAN_POINT ( 'NONE',  ( 208.9490645430419704, 38.23479348326421956, 12.02378101520620746 ) ) ;
#83008 = CARTESIAN_POINT ( 'NONE',  ( -5.899829542312970965, -286.6387064778318177, -338.4661970954428512 ) ) ;
#83009 = FACE_OUTER_BOUND ( 'NONE', #1918, .T. ) ;
#83010 = CARTESIAN_POINT ( 'NONE',  ( -103.1308485592454076, -294.9069897288606512, -303.0170454538719014 ) ) ;
#83011 = CARTESIAN_POINT ( 'NONE',  ( -78.88494953664221043, -287.7578247875727584, -331.9455625082819665 ) ) ;
#83012 = CARTESIAN_POINT ( 'NONE',  ( 168.1488725781630649, 234.1813984995739588, -193.4213935641190858 ) ) ;
#83013 = CARTESIAN_POINT ( 'NONE',  ( -97.21595800675819987, -293.9342288314658731, -315.5494601618863157 ) ) ;
#83014 = CARTESIAN_POINT ( 'NONE',  ( -15.59237409132607688, -284.8083609738938549, -197.1647500704050913 ) ) ;
#83015 = CARTESIAN_POINT ( 'NONE',  ( -11.48170766011693544, -281.9946934155672125, -201.1861644424373878 ) ) ;
#83016 = CARTESIAN_POINT ( 'NONE',  ( -89.75560929285978773, -282.0189167110928565, -325.4492489382009808 ) ) ;
#83017 = CARTESIAN_POINT ( 'NONE',  ( -86.72937967292880046, -289.7616654799782054, -324.1870839085988223 ) ) ;
#83018 = CARTESIAN_POINT ( 'NONE',  ( -62.52753188734794065, -281.1433267972766430, -201.1621955814928242 ) ) ;
#83019 = CARTESIAN_POINT ( 'NONE',  ( -68.60154206500193652, -280.4332986687152243, -204.2141300721354469 ) ) ;
#83020 = CARTESIAN_POINT ( 'NONE',  ( 28.92847167474525705, -290.0074261846993409, -306.3405109671757600 ) ) ;
#83021 = CARTESIAN_POINT ( 'NONE',  ( -100.7518688048407256, -297.2957874581618967, -226.6555638329493263 ) ) ;
#83022 = VERTEX_POINT ( 'NONE', #71431 ) ;
#83023 = CARTESIAN_POINT ( 'NONE',  ( -3.826106466615454504, -274.4821253856649719, -201.0234172720022627 ) ) ;
#83024 = CARTESIAN_POINT ( 'NONE',  ( -110.9019598376697786, -292.6994204338203076, -257.3873030900396088 ) ) ;
#83025 = DIRECTION ( 'NONE',  ( 0.000000000000000000, 0.000000000000000000, 1.000000000000000000 ) ) ;
#83026 = CARTESIAN_POINT ( 'NONE',  ( 10.59707575819634329, -277.1948066931274184, -210.1954327657594490 ) ) ;
#83027 = VERTEX_POINT ( 'NONE', #70960 ) ;
#83028 = CARTESIAN_POINT ( 'NONE',  ( -7.330646697743163465, -274.6593686421707616, -339.2906697189735610 ) ) ;
#83029 = DIRECTION ( 'NONE',  ( 0.000000000000000000, 1.000000000000000000, 0.000000000000000000 ) ) ;
#83030 = CARTESIAN_POINT ( 'NONE',  ( -8.707763106063518777, -293.0836862690555336, -341.0324289061744025 ) ) ;
#83031 = CARTESIAN_POINT ( 'NONE',  ( 2.993087487901384680, -273.9577666961080809, -209.3334325535352320 ) ) ;
#83032 = CARTESIAN_POINT ( 'NONE',  ( -109.8577604937471506, -291.9008344051939048, -283.4809023799742818 ) ) ;
#83034 = ADVANCED_FACE ( 'NONE', ( #36361 ), #35445, .F. ) ;
#83033 = CARTESIAN_POINT ( 'NONE',  ( 23.42943796244891175, -283.8930458574305362, -312.6085177774449448 ) ) ;
#83035 = CARTESIAN_POINT ( 'NONE',  ( -111.9858188822964138, -291.7715394737080032, -286.6970241632299121 ) ) ;
#83036 = CARTESIAN_POINT ( 'NONE',  ( -107.9187043993905490, -292.2453704535353722, -240.8283439907328045 ) ) ;
#83037 = CARTESIAN_POINT ( 'NONE',  ( 34.32397093922029541, -293.5687509408299434, -284.2546990543729635 ) ) ;
#83038 = CARTESIAN_POINT ( 'NONE',  ( 16.44658606462402517, -288.8167080039955863, -218.0942937371492292 ) ) ;
#83039 = CARTESIAN_POINT ( 'NONE',  ( 13.68237696362719191, -282.5272890713608263, -328.0996179833335873 ) ) ;
#83040 = CARTESIAN_POINT ( 'NONE',  ( -97.08016457353026851, -295.2617128351114388, -224.0733024426773170 ) ) ;
#83041 = CARTESIAN_POINT ( 'NONE',  ( 11.49096128488237412, -282.2299005179619371, -329.9647351284985461 ) ) ;
#83042 = CARTESIAN_POINT ( 'NONE',  ( 35.72633326637648565, -277.3343530123499932, -255.0374513298922921 ) ) ;
#83043 = CARTESIAN_POINT ( 'NONE',  ( -92.05005921254146983, -298.4090924074129703, -314.0302885647153062 ) ) ;
#83044 = CIRCLE ( 'NONE', #86095, 3.000000000000007994 ) ;
#83045 = CARTESIAN_POINT ( 'NONE',  ( -81.84026780938299339, -275.7908411482873134, -331.6814486432688796 ) ) ;
#83046 = DIRECTION ( 'NONE',  ( -1.000000000000000000, 0.000000000000000000, 0.000000000000000000 ) ) ;
#83047 = CARTESIAN_POINT ( 'NONE',  ( -78.41639808493620478, -283.1293856672517109, -330.7834452240858809 ) ) ;
#83048 = CARTESIAN_POINT ( 'NONE',  ( -56.47240186498728320, -281.0161232702524217, -196.1307622278391989 ) ) ;
#83049 = CARTESIAN_POINT ( 'NONE',  ( 39.34329278359203386, -286.5542387049203512, -265.8442266619545649 ) ) ;
#83050 = CARTESIAN_POINT ( 'NONE',  ( -11.93309691514147453, -294.1474676518147362, -200.7911995146945117 ) ) ;
#83051 = CARTESIAN_POINT ( 'NONE',  ( 36.85126141049806847, -276.9320584853339824, -252.9307410571222761 ) ) ;
#83052 = CARTESIAN_POINT ( 'NONE',  ( 38.82465294507983344, -276.7698049657901720, -262.6135236975884482 ) ) ;
#83053 = CARTESIAN_POINT ( 'NONE',  ( -78.63375078936265083, -277.4585620216481630, -330.6220619314908049 ) ) ;
#83054 = CARTESIAN_POINT ( 'NONE',  ( -63.74969564120401344, -299.7073753036743256, -200.2873878286791864 ) ) ;
#83055 = CARTESIAN_POINT ( 'NONE',  ( -33.11014011545605484, -284.1052760850298000, -195.5964455488650344 ) ) ;
#83056 = CARTESIAN_POINT ( 'NONE',  ( -47.73633428001114964, -291.5902842358125326, -194.0335167560572813 ) ) ;
#83057 = CARTESIAN_POINT ( 'NONE',  ( -112.3422361346675586, -291.9811542265598518, -283.9017077909066415 ) ) ;
#83058 = CARTESIAN_POINT ( 'NONE',  ( 35.02127691032686840, -292.3172283709896533, -258.5426149853789752 ) ) ;
#83059 = ORIENTED_EDGE ( 'NONE', *, *, #79909, .T. ) ;
#83060 = CARTESIAN_POINT ( 'NONE',  ( 15.04748646970957360, -291.3482983868901783, -214.6649011981226920 ) ) ;
#83061 = CARTESIAN_POINT ( 'NONE',  ( 21.01325545229452274, -292.6026496572957285, -226.4659400462186341 ) ) ;
#83062 = ORIENTED_EDGE ( 'NONE', *, *, #76588, .T. ) ;
#83063 = CARTESIAN_POINT ( 'NONE',  ( -31.83519022091833151, -290.0640028260339705, -346.9064091881161289 ) ) ;
#83064 = CARTESIAN_POINT ( 'NONE',  ( -66.11745521326328401, -280.3167409480962533, -203.1473952358238364 ) ) ;
#83065 = CARTESIAN_POINT ( 'NONE',  ( -60.04341622400809797, -296.6851199696344565, -197.0519856812748003 ) ) ;
#83066 = CARTESIAN_POINT ( 'NONE',  ( -35.15945291713916276, -286.7302549345412217, -193.4808949795269939 ) ) ;
#83067 = CARTESIAN_POINT ( 'NONE',  ( -7.355283648241591088, -286.7679202101279543, -199.4062489621444456 ) ) ;
#83068 = CARTESIAN_POINT ( 'NONE',  ( -99.62957132219536049, -285.4115477470588189, -232.1556042676293998 ) ) ;
#83069 = CARTESIAN_POINT ( 'NONE',  ( 189.4474627607228001, 271.4776447363245779, -139.5738757705058788 ) ) ;
#83070 = CARTESIAN_POINT ( 'NONE',  ( -79.02728084768597228, -207.4829129746956653, -355.6029576119787521 ) ) ;
#83071 = CARTESIAN_POINT ( 'NONE',  ( -22.36693251778569547, -108.5985266847460622, -358.9081768719106549 ) ) ;
#83072 = CARTESIAN_POINT ( 'NONE',  ( -11.20588496726879946, -275.8997874512112958, -338.6950106925331738 ) ) ;
#83073 = CARTESIAN_POINT ( 'NONE',  ( -4.941793710671096740, -275.5355755799877784, -336.1357850067452091 ) ) ;
#83074 = CARTESIAN_POINT ( 'NONE',  ( -108.8290931161916575, -296.4225312617581949, -241.7736542776215742 ) ) ;
#83075 = CARTESIAN_POINT ( 'NONE',  ( -110.3569350145632484, -272.0556378214883466, -283.7581280487278264 ) ) ;
#83076 = ADVANCED_FACE ( 'NONE', ( #43462 ), #85149, .T. ) ;
#83077 = CARTESIAN_POINT ( 'NONE',  ( -82.27029601463505060, -276.3359953019448199, -332.2862303618889541 ) ) ;
#83078 = CARTESIAN_POINT ( 'NONE',  ( -66.22903647347109768, -275.4288700148807720, -202.2179171935093507 ) ) ;
#83079 = CARTESIAN_POINT ( 'NONE',  ( -107.4561191903716093, -291.3165651887640593, -249.7750975122339696 ) ) ;
#83080 = CARTESIAN_POINT ( 'NONE',  ( -58.79640981861882665, -296.1254943504083599, -344.1990505925075468 ) ) ;
#83081 = CARTESIAN_POINT ( 'NONE',  ( -80.59561074974467942, -297.9754200226536227, -206.6682434208644565 ) ) ;
#83082 = CARTESIAN_POINT ( 'NONE',  ( 19.69509471483855378, -294.3626145774609313, -315.9420383682352735 ) ) ;
#83083 = ORIENTED_EDGE ( 'NONE', *, *, #12828, .F. ) ;
#83084 = CARTESIAN_POINT ( 'NONE',  ( -4.596351126262481657, -278.5443058365432307, -338.4712830068449421 ) ) ;
#83085 = B_SPLINE_CURVE_WITH_KNOTS ( 'NONE', 3,
 ( #23962, #29694, #81254, #37244, #87417, #16399 ),
 .UNSPECIFIED., .F., .F.,
 ( 4, 2, 4 ),
 ( 0.002740393443096640798, 0.004110592855002227590, 0.005480792266907814382 ),
 .UNSPECIFIED. ) ;
#83086 = CARTESIAN_POINT ( 'NONE',  ( 31.96875707627194885, -280.6296010688855631, -236.8381183533995511 ) ) ;
#83087 = CARTESIAN_POINT ( 'NONE',  ( 1.004810213960826593, -277.4683479495817551, -332.8142493194610552 ) ) ;
#83088 = CARTESIAN_POINT ( 'NONE',  ( -6.959009817387207697, -278.4190625673017507, -340.0233484117898684 ) ) ;
#83089 = CARTESIAN_POINT ( 'NONE',  ( 52.59173577772707375, -297.7742714233109496, -196.7942471513891292 ) ) ;
#83090 = CARTESIAN_POINT ( 'NONE',  ( 0.000000000000000000, 3.000000000000000000, 7.000000000000000000 ) ) ;
#83091 = CARTESIAN_POINT ( 'NONE',  ( -108.8876706831409678, -278.9109054952037923, -255.8009551424368908 ) ) ;
#83092 = CARTESIAN_POINT ( 'NONE',  ( 13.84926579877209107, -275.5511103788024343, -212.9869368845743338 ) ) ;
#83093 = CARTESIAN_POINT ( 'NONE',  ( -41.74899674898752977, -287.7913852216785813, -346.7540565012317302 ) ) ;
#83094 = CARTESIAN_POINT ( 'NONE',  ( 0.1723937790587578844, -276.5517316171739139, -205.4024613651931190 ) ) ;
#83095 = CARTESIAN_POINT ( 'NONE',  ( 113.5000000000000568, -192.7866584945343504, -447.4016117689005796 ) ) ;
#83096 = CARTESIAN_POINT ( 'NONE',  ( -98.25076229449304321, -289.1876783259443187, -310.9140157406871481 ) ) ;
#83097 = CARTESIAN_POINT ( 'NONE',  ( -91.82491323006232165, -284.6481593370122027, -216.0942563031399004 ) ) ;
#83098 = CARTESIAN_POINT ( 'NONE',  ( 36.57684789031566197, -279.8407252482076046, -274.1057501538825818 ) ) ;
#83100 = CARTESIAN_POINT ( 'NONE',  ( -96.07850890135850364, -283.2641342540224514, -224.6096781897254573 ) ) ;
#83099 = CARTESIAN_POINT ( 'NONE',  ( 34.21890914036310249, -280.3521316485039279, -287.5743394025379303 ) ) ;
#83102 = CARTESIAN_POINT ( 'NONE',  ( -54.48590238382975315, -291.2724506337452226, -343.4280832037434266 ) ) ;
#83101 = VECTOR ( 'NONE', #39806, 1000.000000000000000 ) ;
#83103 = CARTESIAN_POINT ( 'NONE',  ( -71.13808908855099844, -280.8007881666577532, -205.1937899692240137 ) ) ;
#83104 = CARTESIAN_POINT ( 'NONE',  ( 0.000000000000000000, 0.000000000000000000, 10.00000000000000000 ) ) ;
#83105 = CARTESIAN_POINT ( 'NONE',  ( 28.60453745795705416, -279.4503587958092226, -232.1834522322942576 ) ) ;
#83106 = CARTESIAN_POINT ( 'NONE',  ( -9.283698933093397443, -294.4191020254279465, -200.8071876931842326 ) ) ;
#83107 = CARTESIAN_POINT ( 'NONE',  ( -35.33995882435181102, -278.3167865270415859, -194.3878551397247065 ) ) ;
#83108 = VECTOR ( 'NONE', #4412, 1000.000000000000000 ) ;
#83109 = CARTESIAN_POINT ( 'NONE',  ( -7.458403146126411976, -277.3010543065921638, -337.0760430741235041 ) ) ;
#83110 = CARTESIAN_POINT ( 'NONE',  ( -16.62214569753492910, -284.7853767098214348, -342.6697022834584345 ) ) ;
#83111 = FACE_OUTER_BOUND ( 'NONE', #55050, .T. ) ;
#83112 = CARTESIAN_POINT ( 'NONE',  ( -77.35275394717345421, -291.5040294900244362, -334.5191752487101553 ) ) ;
#83113 = CARTESIAN_POINT ( 'NONE',  ( 22.87174090187753706, -286.1090246389712206, -222.6065031546506816 ) ) ;
#83114 = CARTESIAN_POINT ( 'NONE',  ( -52.51455800951686825, -290.2545689538642932, -198.0852149254908454 ) ) ;
#83115 = CARTESIAN_POINT ( 'NONE',  ( -43.47198418667934305, -255.6354909541967970, -443.8759249308465655 ) ) ;
#83116 = CARTESIAN_POINT ( 'NONE',  ( 36.19198120010537423, -274.2533343577543405, -271.6099473374693503 ) ) ;
#83117 = CARTESIAN_POINT ( 'NONE',  ( 30.61137758267051723, -292.0871399327428435, -300.2483177050472136 ) ) ;
#83118 = DIRECTION ( 'NONE',  ( -1.000000000000000000, -0.000000000000000000, -0.000000000000000000 ) ) ;
#83119 = DIRECTION ( 'NONE',  ( 0.000000000000000000, 0.000000000000000000, 1.000000000000000000 ) ) ;
#83120 = CARTESIAN_POINT ( 'NONE',  ( -102.6126562036653525, -289.5537977832203183, -230.7319518079767988 ) ) ;
#83121 = CARTESIAN_POINT ( 'NONE',  ( -40.02317025167526765, -287.6180297807639477, -196.6098458938413955 ) ) ;
#83122 = CARTESIAN_POINT ( 'NONE',  ( -51.51851457042311466, -287.4709339847963747, -345.0135924471754834 ) ) ;
#83123 = CARTESIAN_POINT ( 'NONE',  ( -17.02649037111903141, -287.7447841529243533, -199.5783122343772504 ) ) ;
#83124 = CARTESIAN_POINT ( 'NONE',  ( 222.4306832106270804, -141.7221692137691775, 21.50000000000000000 ) ) ;
#83125 = CARTESIAN_POINT ( 'NONE',  ( 7.016729896633526309, -287.4763416801692983, -212.1169524188645994 ) ) ;
#83126 = CARTESIAN_POINT ( 'NONE',  ( 23.47182552106948350, -294.9283187751506148, -225.8625572963901789 ) ) ;
#83127 = CARTESIAN_POINT ( 'NONE',  ( -17.75518393683089613, -274.8813058344071578, -343.3383923823524242 ) ) ;
#83128 = CARTESIAN_POINT ( 'NONE',  ( -75.32207260113149516, -277.8775116613626324, -337.3180862408706275 ) ) ;
#83129 = CARTESIAN_POINT ( 'NONE',  ( -61.21007982153145122, -289.8246126396358022, -198.6149119826060030 ) ) ;
#83130 = CARTESIAN_POINT ( 'NONE',  ( -68.67252482324978757, -279.6516401569736558, -200.0091219581084374 ) ) ;
#83131 = CARTESIAN_POINT ( 'NONE',  ( -76.08545204440164866, -299.5120923517177403, -206.4986058663844801 ) ) ;
#83132 = CARTESIAN_POINT ( 'NONE',  ( -43.35434167168779851, -267.5826604045195154, -504.1128848280075090 ) ) ;
#83133 = CARTESIAN_POINT ( 'NONE',  ( -112.3076814564642376, -282.5809905178211920, -268.1022932347049732 ) ) ;
#83134 = CARTESIAN_POINT ( 'NONE',  ( -48.18343439339133738, -255.2824783920493132, -484.1824042360379394 ) ) ;
#83135 = CARTESIAN_POINT ( 'NONE',  ( -91.89133863413029246, -275.9799916348003990, -320.7867117569232960 ) ) ;
#83136 = CARTESIAN_POINT ( 'NONE',  ( 36.45301858854293187, -279.7248558642858143, -283.8241143756725364 ) ) ;
#83137 = FACE_OUTER_BOUND ( 'NONE', #39452, .T. ) ;
#83138 = CARTESIAN_POINT ( 'NONE',  ( 22.95814458870818342, -274.6623591738508026, -317.1437880219412477 ) ) ;
#83139 = CARTESIAN_POINT ( 'NONE',  ( -66.30800298652690117, -296.9585538622890795, -338.1229143897916742 ) ) ;
#83140 = CARTESIAN_POINT ( 'NONE',  ( 28.03427491092630675, -280.9995990395029821, -310.5550497094070579 ) ) ;
#83141 = CARTESIAN_POINT ( 'NONE',  ( -110.6099278948500881, -297.5147316574928027, -268.7396085574501967 ) ) ;
#83142 = CARTESIAN_POINT ( 'NONE',  ( -108.4365821937787047, -298.2297614479181789, -241.9553379311838910 ) ) ;
#83143 = CARTESIAN_POINT ( 'NONE',  ( 13.51442350090612265, -274.4552300858728131, -217.9612880576198108 ) ) ;
#83144 = CARTESIAN_POINT ( 'NONE',  ( 22.12412568436829119, -296.1785539594726515, -316.0857227883710721 ) ) ;
#83145 = CARTESIAN_POINT ( 'NONE',  ( 0.2819371970451695630, -286.7055900410825302, -203.1637669365159411 ) ) ;
#83146 = CARTESIAN_POINT ( 'NONE',  ( -7.090014464466213973, -274.7990905942303925, -339.8383779355673937 ) ) ;
#83147 = CARTESIAN_POINT ( 'NONE',  ( -43.18441260890356403, -288.9573296845708796, -347.1391273040750889 ) ) ;
#83148 = CARTESIAN_POINT ( 'NONE',  ( 33.92730608622555621, -286.8325603911933968, -287.2174877620875577 ) ) ;
#83149 = CARTESIAN_POINT ( 'NONE',  ( -110.9568600721551661, -288.7370523765573012, -255.9482898287885746 ) ) ;
#83150 = ORIENTED_EDGE ( 'NONE', *, *, #80612, .F. ) ;
#83151 = CARTESIAN_POINT ( 'NONE',  ( 180.5468918863934960, 256.3577768311903355, -167.2605672291198857 ) ) ;
#83152 = CARTESIAN_POINT ( 'NONE',  ( -74.75279405581906644, -289.0723286309776654, -333.1324787612658156 ) ) ;
#83153 = CYLINDRICAL_SURFACE ( 'NONE', #24828, 155.4364916446740210 ) ;
#83154 = CARTESIAN_POINT ( 'NONE',  ( -105.5695066678691774, -285.0372381067398919, -305.6592552194999257 ) ) ;
#83155 = CARTESIAN_POINT ( 'NONE',  ( 26.30455555904806531, -292.0426190136563491, -227.3493617645108600 ) ) ;
#83156 = CARTESIAN_POINT ( 'NONE',  ( 5.715257828289471931, -282.2251864295674295, -207.4918982849529527 ) ) ;
#83157 = CARTESIAN_POINT ( 'NONE',  ( -33.95397479660803697, -281.4091037548707845, -193.9293079117428817 ) ) ;
#83158 = APPLICATION_CONTEXT ( 'automotive_design' ) ;
#83159 = CARTESIAN_POINT ( 'NONE',  ( -36.19566085279808476, -282.8707060976041134, -343.3521215276085172 ) ) ;
#83160 = CARTESIAN_POINT ( 'NONE',  ( -9.215319398998989442, -278.6846286859714041, -339.9013645283562823 ) ) ;
#83161 = CARTESIAN_POINT ( 'NONE',  ( -75.77990528800914660, -297.5541807025517187, -203.5803301442099382 ) ) ;
#83162 = CARTESIAN_POINT ( 'NONE',  ( -2.695874784059958618, -275.8356015078776409, -205.5466885305193898 ) ) ;
#83163 = CARTESIAN_POINT ( 'NONE',  ( -33.39685296893049582, -290.1221380521362221, -195.8078522684061227 ) ) ;
#83164 = UNCERTAINTY_MEASURE_WITH_UNIT (LENGTH_MEASURE( 1.000000000000000082E-05 ), #18050, 'distance_accuracy_value', 'NONE');
#83165 = CARTESIAN_POINT ( 'NONE',  ( -40.51765895786904537, -296.9316393825748150, -197.1082309030722968 ) ) ;
#83166 = VERTEX_POINT ( 'NONE', #41581 ) ;
#83167 = DIRECTION ( 'NONE',  ( -0.000000000000000000, 1.000000000000000000, 0.000000000000000000 ) ) ;
#83168 = CARTESIAN_POINT ( 'NONE',  ( -97.75757782972854670, -287.0688954467431131, -226.8510209296899234 ) ) ;
#83169 = CARTESIAN_POINT ( 'NONE',  ( -34.85085611945666528, -296.1012129746785035, -347.0115465967681985 ) ) ;
#83170 = CARTESIAN_POINT ( 'NONE',  ( -99.70059961858143538, -285.7296285267968869, -232.1167816535811141 ) ) ;
#83171 = ADVANCED_FACE ( 'NONE', ( #86531 ), #21698, .T. ) ;
#83172 = CARTESIAN_POINT ( 'NONE',  ( -54.09162016184902200, -276.3207675419643010, -345.3306141815919545 ) ) ;
#83173 = CARTESIAN_POINT ( 'NONE',  ( -74.63673230796331381, -292.2206297008740421, -203.1123755302712368 ) ) ;
#83174 = CARTESIAN_POINT ( 'NONE',  ( -54.65890307532110626, -283.9714749688913571, -196.6019154390307619 ) ) ;
#83175 = CIRCLE ( 'NONE', #66575, 8.550761578869359170 ) ;
#83176 = CARTESIAN_POINT ( 'NONE',  ( 21.29158347836460052, -293.2125577443698035, -220.4623054196183034 ) ) ;
#83177 = CARTESIAN_POINT ( 'NONE',  ( -92.42488083952731870, -290.2014559514655048, -318.3734115160648912 ) ) ;
#83178 = CARTESIAN_POINT ( 'NONE',  ( 185.0717070212824922, 2.982529536179759688, 9.000000000000001776 ) ) ;
#83179 = DIRECTION ( 'NONE',  ( -0.000000000000000000, -0.9681751575201845705, 0.2502735790305594676 ) ) ;
#83180 = CARTESIAN_POINT ( 'NONE',  ( -69.70536949854505337, -196.1875009344347802, -356.7257175233714861 ) ) ;
#83181 = TOROIDAL_SURFACE ( 'NONE', #16622, 24.50000000000000355, 0.5000000000000000000 ) ;
#83182 = CARTESIAN_POINT ( 'NONE',  ( -112.8047494735694158, -286.2194742402294310, -258.6968085365660954 ) ) ;
#83183 = CARTESIAN_POINT ( 'NONE',  ( -114.2704648735229114, -294.0523547857347353, -270.3284710469133074 ) ) ;
#83184 = EDGE_LOOP ( 'NONE', ( #64420, #33830, #20045, #59073 ) ) ;
#83185 = CARTESIAN_POINT ( 'NONE',  ( 18.20771260330259977, -279.7938751577332823, -222.5036913694277700 ) ) ;
#83186 = CARTESIAN_POINT ( 'NONE',  ( 8.225130196732044041, -276.1147838858450427, -332.4707111938078015 ) ) ;
#83187 = CARTESIAN_POINT ( 'NONE',  ( -19.11200047120404122, -282.2873267007680624, -197.7285527077597180 ) ) ;
#83188 = CARTESIAN_POINT ( 'NONE',  ( -97.05825111094482338, -248.4111539963268740, -332.8678862503371079 ) ) ;
#83189 = CARTESIAN_POINT ( 'NONE',  ( -90.04496921573739598, -282.3537317053323932, -325.7597341201185372 ) ) ;
#83190 = CARTESIAN_POINT ( 'NONE',  ( -75.54064640864875457, -283.5599502960607197, -206.2308809204665181 ) ) ;
#83191 = CARTESIAN_POINT ( 'NONE',  ( -113.1065001290297545, -274.4122686959622115, -270.3847523717674335 ) ) ;
#83192 = CARTESIAN_POINT ( 'NONE',  ( -107.6603347381303024, -296.7825687261477583, -290.1923576904333686 ) ) ;
#83193 = ORIENTED_EDGE ( 'NONE', *, *, #43122, .F. ) ;
#83194 = CARTESIAN_POINT ( 'NONE',  ( -12.07503723466268397, -291.0726482404612057, -201.2935448514444943 ) ) ;
#83195 = CARTESIAN_POINT ( 'NONE',  ( 20.74870263431859740, -276.8855229691156410, -320.7677336948189009 ) ) ;
#83196 = CARTESIAN_POINT ( 'NONE',  ( 18.99885335402941422, -274.8942946963477425, -223.9419190091889504 ) ) ;
#83197 = CARTESIAN_POINT ( 'NONE',  ( 32.27824904882037771, -274.0578960981491150, -238.0701051869069431 ) ) ;
#83198 = CARTESIAN_POINT ( 'NONE',  ( 222.4306832106270804, -142.7221692137691775, -32.50000000000000711 ) ) ;
#83199 = CARTESIAN_POINT ( 'NONE',  ( -19.80690828132705050, -272.2772748964343350, -197.3868958706597141 ) ) ;
#83200 = ADVANCED_FACE ( 'NONE', ( #6092 ), #62559, .T. ) ;
#83201 = CARTESIAN_POINT ( 'NONE',  ( 27.61467143157695148, -295.5088486365418134, -310.7007898283400777 ) ) ;
#83202 = CARTESIAN_POINT ( 'NONE',  ( 152.8344704311132602, 129.4968913933752503, 12.52864452723162003 ) ) ;
#83203 = CARTESIAN_POINT ( 'NONE',  ( 199.2296996224750103, 66.10105075020101140, 0.000000000000000000 ) ) ;
#83204 = CARTESIAN_POINT ( 'NONE',  ( -7.113509023457820213, -283.7256787409455683, -337.1617350806279205 ) ) ;
#83205 = CARTESIAN_POINT ( 'NONE',  ( 32.23597609400210473, -282.9175547939278772, -239.8173627624601636 ) ) ;
#83206 = CARTESIAN_POINT ( 'NONE',  ( -95.03239482664280047, -284.5326697714195916, -225.4445098187927385 ) ) ;
#83207 = CARTESIAN_POINT ( 'NONE',  ( -10.98718220638100362, -275.1026202818105730, -339.2949978994091111 ) ) ;
#83208 = CARTESIAN_POINT ( 'NONE',  ( -10.50753251409707012, -284.5588702689336174, -339.6311675518573452 ) ) ;
#83209 = CARTESIAN_POINT ( 'NONE',  ( -94.15278944238026781, -276.3727118290278781, -317.3192374782005345 ) ) ;
#83210 = CARTESIAN_POINT ( 'NONE',  ( 9.672831515439035854, -275.7963067823124561, -214.0464532056879534 ) ) ;
#83211 = CARTESIAN_POINT ( 'NONE',  ( 193.6552470326849402, 250.5000000000000568, 16.89672165344822119 ) ) ;
#83212 = CARTESIAN_POINT ( 'NONE',  ( -77.41704251632816636, -280.3322169371054997, -204.7394245984010865 ) ) ;
#83213 = VERTEX_POINT ( 'NONE', #7032 ) ;
#83214 = EDGE_LOOP ( 'NONE', ( #93205, #9126 ) ) ;
#83215 = EDGE_CURVE ( 'NONE', #30930, #34997, #68628, .T. ) ;
#83216 = CARTESIAN_POINT ( 'NONE',  ( 197.1285099842257011, 19.08195175178710556, 12.05325424581539906 ) ) ;
#83217 = CARTESIAN_POINT ( 'NONE',  ( -105.5771099020245316, -286.8419108962791029, -237.4334042637140669 ) ) ;
#83218 = CARTESIAN_POINT ( 'NONE',  ( -41.05762463071861390, -294.2972409424061766, -343.4407619019840467 ) ) ;
#83219 = CARTESIAN_POINT ( 'NONE',  ( -87.32448557239666798, -289.0761422646986603, -328.8693568803246876 ) ) ;
#83220 = CARTESIAN_POINT ( 'NONE',  ( 32.34607846310996848, -286.1194317034921824, -295.2927751172559283 ) ) ;
#83222 = CARTESIAN_POINT ( 'NONE',  ( -110.7979327074476998, -288.6740734437386209, -279.4251076248659729 ) ) ;
#83221 = CARTESIAN_POINT ( 'NONE',  ( -39.97698862683193255, -284.5931181933934795, -196.8190880071194329 ) ) ;
#83223 = CARTESIAN_POINT ( 'NONE',  ( -107.7401714905424228, -286.0325956486889822, -249.4197057840079026 ) ) ;
#83224 = CARTESIAN_POINT ( 'NONE',  ( -15.20496157192699904, -274.7654898958717808, -342.0741607336552192 ) ) ;
#83225 = CARTESIAN_POINT ( 'NONE',  ( 34.11121775428021152, -285.6138032643681868, -243.8862064574834676 ) ) ;
#83226 = CARTESIAN_POINT ( 'NONE',  ( -104.7278169973263573, -298.9863765777511162, -237.4352634164672509 ) ) ;
#83227 = CARTESIAN_POINT ( 'NONE',  ( 35.36446571222547419, -285.7965889165869839, -289.4357576458212407 ) ) ;
#83228 = CARTESIAN_POINT ( 'NONE',  ( 32.19624995882173835, -282.1874816862875832, -247.2256841327707093 ) ) ;
#83229 = CARTESIAN_POINT ( 'NONE',  ( -97.54510290562218700, -291.9386487239567600, -315.3888236536990348 ) ) ;
#83230 = CARTESIAN_POINT ( 'NONE',  ( 123.4306832106270946, -134.2391364535880882, -5.024999999999987921 ) ) ;
#83231 = LINE ( 'NONE', #76147, #80600 ) ;
#83232 = CARTESIAN_POINT ( 'NONE',  ( -105.8502771178793296, -298.0565854005219535, -302.2341328069030055 ) ) ;
#83233 = CARTESIAN_POINT ( 'NONE',  ( -86.78404811331400026, -277.3642737483932592, -213.9655962481994322 ) ) ;
#83234 = CARTESIAN_POINT ( 'NONE',  ( -58.88359884752441076, -290.9775192637200121, -196.6040476799545900 ) ) ;
#83235 = CARTESIAN_POINT ( 'NONE',  ( -108.7487592832080168, -294.7079926242935244, -289.0517460242874677 ) ) ;
#83236 = CARTESIAN_POINT ( 'NONE',  ( 19.72443105625738013, -280.8880721409860257, -316.6918569046043785 ) ) ;
#83237 = CARTESIAN_POINT ( 'NONE',  ( -2.212929956298244960, -272.6007963000595282, -204.7312184997753661 ) ) ;
#83238 = CARTESIAN_POINT ( 'NONE',  ( 20.92435662976772548, -295.4936783009602550, -315.1735815786920512 ) ) ;
#83239 = CARTESIAN_POINT ( 'NONE',  ( -54.49178911615188525, -300.3376638359845288, -195.3683826091709363 ) ) ;
#83240 = CARTESIAN_POINT ( 'NONE',  ( 52.59015588275923392, -297.6385992399109455, -194.0771794660524279 ) ) ;
#83241 = CARTESIAN_POINT ( 'NONE',  ( -27.89631698261259629, -293.1737967659688024, -345.8110473453802456 ) ) ;
#83242 = CARTESIAN_POINT ( 'NONE',  ( 2.544748863795425198, -294.0233065930323164, -208.4586566532220218 ) ) ;
#83243 = DIRECTION ( 'NONE',  ( 0.7957555401921962979, 0.6056179655966504871, 0.000000000000000000 ) ) ;
#83244 = CARTESIAN_POINT ( 'NONE',  ( 33.46190228742342043, -294.1122826943876021, -251.9369053158165741 ) ) ;
#83245 = AXIS2_PLACEMENT_3D ( 'NONE', #89210, #31940, #60829 ) ;
#83246 = DIRECTION ( 'NONE',  ( 0.000000000000000000, 0.000000000000000000, 1.000000000000000000 ) ) ;
#83248 = CARTESIAN_POINT ( 'NONE',  ( -75.65805633681154063, -295.5786477249818631, -332.5558444531047826 ) ) ;
#83247 = CARTESIAN_POINT ( 'NONE',  ( -87.25143057011788983, -281.7633821609863389, -326.8881012458639930 ) ) ;
#83249 = CARTESIAN_POINT ( 'NONE',  ( 38.14554913369389766, -281.7420990074488145, -285.5491132054527270 ) ) ;
#83250 = CONICAL_SURFACE ( 'NONE', #25799, 4.999999999999990230, 1.029744258676648538 ) ;
#83251 = CARTESIAN_POINT ( 'NONE',  ( -58.48501760427461704, -282.9848260694627697, -344.4348728664098758 ) ) ;
#83252 = CARTESIAN_POINT ( 'NONE',  ( -99.65095508441373795, -287.9905435756493830, -311.8282169226496308 ) ) ;
#83253 = CARTESIAN_POINT ( 'NONE',  ( 169.2744399300530347, 8.542400036368780647, 13.00000000000000178 ) ) ;
#83254 = CARTESIAN_POINT ( 'NONE',  ( 4.152293452008417596, -280.9841419206805995, -334.4622683585670302 ) ) ;
#83255 = CARTESIAN_POINT ( 'NONE',  ( -20.57742128474241738, -287.7622242428591903, -345.2517276494198768 ) ) ;
#83256 = CARTESIAN_POINT ( 'NONE',  ( 179.1465552314772083, 8.542400036368780647, 25.74970488511327815 ) ) ;
#83257 = CARTESIAN_POINT ( 'NONE',  ( -71.28076103321581058, -297.1081090744941662, -335.9083033716763111 ) ) ;
#83258 = CARTESIAN_POINT ( 'NONE',  ( 30.03216182896389341, -277.4481546943553667, -306.5196481849504266 ) ) ;
#83259 = CARTESIAN_POINT ( 'NONE',  ( -106.4633666503563347, -278.5335082491939147, -246.6626598034360143 ) ) ;
#83260 = CARTESIAN_POINT ( 'NONE',  ( 37.42143541267572715, -293.4883400369601532, -251.9363094721450125 ) ) ;
#83261 = CARTESIAN_POINT ( 'NONE',  ( -24.79718615571157514, -280.9733054289794723, -344.9256234413394964 ) ) ;
#83262 = CARTESIAN_POINT ( 'NONE',  ( -4.717527877856648288, -291.5514842592104969, -204.7798398768614163 ) ) ;
#83263 = CARTESIAN_POINT ( 'NONE',  ( -110.6402949683239285, -294.7566692966816504, -254.4167933054898185 ) ) ;
#83264 = ORIENTED_EDGE ( 'NONE', *, *, #68323, .F. ) ;
#83265 = DIRECTION ( 'NONE',  ( 0.000000000000000000, 0.000000000000000000, 1.000000000000000000 ) ) ;
#83266 = CARTESIAN_POINT ( 'NONE',  ( -7.969317369887636282, -294.1643260986725181, -337.2720272974965496 ) ) ;
#83267 = CARTESIAN_POINT ( 'NONE',  ( 153.6539576904058038, 130.0000000000000568, -12.50000000000000000 ) ) ;
#83268 = CARTESIAN_POINT ( 'NONE',  ( -102.0172624299487154, -294.4809262143061801, -239.1787733560258289 ) ) ;
#83269 = CARTESIAN_POINT ( 'NONE',  ( -114.1798439490726054, -271.7853104079259765, -267.4894666277526198 ) ) ;
#83270 = CARTESIAN_POINT ( 'NONE',  ( 37.57702599966744827, -279.5438913507804841, -258.7290094800859492 ) ) ;
#83271 = CARTESIAN_POINT ( 'NONE',  ( -36.58722580065883534, -287.3766033886709010, -193.8450319251169276 ) ) ;
#83272 = CARTESIAN_POINT ( 'NONE',  ( -29.17522936735944938, -288.7790977884083077, -342.9028904988959425 ) ) ;
#83273 = CARTESIAN_POINT ( 'NONE',  ( -106.9124004078946939, -279.7502123630232518, -294.8185464424838074 ) ) ;
#83274 = CARTESIAN_POINT ( 'NONE',  ( -110.9886143634434887, -274.2238866686519714, -264.8740468337414882 ) ) ;
#83275 = CARTESIAN_POINT ( 'NONE',  ( -108.3528706729627515, -277.5914034571713387, -251.7498901552513928 ) ) ;
#83276 = ORIENTED_EDGE ( 'NONE', *, *, #89855, .T. ) ;
#83277 = CARTESIAN_POINT ( 'NONE',  ( -114.3417001280813849, -272.3854989540131442, -270.3590004217965088 ) ) ;
#83278 = CARTESIAN_POINT ( 'NONE',  ( -107.3793003533697146, -292.1429072489794976, -295.5811249467953985 ) ) ;
#83279 = CARTESIAN_POINT ( 'NONE',  ( 35.60979886873431610, -295.4335015497329664, -292.5518220834818521 ) ) ;
#83280 = CARTESIAN_POINT ( 'NONE',  ( 195.2616234104794728, 71.31492948064700954, -13.29451844366211510 ) ) ;
#83281 = CARTESIAN_POINT ( 'NONE',  ( -73.58830703904730797, -290.1982105326773080, -333.8584295832638418 ) ) ;
#83282 = DIRECTION ( 'NONE',  ( -1.000000000000000000, 0.000000000000000000, 0.000000000000000000 ) ) ;
#83283 = ADVANCED_FACE ( 'NONE', ( #79470 ), #84481, .F. ) ;
#83284 = CARTESIAN_POINT ( 'NONE',  ( 27.01586018128563538, -291.1591126990565499, -230.2818182179555322 ) ) ;
#83285 = CARTESIAN_POINT ( 'NONE',  ( -29.06671523562641468, -298.4863826236468185, -193.3818080976452904 ) ) ;
#83286 = CARTESIAN_POINT ( 'NONE',  ( 199.0061125298537377, 275.0000000000000568, -7.725424859374024678 ) ) ;
#83287 = CARTESIAN_POINT ( 'NONE',  ( 195.8614702967192329, 25.38294244956506773, 14.12010220544310535 ) ) ;
#83288 = CARTESIAN_POINT ( 'NONE',  ( -109.2059864757586212, -291.7437069328147459, -296.1736896283744613 ) ) ;
#83289 = CARTESIAN_POINT ( 'NONE',  ( 44.71564893372296723, -296.0519495502701943, -270.3284710469131937 ) ) ;
#83290 = CARTESIAN_POINT ( 'NONE',  ( -57.92244669427246606, -287.7860059568863562, -198.3595484264738502 ) ) ;
#83291 = CARTESIAN_POINT ( 'NONE',  ( -67.78046913888434233, -271.6516253564632279, -201.9840105527592868 ) ) ;
#83292 = CARTESIAN_POINT ( 'NONE',  ( -101.9800678583620339, -274.9696152174484496, -233.3359258882194638 ) ) ;
#83293 = CARTESIAN_POINT ( 'NONE',  ( 22.98579280248460321, -291.0334856379262760, -226.7285651111565414 ) ) ;
#83294 = CARTESIAN_POINT ( 'NONE',  ( -72.25014979657481717, -279.3693141221907013, -337.6192128514094861 ) ) ;
#83295 = ORIENTED_EDGE ( 'NONE', *, *, #59476, .T. ) ;
#83296 = CARTESIAN_POINT ( 'NONE',  ( 28.23885174087255123, -281.3391539641907002, -302.7727779485226733 ) ) ;
#83297 = CARTESIAN_POINT ( 'NONE',  ( 37.60653784183389803, -276.8367109855100239, -286.6784192960640212 ) ) ;
#83298 = CARTESIAN_POINT ( 'NONE',  ( 18.87922307554504187, -279.6346889309546100, -218.3301991669989945 ) ) ;
#83299 = CARTESIAN_POINT ( 'NONE',  ( 200.9738707121548487, 293.6302286493877318, -68.30388873731220656 ) ) ;
#83300 = CARTESIAN_POINT ( 'NONE',  ( 22.56717584958217770, -275.8482591014254695, -222.3429151664357448 ) ) ;
#83301 = ADVANCED_FACE ( 'NONE', ( #856 ), #8405, .T. ) ;
#83302 = CONTEXT_DEPENDENT_SHAPE_REPRESENTATION ( #5759, #86768 ) ;
#83303 = CARTESIAN_POINT ( 'NONE',  ( -35.55956057785753899, -275.5942169536958204, -194.0622504129907497 ) ) ;
#83304 = CARTESIAN_POINT ( 'NONE',  ( -105.5937364680635966, -281.2662352645559167, -254.8156830097664738 ) ) ;
#83305 = ORIENTED_EDGE ( 'NONE', *, *, #49429, .F. ) ;
#83306 = DIRECTION ( 'NONE',  ( 0.000000000000000000, 0.000000000000000000, -1.000000000000000000 ) ) ;
#83307 = VECTOR ( 'NONE', #48462, 1000.000000000000000 ) ;
#83308 = CARTESIAN_POINT ( 'NONE',  ( -68.87854996587870460, -290.5565500625998538, -336.5400661233987307 ) ) ;
#83309 = CARTESIAN_POINT ( 'NONE',  ( 11.41004590248148531, -288.4771033813177041, -212.0066164215762967 ) ) ;
#83310 = CARTESIAN_POINT ( 'NONE',  ( -75.92957757043760125, -288.9310697877745611, -332.4487043634551355 ) ) ;
#83311 = CARTESIAN_POINT ( 'NONE',  ( 22.94758027405440615, -286.4194597403190983, -222.5412719806427901 ) ) ;
#83312 = DIRECTION ( 'NONE',  ( -0.000000000000000000, 1.000000000000000000, -0.000000000000000000 ) ) ;
#83313 = CARTESIAN_POINT ( 'NONE',  ( -5.708323508255333856, -281.0290212011087192, -337.0516244364250724 ) ) ;
#83314 = CARTESIAN_POINT ( 'NONE',  ( -23.53255292911645924, -290.7343436940137167, -343.3532103296899436 ) ) ;
#83315 = CARTESIAN_POINT ( 'NONE',  ( 8.207455521533429277, -280.8963281503307599, -328.3571158065620921 ) ) ;
#83316 = CARTESIAN_POINT ( 'NONE',  ( -108.4539811086181373, -280.1112457013910557, -251.7566695546871642 ) ) ;
#83317 = CARTESIAN_POINT ( 'NONE',  ( -29.70075918095427170, -277.4452896280946561, -343.0729538277769279 ) ) ;
#83318 = CARTESIAN_POINT ( 'NONE',  ( -113.7905917931544195, -289.4081175454489312, -265.5056385191937807 ) ) ;
#83319 = CARTESIAN_POINT ( 'NONE',  ( -52.15219579729848220, -286.6701553414141586, -194.9091745017959170 ) ) ;
#83320 = CARTESIAN_POINT ( 'NONE',  ( 23.80870509021086789, -287.4212274303690720, -223.6473909717856827 ) ) ;
#83321 = CARTESIAN_POINT ( 'NONE',  ( -110.0955936040637795, -284.6398252064130929, -276.3503573813566732 ) ) ;
#83322 = VERTEX_POINT ( 'NONE', #72809 ) ;
#83323 = DIRECTION ( 'NONE',  ( 0.000000000000000000, 0.000000000000000000, -1.000000000000000000 ) ) ;
#83324 = CARTESIAN_POINT ( 'NONE',  ( -98.02535698662634900, -291.7989267795626347, -315.7455363306515324 ) ) ;
#83325 = CARTESIAN_POINT ( 'NONE',  ( -6.015041406537023683, -293.3337742651395388, -340.1603925314517483 ) ) ;
#83326 = CARTESIAN_POINT ( 'NONE',  ( 21.67789180088654177, -274.0053569293037299, -227.0010416776049169 ) ) ;
#83327 = CARTESIAN_POINT ( 'NONE',  ( -111.8719108426423929, -295.6628836716047317, -289.3499932580477321 ) ) ;
#83328 = CARTESIAN_POINT ( 'NONE',  ( -52.49359440065099136, -290.3345624990209899, -198.1898818989702988 ) ) ;
#83329 = CARTESIAN_POINT ( 'NONE',  ( 4.369234031972163201, -292.7208328059975884, -331.5017099258112694 ) ) ;
#83330 = CARTESIAN_POINT ( 'NONE',  ( -108.7330864522271128, -291.5336243651678387, -287.4022583451558148 ) ) ;
#83331 = CARTESIAN_POINT ( 'NONE',  ( -55.80257052418232888, -229.5268262511776527, -22.50000000000000000 ) ) ;
#83332 = CARTESIAN_POINT ( 'NONE',  ( 36.27177948952483177, -291.3564332626361306, -255.0964826588745780 ) ) ;
#83333 = CARTESIAN_POINT ( 'NONE',  ( 19.31339685859821742, -296.2347575297886806, -319.5823197403796030 ) ) ;
#83334 = CARTESIAN_POINT ( 'NONE',  ( 32.89222662944607833, -288.2191763907642326, -249.5659052442754842 ) ) ;
#83335 = CARTESIAN_POINT ( 'NONE',  ( 36.02755172885924395, -277.3117607985875566, -253.1190377707951313 ) ) ;
#83336 = CARTESIAN_POINT ( 'NONE',  ( -17.47573911354671594, -275.5962690678069862, -344.3432260255914343 ) ) ;
#83337 = CARTESIAN_POINT ( 'NONE',  ( -113.7604456051334409, -272.0080941347234216, -261.7885964075962306 ) ) ;
#83338 = CARTESIAN_POINT ( 'NONE',  ( 35.15263811323885079, -273.9861073113754628, -285.2790581522954199 ) ) ;
#83339 = CARTESIAN_POINT ( 'NONE',  ( -13.83134329412208174, -278.4393196359653189, -199.6767566697508300 ) ) ;
#83340 = CARTESIAN_POINT ( 'NONE',  ( 35.10159219554091692, -276.9160080622418150, -282.4626632348733324 ) ) ;
#83341 = CARTESIAN_POINT ( 'NONE',  ( -84.38862496545182523, -276.0868920106904625, -330.3700439172448000 ) ) ;
#83342 = CARTESIAN_POINT ( 'NONE',  ( 201.2509219214787777, 65.09645894983574976, 2.633798379907748455 ) ) ;
#83343 = CARTESIAN_POINT ( 'NONE',  ( -90.27613212494456718, -273.9297675972762818, -219.9261520788251119 ) ) ;
#83344 = CARTESIAN_POINT ( 'NONE',  ( -113.5000000000000568, -298.0521521680024080, -397.9547385950631337 ) ) ;
#83346 = CARTESIAN_POINT ( 'NONE',  ( 19.85682786961195845, -274.7450286067314096, -224.9833335238277812 ) ) ;
#83345 = CARTESIAN_POINT ( 'NONE',  ( -38.91173403247118756, -287.0918713555852264, -345.6999645357195732 ) ) ;
#83347 = CARTESIAN_POINT ( 'NONE',  ( 31.68742154508574771, -287.9919321177838469, -304.5985248271242085 ) ) ;
#83348 = CARTESIAN_POINT ( 'NONE',  ( -89.48027949774179035, -289.4299499131792572, -326.9942605120532448 ) ) ;
#83349 = CARTESIAN_POINT ( 'NONE',  ( -95.53336798483998393, -275.2068316506991437, -222.7620568408226518 ) ) ;
#83350 = CARTESIAN_POINT ( 'NONE',  ( -109.3742783101513538, -294.2904637175404332, -290.6425407325457968 ) ) ;
#83351 = CARTESIAN_POINT ( 'NONE',  ( 37.70560280667164932, -280.9568022370764311, -286.9161211083728062 ) ) ;
#83352 = DIRECTION ( 'NONE',  ( -0.000000000000000000, -1.000000000000000000, -0.000000000000000000 ) ) ;
#83353 = CARTESIAN_POINT ( 'NONE',  ( -34.74687298594315621, -278.0844949551296281, -195.3558671629433263 ) ) ;
#83354 = DIRECTION ( 'NONE',  ( 1.110223024625155531E-13, 0.000000000000000000, 1.000000000000000000 ) ) ;
#83355 = CARTESIAN_POINT ( 'NONE',  ( -110.0182797356726212, -289.2112867694162333, -280.7103298263742204 ) ) ;
#83356 = DIRECTION ( 'NONE',  ( -1.000000000000000000, 0.000000000000000000, 0.000000000000000000 ) ) ;
#83357 = CARTESIAN_POINT ( 'NONE',  ( -64.78022087047456523, -289.6937010153351366, -200.5465843163862871 ) ) ;
#83358 = CARTESIAN_POINT ( 'NONE',  ( -11.26280442437097129, -275.9182305945000735, -201.3819758647652520 ) ) ;
#83359 = CARTESIAN_POINT ( 'NONE',  ( 38.82291841351219119, -282.9001875325752167, -264.2327271565270053 ) ) ;
#83361 = CARTESIAN_POINT ( 'NONE',  ( -97.53234923149224755, -283.9761248469291672, -311.7540092301907180 ) ) ;
#83360 = CARTESIAN_POINT ( 'NONE',  ( -96.66698164563842965, -271.2698571632007543, -223.5655500793722581 ) ) ;
#83362 = CARTESIAN_POINT ( 'NONE',  ( 11.92766407886652047, -276.1778221786436234, -215.6307909317528697 ) ) ;
#83363 = CARTESIAN_POINT ( 'NONE',  ( 25.40907944586396638, -275.8375387543028978, -232.6473063329487445 ) ) ;
#83364 = CARTESIAN_POINT ( 'NONE',  ( -12.71657381548230248, -286.8144823243158612, -341.8506441788350116 ) ) ;
#83365 = ADVANCED_FACE ( 'NONE', ( #59554 ), #59588, .T. ) ;
#83366 = CARTESIAN_POINT ( 'NONE',  ( -5.002524092355371543, -284.6265849750445796, -338.0448600208533776 ) ) ;
#83367 = CARTESIAN_POINT ( 'NONE',  ( -96.52280491215569214, -272.0767862475556740, -227.0122298766106894 ) ) ;
#83368 = ORIENTED_EDGE ( 'NONE', *, *, #8361, .F. ) ;
#83369 = DIRECTION ( 'NONE',  ( 0.000000000000000000, -1.000000000000000000, 0.000000000000000000 ) ) ;
#83370 = CARTESIAN_POINT ( 'NONE',  ( 37.45949928069436652, -293.6146311769580848, -288.6859448864928481 ) ) ;
#83372 = CARTESIAN_POINT ( 'NONE',  ( -104.9864642901697067, -286.9502375379933596, -238.6785144397962881 ) ) ;
#83371 = VECTOR ( 'NONE', #83167, 1000.000000000000000 ) ;
#83373 = DIRECTION ( 'NONE',  ( 0.000000000000000000, -1.000000000000000000, 0.000000000000000000 ) ) ;
#83374 = CARTESIAN_POINT ( 'NONE',  ( 25.22466315766302358, -272.4094976428775681, -220.5068182859052968 ) ) ;
#83375 = CARTESIAN_POINT ( 'NONE',  ( -25.80432594554962122, -276.1059232435649733, -346.3285308453869220 ) ) ;
#83376 = CARTESIAN_POINT ( 'NONE',  ( -104.4610361619844952, -288.4807273590805039, -306.4365271129806274 ) ) ;
#83377 = AXIS2_PLACEMENT_3D ( 'NONE', #83124, #32495, #10693 ) ;
#83378 = CARTESIAN_POINT ( 'NONE',  ( -92.16804384127794947, -285.3739220903968885, -319.6221531244599987 ) ) ;
#83379 = CARTESIAN_POINT ( 'NONE',  ( -102.7420114453258719, -279.8467207816627820, -305.0132938261650111 ) ) ;
#83380 = CARTESIAN_POINT ( 'NONE',  ( -97.13078241085194975, -286.6193135897519824, -222.7809547257787699 ) ) ;
#83381 = CARTESIAN_POINT ( 'NONE',  ( 6.060370705028900851, -282.6412053463523648, -209.1952705386757998 ) ) ;
#83382 = CARTESIAN_POINT ( 'NONE',  ( 37.94494193586086794, -275.5160354403257656, -254.1457279098691799 ) ) ;
#83383 = CARTESIAN_POINT ( 'NONE',  ( -22.94098218348056051, -276.7062569876982252, -346.0566890567357063 ) ) ;
#83384 = CARTESIAN_POINT ( 'NONE',  ( -8.653767693668044103, -296.5939800589054016, -339.0649990813101908 ) ) ;
#83385 = DIRECTION ( 'NONE',  ( 0.000000000000000000, 0.000000000000000000, 1.000000000000000000 ) ) ;
#83386 = CARTESIAN_POINT ( 'NONE',  ( -59.75963548836536887, -295.9045011513117629, -197.9342491449833688 ) ) ;
#83387 = CARTESIAN_POINT ( 'NONE',  ( -107.1773006107004136, -277.7736299852884940, -292.0009603506158555 ) ) ;
#83388 = CARTESIAN_POINT ( 'NONE',  ( -68.06630080114807413, -298.7378992605416670, -200.0372572020415873 ) ) ;
#83389 = CARTESIAN_POINT ( 'NONE',  ( -40.03290297085443683, -287.7780167539228273, -196.3967249096531020 ) ) ;
#83390 = CARTESIAN_POINT ( 'NONE',  ( -65.33100169161924953, -296.9315359302708544, -341.3632849548062609 ) ) ;
#83391 = CARTESIAN_POINT ( 'NONE',  ( -24.95680792198181308, -296.1027679658405987, -346.0100330594558500 ) ) ;
#83392 = CARTESIAN_POINT ( 'NONE',  ( -112.1699763204347704, -292.5411176606045842, -271.2314658782549941 ) ) ;
#83393 = CARTESIAN_POINT ( 'NONE',  ( -84.57567925999404679, -277.4001464939907464, -212.2511554480599330 ) ) ;
#83394 = CARTESIAN_POINT ( 'NONE',  ( -103.4456679872251925, -280.9300996767619267, -236.0205183911125744 ) ) ;
#83395 = CARTESIAN_POINT ( 'NONE',  ( 10.10186817582977348, -296.7303688635369667, -195.9367804121130234 ) ) ;
#83396 = CARTESIAN_POINT ( 'NONE',  ( -95.30971361379631901, -285.7446955368546355, -319.1665798725999252 ) ) ;
#83397 = CARTESIAN_POINT ( 'NONE',  ( 35.93834548644947802, -286.5174891728832449, -273.7879314718856563 ) ) ;
#83398 = CARTESIAN_POINT ( 'NONE',  ( 46.71364630202708668, 11.49618872572055928, -331.6741688793942444 ) ) ;
#83399 = ORIENTED_EDGE ( 'NONE', *, *, #584, .T. ) ;
#83400 = CARTESIAN_POINT ( 'NONE',  ( -35.92880368154460058, -285.7370759576803039, -197.3536443206606066 ) ) ;
#83401 = ORIENTED_EDGE ( 'NONE', *, *, #78083, .F. ) ;
#83402 = CARTESIAN_POINT ( 'NONE',  ( -21.77524475299092899, -283.9367973685962738, -345.4555783370901736 ) ) ;
#83403 = CARTESIAN_POINT ( 'NONE',  ( -34.04397020031636600, -274.4280528451893701, -197.4144767702829313 ) ) ;
#83404 = CARTESIAN_POINT ( 'NONE',  ( 22.69033527415341922, -285.7068466318258970, -222.7569785289044262 ) ) ;
#83405 = CARTESIAN_POINT ( 'NONE',  ( -3.771362608470006705, -281.4255067774773238, -201.3114902957267986 ) ) ;
#83406 = CARTESIAN_POINT ( 'NONE',  ( -92.58529693527088966, -280.7991213201947858, -217.6467106564701055 ) ) ;
#83407 = CARTESIAN_POINT ( 'NONE',  ( 39.16126474362443588, -281.7726827342077627, -261.3482260640716959 ) ) ;
#83408 = CARTESIAN_POINT ( 'NONE',  ( 34.45848030099739390, -291.0523547857347353, -270.3937649182068412 ) ) ;
#83409 = CARTESIAN_POINT ( 'NONE',  ( -94.77334838489042568, -240.6273343624868062, -341.9136549172818036 ) ) ;
#83410 = ORIENTED_EDGE ( 'NONE', *, *, #15163, .T. ) ;
#83411 = CARTESIAN_POINT ( 'NONE',  ( -62.67366924264906913, -275.7218535603614100, -199.9457804022509038 ) ) ;
#83412 = CARTESIAN_POINT ( 'NONE',  ( 102.5922281513134919, 116.6502060167416630, -282.7433585466509953 ) ) ;
#83413 = CARTESIAN_POINT ( 'NONE',  ( 32.89385920118760964, -279.9032344003597927, -295.7885500806293066 ) ) ;
#83414 = CARTESIAN_POINT ( 'NONE',  ( -14.19672073583915406, -294.1082850755699951, -197.9298951725927793 ) ) ;
#83415 = CARTESIAN_POINT ( 'NONE',  ( -68.56840588567902728, -294.8222150961618695, -336.4716579983996780 ) ) ;
#83416 = CARTESIAN_POINT ( 'NONE',  ( -103.1599465381613072, -290.5814069812535649, -230.4151532101164719 ) ) ;
#83417 = PLANE ( 'NONE',  #14292 ) ;
#83419 = CARTESIAN_POINT ( 'NONE',  ( 4.046591436637537065, -286.8845311378838119, -331.5246905276018765 ) ) ;
#83418 = CARTESIAN_POINT ( 'NONE',  ( -111.4020735775331445, -294.8891497395210308, -289.2200370318740283 ) ) ;
#83420 = CARTESIAN_POINT ( 'NONE',  ( 36.12684947545425018, -295.2745311739885210, -259.7197975918480211 ) ) ;
#83421 = CARTESIAN_POINT ( 'NONE',  ( -108.9016642274088582, -285.6472534599096207, -287.1616447437694433 ) ) ;
#83422 = EDGE_LOOP ( 'NONE', ( #22550, #44601, #14753, #3903 ) ) ;
#83423 = CARTESIAN_POINT ( 'NONE',  ( -11.24455104975812425, -293.3251819477607114, -198.1127417469649856 ) ) ;
#83424 = CARTESIAN_POINT ( 'NONE',  ( -4.794121284811317274, -283.1037881810158297, -335.7724591498637210 ) ) ;
#83425 = CARTESIAN_POINT ( 'NONE',  ( -44.77246218567561442, -293.9390128652876228, -346.6559213921134415 ) ) ;
#83426 = CARTESIAN_POINT ( 'NONE',  ( -87.27172989295904415, -290.5301540142922931, -328.8360552638200147 ) ) ;
#83427 = EDGE_CURVE ( 'NONE', #70176, #5433, #32334, .T. ) ;
#83428 = CARTESIAN_POINT ( 'NONE',  ( -113.1125059952144767, -291.2116328229413398, -257.0077707773682505 ) ) ;
#83429 = CARTESIAN_POINT ( 'NONE',  ( -109.1785398885511995, -290.5476111811140072, -283.3406579493222353 ) ) ;
#83430 = ORIENTED_EDGE ( 'NONE', *, *, #41338, .F. ) ;
#83431 = CARTESIAN_POINT ( 'NONE',  ( -106.0363124427144754, -297.9968568859628704, -302.3197743487646676 ) ) ;
#83432 = CARTESIAN_POINT ( 'NONE',  ( -112.0526032524244897, -271.5597887483050386, -253.4410212040034196 ) ) ;
#83433 = ADVANCED_FACE ( 'NONE', ( #23554 ), #45768, .F. ) ;
#83434 = CARTESIAN_POINT ( 'NONE',  ( -59.79440787993041084, -278.8128975124869271, -200.5990769741631539 ) ) ;
#83435 = ORIENTED_EDGE ( 'NONE', *, *, #51069, .T. ) ;
#83436 = ORIENTED_EDGE ( 'NONE', *, *, #70625, .F. ) ;
#83437 = CARTESIAN_POINT ( 'NONE',  ( -13.07594815375333930, -273.8668476596614028, -197.3494738136759850 ) ) ;
#83438 = CARTESIAN_POINT ( 'NONE',  ( -88.59417177527213028, -295.7975433669884637, -217.3381036303860583 ) ) ;
#83439 = CARTESIAN_POINT ( 'NONE',  ( 19.26541006732544759, -278.0840356577512580, -318.3871583984513904 ) ) ;
#83440 = CARTESIAN_POINT ( 'NONE',  ( 36.24804142996119083, -273.5650185599660063, -260.5930364160385011 ) ) ;
#83441 = AXIS2_PLACEMENT_3D ( 'NONE', #63816, #6966, #42459 ) ;
#83442 = CARTESIAN_POINT ( 'NONE',  ( -67.44410390668862476, -296.6610922589126744, -337.3149881339224407 ) ) ;
#83443 = CARTESIAN_POINT ( 'NONE',  ( -68.19008139768868659, -298.7169311966987948, -203.8447372838440685 ) ) ;
#83444 = DIRECTION ( 'NONE',  ( 1.000000000000000000, 0.000000000000000000, 0.000000000000000000 ) ) ;
#83445 = CARTESIAN_POINT ( 'NONE',  ( -110.0304720195537982, -297.8614440644573165, -293.2691992942622505 ) ) ;
#83446 = CARTESIAN_POINT ( 'NONE',  ( -112.2252945396787993, -270.6798292912490638, -261.9436308493769729 ) ) ;
#83447 = CARTESIAN_POINT ( 'NONE',  ( 35.72294778351895417, -294.1728165033564437, -268.0266173076009295 ) ) ;
#83448 = CARTESIAN_POINT ( 'NONE',  ( -107.1243316290799754, -289.4346670870831986, -246.9996270687985316 ) ) ;
#83449 = FACE_OUTER_BOUND ( 'NONE', #65204, .T. ) ;
#83450 = CARTESIAN_POINT ( 'NONE',  ( 38.67594812071207855, -276.1972263816411441, -282.5634380782915400 ) ) ;
#83451 = CARTESIAN_POINT ( 'NONE',  ( -34.48315416847574966, -298.4221895734845589, -197.3398065820845773 ) ) ;
#83452 = AXIS2_PLACEMENT_3D ( 'NONE', #51686, #28547, #26790 ) ;
#83453 = CARTESIAN_POINT ( 'NONE',  ( -19.28750040698190205, -284.8010226849348783, -343.5753643798592520 ) ) ;
#83454 = CARTESIAN_POINT ( 'NONE',  ( 8.897359168909336091, -281.1174375276990531, -331.3139494736201982 ) ) ;
#83455 = CARTESIAN_POINT ( 'NONE',  ( -77.76838110910631485, -276.9281774339719391, -335.8370374268101273 ) ) ;
#83456 = CARTESIAN_POINT ( 'NONE',  ( 175.2296996224750103, 250.0000000000000568, 0.000000000000000000 ) ) ;
#83457 = CARTESIAN_POINT ( 'NONE',  ( -90.86655409766818536, -283.0336673584465643, -320.2378834610705667 ) ) ;
#83458 = CARTESIAN_POINT ( 'NONE',  ( 36.06937697272130094, -279.7596681679433459, -286.5710787778032795 ) ) ;
#83459 = CARTESIAN_POINT ( 'NONE',  ( 22.93814492978057018, -274.7118847282850425, -312.6589417394282577 ) ) ;
#83460 = CARTESIAN_POINT ( 'NONE',  ( -71.06402104504375927, -279.4972802982216535, -337.3663333898606993 ) ) ;
#83461 = FACE_OUTER_BOUND ( 'NONE', #51167, .T. ) ;
#83462 = DIRECTION ( 'NONE',  ( 0.000000000000000000, -0.000000000000000000, -1.000000000000000000 ) ) ;
#83463 = CARTESIAN_POINT ( 'NONE',  ( -34.77913880771958333, -296.3236811867578808, -194.3752002295109662 ) ) ;
#83464 = CARTESIAN_POINT ( 'NONE',  ( -95.61650295640320962, -279.8994201434853153, -317.8583741363235049 ) ) ;
#83465 = SPHERICAL_SURFACE ( 'NONE', #54394, 3.000000000000000000 ) ;
#83466 = CARTESIAN_POINT ( 'NONE',  ( -108.8537920578055491, -286.1590073307670536, -294.7606037356579805 ) ) ;
#83467 = ORIENTED_EDGE ( 'NONE', *, *, #33278, .F. ) ;
#83468 = CARTESIAN_POINT ( 'NONE',  ( 202.4403316624504043, 63.53362652955857470, 6.999999999998341771 ) ) ;
#83469 = CARTESIAN_POINT ( 'NONE',  ( 24.83329132087108349, -284.9835232049495062, -228.3262140529449766 ) ) ;
#83470 = CARTESIAN_POINT ( 'NONE',  ( 152.4536156746142410, 129.7208004331680797, -12.50000000000000000 ) ) ;
#83471 = CARTESIAN_POINT ( 'NONE',  ( -109.5354678547003573, -295.1724987090038326, -283.6667710372168472 ) ) ;
#83472 = CARTESIAN_POINT ( 'NONE',  ( -70.54588100114629867, -287.6342580605751209, -336.7706046577903294 ) ) ;
#83473 = CARTESIAN_POINT ( 'NONE',  ( 60.10016229265469434, 49.69813606028536412, -316.8989054076328671 ) ) ;
#83474 = CARTESIAN_POINT ( 'NONE',  ( -112.3856634378736032, -294.5377763325769820, -271.4678884910789520 ) ) ;
#83475 = CARTESIAN_POINT ( 'NONE',  ( -52.02077281295309064, -284.3475746318123925, -195.4257635182382558 ) ) ;
#83476 = CARTESIAN_POINT ( 'NONE',  ( 33.73536812890394998, -283.4119494634100533, -290.2229100550771932 ) ) ;
#83477 = CARTESIAN_POINT ( 'NONE',  ( -63.58337598135658908, -281.6294238540601214, -341.6727471993660856 ) ) ;
#83478 = CARTESIAN_POINT ( 'NONE',  ( -94.10428572898682376, -289.9028999145141938, -316.2632843355752925 ) ) ;
#83479 = CARTESIAN_POINT ( 'NONE',  ( -96.89312957719243968, -280.5775870478598790, -227.1291602576011712 ) ) ;
#83480 = CARTESIAN_POINT ( 'NONE',  ( 7.232630231837879009, -281.4799188724474561, -212.2821068637000508 ) ) ;
#83481 = CARTESIAN_POINT ( 'NONE',  ( 2.335988668896574971, -290.5036862728474603, -334.4854965381022680 ) ) ;
#83482 = ORIENTED_EDGE ( 'NONE', *, *, #59045, .T. ) ;
#83483 = CARTESIAN_POINT ( 'NONE',  ( -101.2085470588424272, -273.1198838868033363, -227.2542674860649470 ) ) ;
#83484 = CARTESIAN_POINT ( 'NONE',  ( -91.97995764589691703, -293.2473193901424793, -219.4844929036364078 ) ) ;
#83485 = CARTESIAN_POINT ( 'NONE',  ( 150.4957602436334412, 20.99999999999998934, 3.637614988394418880 ) ) ;
#83486 = CARTESIAN_POINT ( 'NONE',  ( -72.08107566293803359, -294.1233781216987495, -198.2974183793908196 ) ) ;
#83487 = EDGE_LOOP ( 'NONE', ( #12164, #55521, #76793, #65442 ) ) ;
#83488 = EDGE_CURVE ( 'NONE', #73999, #2981, #24763, .T. ) ;
#83489 = CARTESIAN_POINT ( 'NONE',  ( 24.54266787001388650, -274.1300837361697518, -313.1167648979428577 ) ) ;
#83490 = LINE ( 'NONE', #91041, #74544 ) ;
#83491 = CARTESIAN_POINT ( 'NONE',  ( -27.86771615180484218, -293.3337838255895917, -346.0226123158192877 ) ) ;
#83492 = CARTESIAN_POINT ( 'NONE',  ( -92.78701748118989201, -296.7367470087901324, -222.7624144439384395 ) ) ;
#83493 = CARTESIAN_POINT ( 'NONE',  ( 6.270381546870561706, -289.9683582228354908, -329.8275374989206057 ) ) ;
#83494 = CARTESIAN_POINT ( 'NONE',  ( -42.98816216063917039, -284.8843999989980489, -344.2095388006447365 ) ) ;
#83495 = CARTESIAN_POINT ( 'NONE',  ( -107.8306215674464568, -292.3554510102356403, -240.8667414716206849 ) ) ;
#83496 = CARTESIAN_POINT ( 'NONE',  ( -64.23126705966906513, -293.0238351612961765, -198.6795392366130102 ) ) ;
#83497 = CARTESIAN_POINT ( 'NONE',  ( -62.79874002224426732, -291.5446184517837764, -201.9437289332097407 ) ) ;
#83498 = CARTESIAN_POINT ( 'NONE',  ( -107.4431108929004353, -286.8987710334055805, -243.7004192748076719 ) ) ;
#83499 = CARTESIAN_POINT ( 'NONE',  ( -39.58938593284456431, -280.1913707393119353, -193.3808800750918522 ) ) ;
#83500 = CARTESIAN_POINT ( 'NONE',  ( -110.9095010193052957, -294.4116173836607686, -287.6535395666318209 ) ) ;
#83501 = CARTESIAN_POINT ( 'NONE',  ( 4.543917342797125336, -282.3373657984004694, -335.0352412674635616 ) ) ;
#83502 = CARTESIAN_POINT ( 'NONE',  ( 34.79231427388593545, -277.6407318583409278, -287.9518260514425378 ) ) ;
#83503 = CARTESIAN_POINT ( 'NONE',  ( -85.28047601435908120, -298.1948066931273615, -330.5268031993605859 ) ) ;
#83504 = CARTESIAN_POINT ( 'NONE',  ( -110.2583065397283946, -276.4296316844952344, -290.9396016805934551 ) ) ;
#83506 = VECTOR ( 'NONE', #46536, 1000.000000000000000 ) ;
#83505 = LINE ( 'NONE', #38087, #16672 ) ;
#83507 = CARTESIAN_POINT ( 'NONE',  ( -86.97523656896281352, -283.2729626921415047, -324.0447068728149702 ) ) ;
#83508 = TOROIDAL_SURFACE ( 'NONE', #42701, 4.499999999999990230, 0.5000000000000000000 ) ;
#83509 = CARTESIAN_POINT ( 'NONE',  ( -42.41913721670286463, -281.1945235871316413, -193.9266470193877865 ) ) ;
#83510 = CARTESIAN_POINT ( 'NONE',  ( 37.49295188953270497, -286.3956630625942239, -253.1973278739361604 ) ) ;
#83511 = CARTESIAN_POINT ( 'NONE',  ( -49.88217404808551692, -293.6502793456660925, -197.3658772377385162 ) ) ;
#83512 = CARTESIAN_POINT ( 'NONE',  ( -1.693978837971687801, -276.1166892704454199, -203.0136578687803137 ) ) ;
#83513=STYLED_ITEM('',(#93731),#27246);
#83514 = CARTESIAN_POINT ( 'NONE',  ( 28.67889689226771566, -277.3737587020327169, -309.0209038182451309 ) ) ;
#83515 = CARTESIAN_POINT ( 'NONE',  ( 16.52972094407187242, -276.0923400715444700, -319.6430337401266115 ) ) ;
#83516 = CARTESIAN_POINT ( 'NONE',  ( -110.9407071720953581, -298.3772169346628971, -283.9676526752120935 ) ) ;
#83517 = CARTESIAN_POINT ( 'NONE',  ( -109.7975279541543046, -282.7929746636296500, -251.6479823908108244 ) ) ;
#83518 = CIRCLE ( 'NONE', #17031, 4.000000000000003553 ) ;
#83519 = CARTESIAN_POINT ( 'NONE',  ( -39.20692436760563027, -291.6960974933989519, -193.3918309911692575 ) ) ;
#83520 = CARTESIAN_POINT ( 'NONE',  ( 36.37570793743105213, -289.3962956810174774, -289.6531931783655978 ) ) ;
#83521 = CARTESIAN_POINT ( 'NONE',  ( 18.72182795199518424, -291.8042567305818693, -223.1265237357260673 ) ) ;
#83522 = VERTEX_POINT ( 'NONE', #67581 ) ;
#83523 = CARTESIAN_POINT ( 'NONE',  ( -79.25592021465617165, -290.0735515596680898, -206.4088780873719600 ) ) ;
#83524 = CARTESIAN_POINT ( 'NONE',  ( -4.819850047954069794, -292.1593566701213263, -204.9681651676269212 ) ) ;
#83525 = ORIENTED_EDGE ( 'NONE', *, *, #72959, .T. ) ;
#83526 = CARTESIAN_POINT ( 'NONE',  ( -43.14513492355533941, -290.2034799911207301, -346.8321102238632534 ) ) ;
#83527 = CARTESIAN_POINT ( 'NONE',  ( -85.50130918654589607, -279.6973397814891769, -215.4726898576277563 ) ) ;
#83528 = CARTESIAN_POINT ( 'NONE',  ( -114.0287313637569611, -295.4821416439342556, -269.5918656632948682 ) ) ;
#83529 = CARTESIAN_POINT ( 'NONE',  ( -21.01370799430131697, -286.9077985944710463, -195.2165276307016768 ) ) ;
#83530 = CARTESIAN_POINT ( 'NONE',  ( 39.33319754247998645, -287.7927842176408149, -262.9550734836485617 ) ) ;
#83531 = CARTESIAN_POINT ( 'NONE',  ( -109.6337561475086204, -285.0211776174291458, -260.0681046597024419 ) ) ;
#83532 = CARTESIAN_POINT ( 'NONE',  ( 102.8821184830924267, 116.5732156867659342, -282.8887793008179870 ) ) ;
#83533 = CARTESIAN_POINT ( 'NONE',  ( -78.94308665734938302, -207.6905716540671278, -356.1245641789462297 ) ) ;
#83534 = CARTESIAN_POINT ( 'NONE',  ( 44.56609888530009300, 11.47358219897120080, -328.3762950272841294 ) ) ;
#83535 = CARTESIAN_POINT ( 'NONE',  ( -8.898633777073184703, -273.6310117220890561, -202.9008987423906376 ) ) ;
#83536 = CARTESIAN_POINT ( 'NONE',  ( 18.53513759638890690, -275.1444237426023847, -317.8164135808054311 ) ) ;
#83537 = CARTESIAN_POINT ( 'NONE',  ( -112.8270871651255618, -296.2469278174632450, -255.4110798984995370 ) ) ;
#83538 = CARTESIAN_POINT ( 'NONE',  ( 104.3072796027752673, 114.1787421069637105, -280.1511098027236812 ) ) ;
#83539 = CARTESIAN_POINT ( 'NONE',  ( 34.26611105204779761, -273.8939975902330275, -243.4237897955941321 ) ) ;
#83540 = CARTESIAN_POINT ( 'NONE',  ( -111.3558677489446183, -274.3479423682161382, -267.6218071371351925 ) ) ;
#83541 = EDGE_LOOP ( 'NONE', ( #32977, #73541, #74938, #19762 ) ) ;
#83542 = CARTESIAN_POINT ( 'NONE',  ( -3.551308916552529560, -299.4067538136396252, -193.5911544943717217 ) ) ;
#83543 = CARTESIAN_POINT ( 'NONE',  ( -50.75661716430504811, -289.7203767828612513, -342.2322550546592765 ) ) ;
#83544 = CARTESIAN_POINT ( 'NONE',  ( -114.1487856353897712, -297.4002016366695784, -266.7530796441062080 ) ) ;
#83545 = CARTESIAN_POINT ( 'NONE',  ( -82.93915359280163102, -297.9395659979604716, -208.3239650866019588 ) ) ;
#83546 = CARTESIAN_POINT ( 'NONE',  ( -80.15306037536085171, -295.8169075192104174, -329.4896850061484201 ) ) ;
#83547 = VERTEX_POINT ( 'NONE', #8857 ) ;
#83548 = CARTESIAN_POINT ( 'NONE',  ( -31.53604330725120164, -278.8996815272684557, -345.7493916958144951 ) ) ;
#83549 = VERTEX_POINT ( 'NONE', #36828 ) ;
#83550 = CARTESIAN_POINT ( 'NONE',  ( 23.70231203714039836, -280.4343936723595334, -223.5084555303059233 ) ) ;
#83551 = UNCERTAINTY_MEASURE_WITH_UNIT (LENGTH_MEASURE( 1.000000000000000082E-05 ), #64964, 'distance_accuracy_value', 'NONE');
#83552 = CARTESIAN_POINT ( 'NONE',  ( -89.24414438008285799, -278.7456658904580422, -322.1007552218759429 ) ) ;
#83553 = CARTESIAN_POINT ( 'NONE',  ( -38.50664539732039060, -278.8267058698347682, -346.3388576137431301 ) ) ;
#83554 = CARTESIAN_POINT ( 'NONE',  ( -73.33391107725348945, -275.5471112762936627, -336.5797862244453427 ) ) ;
#83555 = CARTESIAN_POINT ( 'NONE',  ( -107.2572525056515218, -273.3271543561581325, -248.9791829637545106 ) ) ;
#83556 = CARTESIAN_POINT ( 'NONE',  ( -63.27021795266994530, -296.2824949836247583, -201.4371405066596594 ) ) ;
#83557 = DIRECTION ( 'NONE',  ( -1.000000000000000000, -4.095251346825557639E-15, 0.000000000000000000 ) ) ;
#83558 = CARTESIAN_POINT ( 'NONE',  ( -107.1159935047156324, -278.4325508829217597, -291.9907512978328441 ) ) ;
#83559 = CARTESIAN_POINT ( 'NONE',  ( -23.41823235009659143, -287.5626910537846470, -345.6441027961407713 ) ) ;
#83560 = CARTESIAN_POINT ( 'NONE',  ( -90.76284863589798135, -275.2946102174046246, -217.7191049127725648 ) ) ;
#83561 = CARTESIAN_POINT ( 'NONE',  ( 195.5353459679622290, 20.92212392303436985, -14.58720617293945310 ) ) ;
#83562 = CARTESIAN_POINT ( 'NONE',  ( -109.5801722296861556, -289.5957942488715844, -282.0246663936416667 ) ) ;
#83563 = CARTESIAN_POINT ( 'NONE',  ( -114.0495132143409620, -283.9772938462530192, -264.2480709591835648 ) ) ;
#83564 = CARTESIAN_POINT ( 'NONE',  ( 20.96561177439674495, -280.4258233502402504, -315.9487412495511194 ) ) ;
#83566 = CARTESIAN_POINT ( 'NONE',  ( -104.7798596275713834, -283.0508188132958480, -238.7206201930535485 ) ) ;
#83565 = CARTESIAN_POINT ( 'NONE',  ( 36.01481182132828707, -280.2114044299391935, -276.8207810982214596 ) ) ;
#83567 = CARTESIAN_POINT ( 'NONE',  ( -16.90200753173384385, -288.3161387804996139, -198.1466682588884112 ) ) ;
#83568 = CARTESIAN_POINT ( 'NONE',  ( -96.73600627050431910, -280.3574260664447024, -227.2398134632963718 ) ) ;
#83569 = CARTESIAN_POINT ( 'NONE',  ( 29.33919985515026596, -212.1443419142231051, 25.50000000000000000 ) ) ;
#83570 = AXIS2_PLACEMENT_3D ( 'NONE', #40935, #25355, #11150 ) ;
#83571 = CARTESIAN_POINT ( 'NONE',  ( -22.61216942323112278, -294.2407228081135031, -196.7688180487071179 ) ) ;
#83572 = CARTESIAN_POINT ( 'NONE',  ( -113.3713618042508671, -276.7766952380807766, -271.5696119474641250 ) ) ;
#83573 = TOROIDAL_SURFACE ( 'NONE', #57928, 4.499999999999993783, 0.5000000000000000000 ) ;
#83574 = CARTESIAN_POINT ( 'NONE',  ( -94.85080901949508814, -285.8844174751034188, -318.7827891345715443 ) ) ;
#83575 = VECTOR ( 'NONE', #39326, 1000.000000000000000 ) ;
#83576 = CARTESIAN_POINT ( 'NONE',  ( 197.0936144127869341, 69.78646135765499992, 10.59529938563716200 ) ) ;
#83577 = CARTESIAN_POINT ( 'NONE',  ( -72.48206884650126369, -291.4336579165063199, -337.2670659464135383 ) ) ;
#83578 = AXIS2_PLACEMENT_3D ( 'NONE', #70267, #84898, #20047 ) ;
#83579 = CARTESIAN_POINT ( 'NONE',  ( -112.2279753225190149, -294.4881089321660284, -275.3361550871782129 ) ) ;
#83580 = CARTESIAN_POINT ( 'NONE',  ( 5.099023081603529128, -285.8070168476255617, -206.2435135136128395 ) ) ;
#83581 = CARTESIAN_POINT ( 'NONE',  ( -68.11641715727034807, -290.0410410176143046, -203.2699872277709403 ) ) ;
#83582 = CARTESIAN_POINT ( 'NONE',  ( 175.2296996224750103, 158.6892791692949629, 24.00000000000001066 ) ) ;
#83583 = CARTESIAN_POINT ( 'NONE',  ( 22.86023606935548358, -274.8219652345104009, -312.6025875795114644 ) ) ;
#83584 = CARTESIAN_POINT ( 'NONE',  ( -50.71661875223671245, -293.3643875934328094, -343.3815057487315130 ) ) ;
#83585 = CARTESIAN_POINT ( 'NONE',  ( 196.8872833010042882, 42.02416330566287428, 12.48796469961284572 ) ) ;
#83586 = CARTESIAN_POINT ( 'NONE',  ( -37.77152332136167701, -290.5267452074634775, -194.0556594118756095 ) ) ;
#83587 = CARTESIAN_POINT ( 'NONE',  ( -88.26104537463086785, -286.9245651406856723, -216.9414521880127040 ) ) ;
#83588 = CARTESIAN_POINT ( 'NONE',  ( 25.00723104401543750, -286.3747244374912952, -313.8862593594518557 ) ) ;
#83589 = CIRCLE ( 'NONE', #12587, 7.999911143031724237 ) ;
#83590 = CARTESIAN_POINT ( 'NONE',  ( -110.4560286155236071, -285.8624637120027501, -279.1465748536348883 ) ) ;
#83591 = CARTESIAN_POINT ( 'NONE',  ( 160.5350683151633291, 249.5000000000000568, 25.22542485937379197 ) ) ;
#83592 = CARTESIAN_POINT ( 'NONE',  ( -9.441252023900927881, -287.2291755239171493, -202.7149949180676174 ) ) ;
#83593 = CARTESIAN_POINT ( 'NONE',  ( 37.22056660734074285, -295.3882464338495311, -259.1088065173165660 ) ) ;
#83594 = CARTESIAN_POINT ( 'NONE',  ( -102.3790337418371763, -276.1202220280419510, -308.9275197025054354 ) ) ;
#83595 = CARTESIAN_POINT ( 'NONE',  ( 39.11710122699075498, -276.0027742400349666, -279.7411067331673848 ) ) ;
#83596 = CARTESIAN_POINT ( 'NONE',  ( -22.45314311166790588, -290.3210391183087609, -196.2291638266372331 ) ) ;
#83597 = CARTESIAN_POINT ( 'NONE',  ( -67.36245925523701317, -279.6691571329307635, -199.4544608802166294 ) ) ;
#83598 = CARTESIAN_POINT ( 'NONE',  ( -106.4760059060146489, -298.1632874237901660, -298.5088455074348985 ) ) ;
#83599 = CARTESIAN_POINT ( 'NONE',  ( -48.18343439339133027, -256.1235685799528596, -485.9512705678166640 ) ) ;
#83600 = DIRECTION ( 'NONE',  ( 0.000000000000000000, 0.000000000000000000, -1.000000000000000000 ) ) ;
#83601 = CARTESIAN_POINT ( 'NONE',  ( -109.4845510343781143, -276.9187973830696592, -252.8604166639343305 ) ) ;
#83602 = EDGE_CURVE ( 'NONE', #31710, #51979, #60480, .T. ) ;
#83603 = CARTESIAN_POINT ( 'NONE',  ( 36.68946876235337839, -279.7073047893435387, -282.4572760389032169 ) ) ;
#83604 = EDGE_CURVE ( 'NONE', #41385, #45114, #22606, .T. ) ;
#83605 = CARTESIAN_POINT ( 'NONE',  ( 175.2296996224750103, 140.2072866198470251, -24.00000000000002132 ) ) ;
#83606 = CARTESIAN_POINT ( 'NONE',  ( 6.849372451248299853, -273.1209173928744463, -208.0880875547902065 ) ) ;
#83607 = CARTESIAN_POINT ( 'NONE',  ( 20.24760536984477000, -295.7158373115918266, -316.3614508254897260 ) ) ;
#83608 = AXIS2_PLACEMENT_3D ( 'NONE', #14368, #51245, #78750 ) ;
#83609 = CARTESIAN_POINT ( 'NONE',  ( 35.88466650688650361, -280.1850321800189931, -247.5709503830718461 ) ) ;
#83610 = CARTESIAN_POINT ( 'NONE',  ( -90.57003437736362628, -296.7704952303038795, -320.7347617401772482 ) ) ;
#83611 = CARTESIAN_POINT ( 'NONE',  ( -70.53035978945197826, -298.9388355138526663, -201.4277360464224955 ) ) ;
#83612 = CARTESIAN_POINT ( 'NONE',  ( -33.80998169044987378, -297.9308959821268559, -197.3612213806951843 ) ) ;
#83613 = CARTESIAN_POINT ( 'NONE',  ( -55.52113752425723447, -293.8183571015531470, -197.5977432556503572 ) ) ;
#83614 = CARTESIAN_POINT ( 'NONE',  ( -114.3548223872009260, -284.6876880671820231, -272.8513511617020981 ) ) ;
#83615 = CARTESIAN_POINT ( 'NONE',  ( 0.4106575901258024408, -274.6947651974198266, -336.1097712475500430 ) ) ;
#83616 = CARTESIAN_POINT ( 'NONE',  ( 21.48764901255395543, -288.0547746324221521, -320.0411711650548341 ) ) ;
#83617 = CARTESIAN_POINT ( 'NONE',  ( 22.93677463692982244, -287.1885722299908821, -311.9754517053271456 ) ) ;
#83618 = CARTESIAN_POINT ( 'NONE',  ( -93.20417831708374479, -289.2489799202384120, -220.3172953790736699 ) ) ;
#83619 = ORIENTED_EDGE ( 'NONE', *, *, #85455, .T. ) ;
#83620 = CARTESIAN_POINT ( 'NONE',  ( 84.09003387609358526, 83.72762891241104910, -302.5758382668069544 ) ) ;
#83621 = CARTESIAN_POINT ( 'NONE',  ( 14.12228742805320536, -287.8127915613035839, -322.2209909714188711 ) ) ;
#83622 = DIRECTION ( 'NONE',  ( 0.000000000000000000, 0.000000000000000000, 1.000000000000000000 ) ) ;
#83623 = CARTESIAN_POINT ( 'NONE',  ( -108.0058390277665268, -285.1089571944567069, -300.4870462044021906 ) ) ;
#83624 = CARTESIAN_POINT ( 'NONE',  ( 20.21025720406927562, -291.9207381929551275, -219.5417231869045622 ) ) ;
#83625 = CARTESIAN_POINT ( 'NONE',  ( -1.529620915453896890, -282.1190008418298589, -203.1009113272673972 ) ) ;
#83626 = CARTESIAN_POINT ( 'NONE',  ( 25.86368855657732269, -282.2940102327014529, -227.1598092541180733 ) ) ;
#83627 = CARTESIAN_POINT ( 'NONE',  ( -100.4021996277868851, -283.8807591070132048, -307.1357479241078181 ) ) ;
#83628 = CARTESIAN_POINT ( 'NONE',  ( 20.74635420978414047, -278.2062920974549911, -317.8237358363423937 ) ) ;
#83629 = CARTESIAN_POINT ( 'NONE',  ( -65.54200561698550587, -297.6935812576494982, -198.6539872572283230 ) ) ;
#83630 = CARTESIAN_POINT ( 'NONE',  ( -97.09991869523867081, -287.9580211839782464, -315.1127845529509273 ) ) ;
#83631 = CARTESIAN_POINT ( 'NONE',  ( -79.06826775116425665, -272.2706420845412367, -209.9170738562476402 ) ) ;
#83632 = EDGE_LOOP ( 'NONE', ( #62123, #24031, #45222, #68542 ) ) ;
#83633 = ORIENTED_EDGE ( 'NONE', *, *, #74867, .F. ) ;
#83634 = LINE ( 'NONE', #18797, #53096 ) ;
#83635 = CARTESIAN_POINT ( 'NONE',  ( -92.60639422852541713, -287.1733562218302609, -220.4142353466645261 ) ) ;
#83636 = CARTESIAN_POINT ( 'NONE',  ( 23.79093163603620198, -295.2512064732600834, -316.6676385211700904 ) ) ;
#83637 = CARTESIAN_POINT ( 'NONE',  ( -65.13965640441421101, -286.3306198861232019, -202.6968311293901763 ) ) ;
#83638 = CARTESIAN_POINT ( 'NONE',  ( -9.308939621169331602, -275.7532582758374247, -341.8242871772670242 ) ) ;
#83639 = CARTESIAN_POINT ( 'NONE',  ( -64.36076891912699693, -292.3601814055583077, -198.3099978050392167 ) ) ;
#83640 = CARTESIAN_POINT ( 'NONE',  ( -69.25068512362842910, -283.7764786004359507, -201.6292855902406700 ) ) ;
#83641 = CARTESIAN_POINT ( 'NONE',  ( -77.16196030773112113, -291.8674319771969294, -204.4202724241321789 ) ) ;
#83642 = CARTESIAN_POINT ( 'NONE',  ( -63.82460531587253172, -289.7403612548397973, -338.4648817304469048 ) ) ;
#83643 = FACE_OUTER_BOUND ( 'NONE', #62736, .T. ) ;
#83644 = AXIS2_PLACEMENT_3D ( 'NONE', #3329, #81010, #10427 ) ;
#83645 = CARTESIAN_POINT ( 'NONE',  ( 200.6103193995254230, 250.5000000000000568, -2.464576988612312114 ) ) ;
#83646 = CARTESIAN_POINT ( 'NONE',  ( 189.2201263495670958, 268.0219113037794614, -137.5448743359141019 ) ) ;
#83647 = CARTESIAN_POINT ( 'NONE',  ( -94.79979063882947798, -285.3869565282979011, -320.5734231346647221 ) ) ;
#83648 = CARTESIAN_POINT ( 'NONE',  ( -69.85430415644619018, -283.1237833571632336, -202.7746430608542312 ) ) ;
#83649 = VERTEX_POINT ( 'NONE', #15990 ) ;
#83650 = CARTESIAN_POINT ( 'NONE',  ( 22.83066784913029679, -281.0536917245429436, -312.2360771581774088 ) ) ;
#83651 = CARTESIAN_POINT ( 'NONE',  ( 32.99872845308576075, -275.6181197124072355, -301.6336042677241949 ) ) ;
#83652 = CARTESIAN_POINT ( 'NONE',  ( -107.2355265971909546, -280.9023202287054346, -243.4785825081016810 ) ) ;
#83653 = CARTESIAN_POINT ( 'NONE',  ( -110.6140932004204842, -273.3870535845430823, -283.9357899037859170 ) ) ;
#83654 = CARTESIAN_POINT ( 'NONE',  ( 37.67965657171717453, -279.9440781558708409, -255.8558660642179632 ) ) ;
#83656 = CARTESIAN_POINT ( 'NONE',  ( -92.72503140558073653, -283.2739396131223657, -220.2398861061249704 ) ) ;
#83655 = AXIS2_PLACEMENT_3D ( 'NONE', #59750, #9513, #81031 ) ;
#83657 = CARTESIAN_POINT ( 'NONE',  ( -110.6296720769561972, -274.6593297104210478, -250.9460721357923489 ) ) ;
#83658 = PRODUCT ( 'MAS-324', 'MAS-324', '', ( #69122 ) ) ;
#83659 = CARTESIAN_POINT ( 'NONE',  ( -61.02719283052873323, -295.8602783437192443, -339.5304785176875839 ) ) ;
#83660 = ORIENTED_EDGE ( 'NONE', *, *, #22726, .T. ) ;
#83661 = CARTESIAN_POINT ( 'NONE',  ( -33.46579123389754074, -290.7867488611997260, -196.9576646622759029 ) ) ;
#83662 = CARTESIAN_POINT ( 'NONE',  ( 27.56725041205460514, -276.7457894615187115, -311.6928796239213284 ) ) ;
#83663 = CARTESIAN_POINT ( 'NONE',  ( -6.528980864048501864, -274.4684564035028416, -204.1827504327639531 ) ) ;
#83664 = CARTESIAN_POINT ( 'NONE',  ( 14.66342823393550532, -275.2609211811513319, -326.7979036708752005 ) ) ;
#83665 = CARTESIAN_POINT ( 'NONE',  ( 185.2786201558346306, 214.5679412853093595, 22.89156442063597297 ) ) ;
#83666 = CARTESIAN_POINT ( 'NONE',  ( -107.3513634428434784, -270.9033725294536907, -243.3185114834425065 ) ) ;
#83667 = AXIS2_PLACEMENT_3D ( 'NONE', #33171, #62061, #41175 ) ;
#83668 = CYLINDRICAL_SURFACE ( 'NONE', #42787, 3.000000000000000000 ) ;
#83669 = CARTESIAN_POINT ( 'NONE',  ( 113.5000000000000568, -192.7866584945343504, -447.4016117689005796 ) ) ;
#83670 = AXIS2_PLACEMENT_3D ( 'NONE', #91736, #18376, #19314 ) ;
#83671 = CARTESIAN_POINT ( 'NONE',  ( -23.99578925850525835, -283.9573320297236023, -342.4451851249907008 ) ) ;
#83672 = CARTESIAN_POINT ( 'NONE',  ( 35.51362451769220741, -283.5888259353502008, -292.1311024125701010 ) ) ;
#83673 = CARTESIAN_POINT ( 'NONE',  ( -103.1079902031413269, -283.4678692589171760, -302.3942872770173267 ) ) ;
#83674 = CARTESIAN_POINT ( 'NONE',  ( 19.78808432388189686, -274.6065859171814623, -317.0996303155948226 ) ) ;
#83675 = CARTESIAN_POINT ( 'NONE',  ( 10.72623435313587059, -284.2403092013405512, -327.0002776758514642 ) ) ;
#83676 = CARTESIAN_POINT ( 'NONE',  ( -109.4471449020585538, -276.8331981486666109, -285.5766557105600327 ) ) ;
#83677 = CARTESIAN_POINT ( 'NONE',  ( 2.197429475817664013, -229.5268262511776527, 22.50000000000000000 ) ) ;
#83678 = CARTESIAN_POINT ( 'NONE',  ( -27.26122141817058164, -275.2628131234124567, -197.6972645889283626 ) ) ;
#83679 = CARTESIAN_POINT ( 'NONE',  ( 195.0120035674127337, 41.75829791874501495, 13.59005667143956764 ) ) ;
#83680 = CARTESIAN_POINT ( 'NONE',  ( -96.69923366365264883, -280.0119705313902614, -221.5467817715656338 ) ) ;
#83681 = CIRCLE ( 'NONE', #26244, 203.9779373800640485 ) ;
#83682 = VERTEX_POINT ( 'NONE', #80369 ) ;
#83683 = CARTESIAN_POINT ( 'NONE',  ( 194.5881128153457098, 0.000000000000000000, -47.19625681453479871 ) ) ;
#83684 = CARTESIAN_POINT ( 'NONE',  ( -62.80890407608294623, -287.5845191447024831, -199.0047797732487425 ) ) ;
#83685 = CARTESIAN_POINT ( 'NONE',  ( -23.49827999087680652, -294.0679488439579927, -342.2526671583277107 ) ) ;
#83686 = CARTESIAN_POINT ( 'NONE',  ( -114.2666556469257131, -289.9259366616903435, -268.3490902008105081 ) ) ;
#83687 = CARTESIAN_POINT ( 'NONE',  ( 20.31856066047237519, -285.1447471103097655, -223.9377082656914126 ) ) ;
#83689 = CARTESIAN_POINT ( 'NONE',  ( -110.9788537831871054, -288.8889729717097339, -262.9083591717460990 ) ) ;
#83688 = CARTESIAN_POINT ( 'NONE',  ( 36.27028063202638464, -286.1000840102910843, -268.3140329276992588 ) ) ;
#83690 = CARTESIAN_POINT ( 'NONE',  ( -98.44609493244351484, -286.3186188348701080, -229.6993000141757761 ) ) ;
#83691 = CARTESIAN_POINT ( 'NONE',  ( -39.92038152832244435, -275.0843633331755314, -345.3295050678155462 ) ) ;
#83692 = CARTESIAN_POINT ( 'NONE',  ( -46.39007835770571830, -284.3390262087961560, -194.7002478726284096 ) ) ;
#83693 = CARTESIAN_POINT ( 'NONE',  ( -29.35235599798215134, -300.1523195474867407, -195.3583854697037054 ) ) ;
#83694 = CARTESIAN_POINT ( 'NONE',  ( 36.86089110167503691, -285.7097769764948225, -282.6770705386612690 ) ) ;
#83695 = CARTESIAN_POINT ( 'NONE',  ( 17.23016830472284155, -281.7968823512113659, -221.5213839106548903 ) ) ;
#83696 = CARTESIAN_POINT ( 'NONE',  ( -94.05783607469211915, -291.8692315460991722, -319.6896933938890015 ) ) ;
#83697 = DIRECTION ( 'NONE',  ( -0.000000000000000000, -1.000000000000000000, -0.000000000000000000 ) ) ;
#83698 = CARTESIAN_POINT ( 'NONE',  ( 196.8702642586143270, 40.96915988761478644, 12.42857142857141994 ) ) ;
#83699 = CARTESIAN_POINT ( 'NONE',  ( -98.82230144032514829, -297.8783128380003404, -314.3747118235620519 ) ) ;
#83700 = CARTESIAN_POINT ( 'NONE',  ( 6.101821325143905739, -278.6415284164199306, -209.2247042026039594 ) ) ;
#83701 = CARTESIAN_POINT ( 'NONE',  ( -53.34568327821199318, -291.0492293343397705, -195.1533504221171427 ) ) ;
#83702 = CARTESIAN_POINT ( 'NONE',  ( -95.06443740709715939, -295.5943986711673119, -224.3771423080110878 ) ) ;
#83703 = CARTESIAN_POINT ( 'NONE',  ( 29.75791416870868389, -280.6394854804789247, -300.4674218182362893 ) ) ;
#83704 = CARTESIAN_POINT ( 'NONE',  ( 34.25159369914924667, -273.3654809044871854, -249.7876352249365937 ) ) ;
#83705 = CARTESIAN_POINT ( 'NONE',  ( 22.19443561198040982, -294.2682909721281703, -227.2503748406092257 ) ) ;
#83706 = CARTESIAN_POINT ( 'NONE',  ( 31.98288692825981272, -296.4805209788416391, -303.7098442033570223 ) ) ;
#83707 = CARTESIAN_POINT ( 'NONE',  ( -112.2046667397903263, -295.2193192331176306, -255.5209238969743808 ) ) ;
#83708 = CARTESIAN_POINT ( 'NONE',  ( 23.20775597478778352, -292.4118531398285086, -316.2712190717501244 ) ) ;
#83709 = AXIS2_PLACEMENT_3D ( 'NONE', #27244, #85921, #14460 ) ;
#83710 = CARTESIAN_POINT ( 'NONE',  ( -110.3720588842078740, -291.8589733440334157, -279.4132788741173954 ) ) ;
#83711 = EDGE_CURVE ( 'NONE', #9616, #29874, #11159, .T. ) ;
#83712 = PLANE ( 'NONE',  #14282 ) ;
#83713 = CARTESIAN_POINT ( 'NONE',  ( -57.70967943973177228, -292.5853005307996568, -200.0390167523388527 ) ) ;
#83714 = CARTESIAN_POINT ( 'NONE',  ( -18.20453976106250948, -63.49190233628851132, 22.50000000000000000 ) ) ;
#83716 = CARTESIAN_POINT ( 'NONE',  ( 33.44606184527689408, -293.7875351576128651, -288.1962730086082729 ) ) ;
#83715 = CARTESIAN_POINT ( 'NONE',  ( -105.5282640988716736, -282.1524235935357297, -302.4391368366162851 ) ) ;
#83717 = VECTOR ( 'NONE', #7875, 1000.000000000000000 ) ;
#83718 = CARTESIAN_POINT ( 'NONE',  ( 39.18277429408395562, -281.4394552767052460, -261.3499659589428461 ) ) ;
#83719 = CARTESIAN_POINT ( 'NONE',  ( -111.0889411197778855, -283.9413196168746936, -292.4769865206196755 ) ) ;
#83720 = CARTESIAN_POINT ( 'NONE',  ( -40.04936459777392344, -287.0859725935235929, -345.1962801798966893 ) ) ;
#83721 = EDGE_CURVE ( 'NONE', #19500, #87290, #26306, .T. ) ;
#83722 = CARTESIAN_POINT ( 'NONE',  ( 10.40439963802415413, -279.1770969573357775, -210.7701246941907129 ) ) ;
#83723 = VECTOR ( 'NONE', #39545, 1000.000000000000000 ) ;
#83724 = CARTESIAN_POINT ( 'NONE',  ( 0.5545326242041785925, -287.4800480722837506, -337.0947171187447111 ) ) ;
#83725 = CARTESIAN_POINT ( 'NONE',  ( 195.4738470807140800, 39.72044523931811000, 14.98562018837177590 ) ) ;
#83726 = CARTESIAN_POINT ( 'NONE',  ( 34.99664873470414506, -294.9615744125441665, -255.7459306463501605 ) ) ;
#83727 = CARTESIAN_POINT ( 'NONE',  ( 27.16124974261197522, -277.5195238057606844, -311.4226089470499232 ) ) ;
#83728 = CARTESIAN_POINT ( 'NONE',  ( -89.48570549627913806, -278.9592817926890689, -219.1710697254665945 ) ) ;
#83729 = CARTESIAN_POINT ( 'NONE',  ( 13.27688018601567776, -292.9041851990604073, -212.3373355181988416 ) ) ;
#83730 = AXIS2_PLACEMENT_3D ( 'NONE', #18875, #5135, #47731 ) ;
#83731 = CARTESIAN_POINT ( 'NONE',  ( -71.11741497043608717, -281.5743188162936690, -337.9519109115691435 ) ) ;
#83732 = AXIS2_PLACEMENT_3D ( 'NONE', #3663, #84117, #32068 ) ;
#83733 = CARTESIAN_POINT ( 'NONE',  ( 20.37571500980241623, -291.9773247881270777, -225.2618984494971244 ) ) ;
#83734 = CARTESIAN_POINT ( 'NONE',  ( -107.9589445449695688, -294.8793984392997913, -245.0983897371746707 ) ) ;
#83735 = ORIENTED_EDGE ( 'NONE', *, *, #68908, .F. ) ;
#83736 = DIRECTION ( 'NONE',  ( -1.000000000000000000, 0.000000000000000000, 0.000000000000000000 ) ) ;
#83737 = TOROIDAL_SURFACE ( 'NONE', #53470, 2.000000000000000000, 1.000000000000000000 ) ;
#83738 = CARTESIAN_POINT ( 'NONE',  ( -18.21041960237902302, -294.3064864114428474, -340.8734044787660764 ) ) ;
#83739 = DIRECTION ( 'NONE',  ( 1.000000000000000000, 0.000000000000000000, 0.000000000000000000 ) ) ;
#83740 = CARTESIAN_POINT ( 'NONE',  ( -37.30987171927208834, -283.5523547857346784, -200.3611179825600459 ) ) ;
#83741 = CARTESIAN_POINT ( 'NONE',  ( -34.75720343727335404, -297.1425210244456707, -193.5968116746220460 ) ) ;
#83742 = CARTESIAN_POINT ( 'NONE',  ( 10.06882940760500134, -278.8368577378015516, -211.1960796480762497 ) ) ;
#83743 = CARTESIAN_POINT ( 'NONE',  ( -40.81098369611125065, -287.3246733916650442, -193.8811083699249309 ) ) ;
#83744 = CARTESIAN_POINT ( 'NONE',  ( 22.74869363240472708, -287.9630191484949933, -311.8336583687811867 ) ) ;
#83745 = CARTESIAN_POINT ( 'NONE',  ( -96.63949041376348248, -279.4645187621603100, -314.1370317710530458 ) ) ;
#83746 = CARTESIAN_POINT ( 'NONE',  ( -112.0302531516438194, -294.5580413597796792, -271.4627843704465135 ) ) ;
#83747 = CARTESIAN_POINT ( 'NONE',  ( -94.40905279170833353, -298.9714244982031346, -223.2108184744342054 ) ) ;
#83748 = AXIS2_PLACEMENT_3D ( 'NONE', #81759, #44383, #80841 ) ;
#83749 = CARTESIAN_POINT ( 'NONE',  ( -69.43884146103015098, -276.2791051981377564, -336.3818797203672375 ) ) ;
#83750 = ORIENTED_EDGE ( 'NONE', *, *, #50836, .F. ) ;
#83751 = CARTESIAN_POINT ( 'NONE',  ( -36.18052107874536460, -297.7330388629878826, -193.3823253170526755 ) ) ;
#83752 = CARTESIAN_POINT ( 'NONE',  ( -53.70166852880146990, -291.1838859353031808, -342.9811264430320534 ) ) ;
#83753 = CARTESIAN_POINT ( 'NONE',  ( 12.88399548592787980, -295.9652470364154055, -327.7357191750959942 ) ) ;
#83754 = CARTESIAN_POINT ( 'NONE',  ( 202.8417115650362064, 291.9636489450775798, -53.99999999997881872 ) ) ;
#83755 = CARTESIAN_POINT ( 'NONE',  ( -106.6705898391738998, -291.5110177175811828, -247.1792776850786595 ) ) ;
#83756 = VERTEX_POINT ( 'NONE', #59076 ) ;
#83757 = CARTESIAN_POINT ( 'NONE',  ( -103.0242062971173169, -296.6806908124781899, -310.3501310955515464 ) ) ;
#83758 = CARTESIAN_POINT ( 'NONE',  ( -94.70988034397520039, -289.3711456539789992, -220.8519292617993131 ) ) ;
#83759 = CARTESIAN_POINT ( 'NONE',  ( -105.2369621212111070, -297.3556261521179067, -233.9716225015516216 ) ) ;
#83760 = DIRECTION ( 'NONE',  ( -0.000000000000000000, -1.000000000000000000, -0.000000000000000000 ) ) ;
#83761 = CARTESIAN_POINT ( 'NONE',  ( 196.1314029556922947, 25.10402156816986974, 13.71726109663742754 ) ) ;
#83762 = CARTESIAN_POINT ( 'NONE',  ( -72.83405174706639684, -291.0336904919063841, -337.9257268898228972 ) ) ;
#83763 = CARTESIAN_POINT ( 'NONE',  ( -111.2869819898779866, -293.6237833571632905, -305.9350535429201159 ) ) ;
#83764 = CARTESIAN_POINT ( 'NONE',  ( -49.74998625019737375, -287.8938299353961838, -196.5108785158396358 ) ) ;
#83765 = CARTESIAN_POINT ( 'NONE',  ( -43.59976985966797969, -284.5494196383076542, -194.1541935519939841 ) ) ;
#83766 = CARTESIAN_POINT ( 'NONE',  ( -65.22891867520753806, -271.6867263491052427, -200.9042931272572901 ) ) ;
#83767 = CARTESIAN_POINT ( 'NONE',  ( -29.86915946427574653, -276.0676374165018387, -196.2971231313207170 ) ) ;
#83768 = CARTESIAN_POINT ( 'NONE',  ( -87.72159621072766811, -287.8418205613744476, -325.2323475115753126 ) ) ;
#83769 = CARTESIAN_POINT ( 'NONE',  ( -53.83883943083342416, -279.1219846508457181, -344.3618179644143424 ) ) ;
#83770 = ORIENTED_EDGE ( 'NONE', *, *, #11869, .F. ) ;
#83772 = CARTESIAN_POINT ( 'NONE',  ( -4.294075338245559870, -279.8482884150208179, -205.1417840895167046 ) ) ;
#83771 = CARTESIAN_POINT ( 'NONE',  ( -69.74029361473012045, -279.6132566577916236, -204.9306757305529914 ) ) ;
#83773 = CARTESIAN_POINT ( 'NONE',  ( -9.311941745198748066, -277.7738555204592217, -341.7461665208114141 ) ) ;
#83774 = CARTESIAN_POINT ( 'NONE',  ( 38.78994780296864064, -280.2345737860297845, -261.4116726539747333 ) ) ;
#83775 = CARTESIAN_POINT ( 'NONE',  ( 191.8115894054295723, 277.2456744639775934, -124.3514335590991351 ) ) ;
#83776 = CARTESIAN_POINT ( 'NONE',  ( 29.73608067869177773, -276.0067991666836633, -232.9236822774168729 ) ) ;
#83777 = ITEM_DEFINED_TRANSFORMATION ( 'NONE', 'NONE', #68826,  #18940 ) ;
#83778 = CARTESIAN_POINT ( 'NONE',  ( -63.33923436811479490, -275.2395878527539139, -198.6196657700898243 ) ) ;
#83779 = CARTESIAN_POINT ( 'NONE',  ( 34.45848030099739390, -278.0519495502701375, -270.3284710469131937 ) ) ;
#83780 = ORIENTED_EDGE ( 'NONE', *, *, #90876, .F. ) ;
#83781 = AXIS2_PLACEMENT_3D ( 'NONE', #29100, #51785, #16744 ) ;
#83782 = DIRECTION ( 'NONE',  ( -0.000000000000000000, -1.000000000000000000, -0.000000000000000000 ) ) ;
#83783 = CARTESIAN_POINT ( 'NONE',  ( 15.24168261024363780, -287.8963673640045613, -219.2806527016049074 ) ) ;
#83784 = CARTESIAN_POINT ( 'NONE',  ( 28.04335104957394265, -289.8233730422027747, -309.0750572626094481 ) ) ;
#83785 = CARTESIAN_POINT ( 'NONE',  ( -108.8084738454747935, -290.1032771662269170, -254.9860432518425455 ) ) ;
#83786 = CARTESIAN_POINT ( 'NONE',  ( 7.513147032221117350, -286.1532649965426458, -207.7849405391121707 ) ) ;
#83787 = CARTESIAN_POINT ( 'NONE',  ( 197.2991597539432860, 24.58358476407964588, 10.37296855621334757 ) ) ;
#83788 = CARTESIAN_POINT ( 'NONE',  ( 3.819701787755762634, -280.8880928513618755, -331.6779581204693272 ) ) ;
#83789 = CARTESIAN_POINT ( 'NONE',  ( 36.21683723239629416, -289.2779869966798287, -259.9861718491330294 ) ) ;
#83790 = CARTESIAN_POINT ( 'NONE',  ( -23.95839367581954349, -281.3579571241756980, -342.8290064511082846 ) ) ;
#83791 = CARTESIAN_POINT ( 'NONE',  ( -59.90082660569489548, -281.0689601138114995, -200.3622609926799782 ) ) ;
#83792 = AXIS2_PLACEMENT_3D ( 'NONE', #38292, #1389, #67207 ) ;
#83793 = CARTESIAN_POINT ( 'NONE',  ( -27.00661709502031371, -277.4095408039930248, -342.6879767574355924 ) ) ;
#83794 = CARTESIAN_POINT ( 'NONE',  ( -113.9929757534116703, -289.3364193224434757, -271.2089663723333501 ) ) ;
#83795 = CARTESIAN_POINT ( 'NONE',  ( -93.80803464921662282, -286.0666591789097311, -218.1706349736725770 ) ) ;
#83796 = CARTESIAN_POINT ( 'NONE',  ( -15.43698499778952637, -286.8205061370775866, -196.5513793784771508 ) ) ;
#83797 = CARTESIAN_POINT ( 'NONE',  ( 33.75990650994296516, -281.5006428796340856, -253.8214221561174213 ) ) ;
#83798 = VERTEX_POINT ( 'NONE', #23071 ) ;
#83799 = CARTESIAN_POINT ( 'NONE',  ( 202.9738562182569694, 293.9636489450776367, -54.00000000000000000 ) ) ;
#83800 = CARTESIAN_POINT ( 'NONE',  ( -108.6941563864936739, -292.0839460738015418, -295.9945958192292323 ) ) ;
#83801 = CIRCLE ( 'NONE', #62693, 3.589950628481164419 ) ;
#83802 = CARTESIAN_POINT ( 'NONE',  ( -8.680324368668214774, -291.1043027850038243, -199.4257684546907967 ) ) ;
#83803 = AXIS2_PLACEMENT_3D ( 'NONE', #56929, #72064, #84823 ) ;
#83804 = CARTESIAN_POINT ( 'NONE',  ( 31.34313224059402714, -274.2731225449401791, -244.9484784058903131 ) ) ;
#83805 = CARTESIAN_POINT ( 'NONE',  ( -37.69684412098850856, -294.4050444960540176, -347.2714263640753529 ) ) ;
#83806 = CARTESIAN_POINT ( 'NONE',  ( -33.45266957547072906, -290.5818340151796519, -196.7578611941518147 ) ) ;
#83807 = B_SPLINE_CURVE_WITH_KNOTS ( 'NONE', 3,
 ( #54873, #83754, #19832, #26939, #76663, #47765, #62472, #41105, #11790, #91314, #48229, #12261, #91788, #55827, #50590, #43021, #58179, #87021, #7045, #93657, #64833, #21714, #21238, #14156, #78081, #28817, #14619, #34978, #64377, #56788 ),
 .UNSPECIFIED., .F., .F.,
 ( 4, 2, 2, 2, 2, 2, 2, 2, 2, 2, 2, 2, 2, 2, 4 ),
 ( 0.000000000000000000, 0.0003908071623920878011, 0.0007816143247841756021, 0.001172421487176263403, 0.001563228649568351204, 0.002344842974352409279, 0.003126457299136467353, 0.003517264461528496391, 0.003908071623920524561, 0.004298878786312553164, 0.004689685948704582635, 0.005080493111096611239, 0.005471300273488639843, 0.005862107435880668446, 0.006252914598272697050 ),
 .UNSPECIFIED. ) ;
#83808 = CARTESIAN_POINT ( 'NONE',  ( 13.02831800923248196, -292.5772533925004950, -324.6608108447870222 ) ) ;
#83809 = CARTESIAN_POINT ( 'NONE',  ( -42.67754315469100135, -290.3259037179245752, -343.6148609239481857 ) ) ;
#83810 = AXIS2_PLACEMENT_3D ( 'NONE', #47816, #76255, #56357 ) ;
#83811 = CARTESIAN_POINT ( 'NONE',  ( -56.74817810252171313, -291.3023910043950764, -342.8605539464959975 ) ) ;
#83812 = CARTESIAN_POINT ( 'NONE',  ( -17.09535120299540978, -290.3127891164427865, -197.9724878048348558 ) ) ;
#83813 = CARTESIAN_POINT ( 'NONE',  ( -2.273194515521165915, -296.5886059270989108, -336.7140916198875402 ) ) ;
#83814 = CARTESIAN_POINT ( 'NONE',  ( -93.44304845314134411, -286.1597395155926620, -223.2862078405397881 ) ) ;
#83815 = CARTESIAN_POINT ( 'NONE',  ( 22.58319217484764962, -296.1715466622551958, -315.7377167139565586 ) ) ;
#83816 = CARTESIAN_POINT ( 'NONE',  ( -18.97579045949714782, -276.2671760878968712, -197.2244370412116439 ) ) ;
#83817 = CARTESIAN_POINT ( 'NONE',  ( 10.26721067062497994, -275.2071967860114796, -330.4405094951238198 ) ) ;
#83818 = VECTOR ( 'NONE', #56900, 1000.000000000000000 ) ;
#83819 = CARTESIAN_POINT ( 'NONE',  ( -60.09050750711053013, -296.9619142118142463, -196.9119102270677217 ) ) ;
#83820 = CARTESIAN_POINT ( 'NONE',  ( 34.56577036798375957, -274.0207605876565822, -287.9441185455851837 ) ) ;
#83821 = CARTESIAN_POINT ( 'NONE',  ( -46.61201146376574656, -278.0135563864154165, -196.4484954042421805 ) ) ;
#83822 = CARTESIAN_POINT ( 'NONE',  ( -32.68106511887405929, -275.3172437285948604, -197.0995713611181657 ) ) ;
#83823 = CARTESIAN_POINT ( 'NONE',  ( 24.01763491674655526, -273.5167726619777682, -224.8238991709367838 ) ) ;
#83824 = ADVANCED_FACE ( 'NONE', ( #51950 ), #88404, .F. ) ;
#83825 = CARTESIAN_POINT ( 'NONE',  ( -98.58834061380095193, -297.9094438971769705, -230.2512916970663639 ) ) ;
#83826 = LINE ( 'NONE', #84753, #5089 ) ;
#83828 = CARTESIAN_POINT ( 'NONE',  ( 19.00020729366106664, -274.7276416310530180, -223.9435623315623332 ) ) ;
#83827 = CARTESIAN_POINT ( 'NONE',  ( -31.96975626570363360, -287.0049329891199932, -345.5760336180214836 ) ) ;
#83829 = CARTESIAN_POINT ( 'NONE',  ( 37.14441420239932512, -287.7964260024668874, -289.8756964291102918 ) ) ;
#83830 = CARTESIAN_POINT ( 'NONE',  ( -38.92399575944390477, -288.7382159848314700, -347.3237104035712264 ) ) ;
#83831 = CARTESIAN_POINT ( 'NONE',  ( -79.72127913954591349, -299.4627254855557226, -207.9896349472606971 ) ) ;
#83832 = CARTESIAN_POINT ( 'NONE',  ( 30.03437436176456643, -291.9833174549009982, -303.0457475220817969 ) ) ;
#83833 = CARTESIAN_POINT ( 'NONE',  ( 39.11634884246835497, -280.8514686251995727, -278.5115826226154923 ) ) ;
#83834 = CARTESIAN_POINT ( 'NONE',  ( 208.4306832106271088, 42.44233620800392970, 7.500000000000012434 ) ) ;
#83835 = CARTESIAN_POINT ( 'NONE',  ( -7.849339673284405627, -278.4382835502037210, -201.3485681991572562 ) ) ;
#83836 = DIRECTION ( 'NONE',  ( 1.000000000000000000, 0.000000000000000000, -0.000000000000000000 ) ) ;
#83837 = CARTESIAN_POINT ( 'NONE',  ( 3.824691759201260144, -287.2795201743352322, -331.1879993357542276 ) ) ;
#83838 = CARTESIAN_POINT ( 'NONE',  ( 204.6539576904058606, 293.9636489450776367, 3.999999999999991562 ) ) ;
#83839 = LINE ( 'NONE', #90448, #82097 ) ;
#83840 = CARTESIAN_POINT ( 'NONE',  ( -99.95557580891174609, -289.1104353168259991, -228.9811999213561649 ) ) ;
#83841 = CARTESIAN_POINT ( 'NONE',  ( -77.96920197815704512, -299.0966985934662148, -208.6892569347878066 ) ) ;
#83842 = CARTESIAN_POINT ( 'NONE',  ( 31.86646859667727938, -283.3967016165115638, -302.8715703831161932 ) ) ;
#83844 = CARTESIAN_POINT ( 'NONE',  ( -67.78436866182518372, -283.4631951357076218, -336.7105259116786442 ) ) ;
#83843 = CARTESIAN_POINT ( 'NONE',  ( -67.49561044007009514, -295.6788301438177768, -201.2465219436849964 ) ) ;
#83845 = CARTESIAN_POINT ( 'NONE',  ( -89.67384716508622944, -274.7212821661693738, -218.6240780282018648 ) ) ;
#83846 = CARTESIAN_POINT ( 'NONE',  ( 35.53810108040848803, -276.2633003847489590, -263.3952242428138675 ) ) ;
#83847 = EDGE_CURVE ( 'NONE', #4469, #38261, #77690, .T. ) ;
#83848 = CARTESIAN_POINT ( 'NONE',  ( -6.260484085812628940, -284.6439699216946337, -338.6176829535341994 ) ) ;
#83849 = CARTESIAN_POINT ( 'NONE',  ( -102.2979889642521982, -271.9343324569760512, -236.2672922166874798 ) ) ;
#83850 = ORIENTED_EDGE ( 'NONE', *, *, #63587, .F. ) ;
#83851 = CARTESIAN_POINT ( 'NONE',  ( 203.8614262746842201, 292.1666555297790069, -53.99999999998426858 ) ) ;
#83852 = CARTESIAN_POINT ( 'NONE',  ( 38.35686161845388398, -293.5626672673940902, -284.5294341077632794 ) ) ;
#83853 = CARTESIAN_POINT ( 'NONE',  ( -101.0254760614666054, -287.0578934632392247, -231.3238711511847328 ) ) ;
#83854 = DIRECTION ( 'NONE',  ( 0.000000000000000000, 1.000000000000000000, 0.000000000000000000 ) ) ;
#83855 = CARTESIAN_POINT ( 'NONE',  ( -119.3990491898856732, -276.0523547857346784, -270.3284710469131937 ) ) ;
#83856 = CARTESIAN_POINT ( 'NONE',  ( -91.22311014998314249, -276.9914919884159872, -325.2165884382902732 ) ) ;
#83857 = CARTESIAN_POINT ( 'NONE',  ( -82.39620480500543920, -288.0558237848652539, -331.8146127721043968 ) ) ;
#83858 = CARTESIAN_POINT ( 'NONE',  ( -34.80345155149174019, -284.5398496307136043, -344.0232824041333970 ) ) ;
#83859 = CARTESIAN_POINT ( 'NONE',  ( -9.587862702729344377, -278.4446481729323750, -338.9875442448548029 ) ) ;
#83860 = CARTESIAN_POINT ( 'NONE',  ( -100.9187158449311568, -285.4141394514896319, -312.8419807037064402 ) ) ;
#83861 = CARTESIAN_POINT ( 'NONE',  ( -36.20267861888595462, -281.8324784494802202, -343.7493536614051095 ) ) ;
#83862 = CARTESIAN_POINT ( 'NONE',  ( -75.54592218180198415, -281.5430959747556585, -205.7612093468124215 ) ) ;
#83863 = CARTESIAN_POINT ( 'NONE',  ( -38.35954047606500694, -274.2064022054048564, -193.3678455130843474 ) ) ;
#83864 = CARTESIAN_POINT ( 'NONE',  ( -112.1756846062068149, -278.1579804633938693, -288.5512546450444802 ) ) ;
#83865 = CARTESIAN_POINT ( 'NONE',  ( -50.70619976531285289, -297.1443490438134631, -343.5916057907743379 ) ) ;
#83866 = CARTESIAN_POINT ( 'NONE',  ( 222.4306832106270804, -141.7221692137691775, 21.50000000000000000 ) ) ;
#83867 = CARTESIAN_POINT ( 'NONE',  ( 185.4166944662832179, 276.0000000000000568, 23.37680765314684450 ) ) ;
#83868 = CARTESIAN_POINT ( 'NONE',  ( -111.0668489603112192, -294.9136984068614993, -252.8995053916117683 ) ) ;
#83869 = CARTESIAN_POINT ( 'NONE',  ( -5.044520822516396663, -276.1228047087200252, -335.9103585911216783 ) ) ;
#83870 = CARTESIAN_POINT ( 'NONE',  ( -110.6615795018882977, -274.0392125733291664, -247.9940030099612329 ) ) ;
#83871 = CARTESIAN_POINT ( 'NONE',  ( 36.64397342037946714, -289.3568447565173187, -273.7846549246695531 ) ) ;
#83872 = VECTOR ( 'NONE', #47184, 1000.000000000000000 ) ;
#83873 = CARTESIAN_POINT ( 'NONE',  ( -113.2515100987002370, -297.9741855112433768, -278.1334086309209965 ) ) ;
#83874 = CARTESIAN_POINT ( 'NONE',  ( 4.025850345351407178, -295.7136128574110217, -334.8963196889432083 ) ) ;
#83875 = CARTESIAN_POINT ( 'NONE',  ( -93.95986355746282470, -293.2324258621239892, -221.4283886615356778 ) ) ;
#83876 = CARTESIAN_POINT ( 'NONE',  ( -13.70627317335899242, -278.3593261074861402, -199.3035480811219600 ) ) ;
#83877 = CARTESIAN_POINT ( 'NONE',  ( -95.07249317763655938, -281.1245961154930342, -223.3667594332614499 ) ) ;
#83878 = CARTESIAN_POINT ( 'NONE',  ( -111.6482811715772954, -294.6896229378324961, -265.9062095572635940 ) ) ;
#83879 = CARTESIAN_POINT ( 'NONE',  ( -8.487003589242570811, -284.5390178380397970, -340.4718230149956071 ) ) ;
#83880 = AXIS2_PLACEMENT_3D ( 'NONE', #86003, #21615, #50498 ) ;
#83881 = CARTESIAN_POINT ( 'NONE',  ( 26.64386745758308450, -285.9839204023475645, -234.4791109983779620 ) ) ;
#83882 = CARTESIAN_POINT ( 'NONE',  ( 204.9738562182569979, 294.2969822784110079, -54.00000000001656275 ) ) ;
#83883 = VERTEX_POINT ( 'NONE', #30653 ) ;
#83884 = CARTESIAN_POINT ( 'NONE',  ( -94.97112907977204088, -284.8507503115266672, -225.4973504363775589 ) ) ;
#83885 = ORIENTED_EDGE ( 'NONE', *, *, #28405, .T. ) ;
#83886 = CARTESIAN_POINT ( 'NONE',  ( 31.73703595662894728, -282.2013667048361754, -236.9280197314031682 ) ) ;
#83887 = CARTESIAN_POINT ( 'NONE',  ( 51.75741359865251923, -299.6895210198656514, -197.2919279030197401 ) ) ;
#83888 = CARTESIAN_POINT ( 'NONE',  ( -3.650083206593016438, -285.2818066339923462, -201.5507064699835382 ) ) ;
#83889 = CARTESIAN_POINT ( 'NONE',  ( 3.686056364449620482, -281.5306953664110665, -205.4173405899487932 ) ) ;
#83890 = CARTESIAN_POINT ( 'NONE',  ( -48.04088945800175736, -281.4386669150863440, -194.7548937926495967 ) ) ;
#83891 = CARTESIAN_POINT ( 'NONE',  ( 33.54811550065814174, -282.2689621360876799, -300.5035687541375182 ) ) ;
#83892 = CARTESIAN_POINT ( 'NONE',  ( -6.998514795304330072, -280.1237833571632336, -333.4427485647536855 ) ) ;
#83893 = CARTESIAN_POINT ( 'NONE',  ( 195.0332379032363406, 278.6780395204132788, -125.9065900532892783 ) ) ;
#83894 = ORIENTED_EDGE ( 'NONE', *, *, #44228, .F. ) ;
#83895 = CARTESIAN_POINT ( 'NONE',  ( 18.64052951612779907, -276.8593582415225569, -220.6253460462095575 ) ) ;
#83896 = CARTESIAN_POINT ( 'NONE',  ( 121.1092636158038403, 149.8039588042703087, -263.3851840300012555 ) ) ;
#83897 = CARTESIAN_POINT ( 'NONE',  ( 15.06183806717322327, -280.3289999966299320, -323.5913329037326776 ) ) ;
#83898 = CARTESIAN_POINT ( 'NONE',  ( -6.321397510775049966, -294.2141862193411725, -200.9804945590911416 ) ) ;
#83899 = CARTESIAN_POINT ( 'NONE',  ( -31.60261734790722343, -294.3265146052269756, -343.2876046489433861 ) ) ;
#83900 = CARTESIAN_POINT ( 'NONE',  ( -94.66126940491362518, -290.7565496858929350, -219.0386679121750149 ) ) ;
#83901 = DIRECTION ( 'NONE',  ( -0.000000000000000000, 0.000000000000000000, 1.000000000000000000 ) ) ;
#83903 = CARTESIAN_POINT ( 'NONE',  ( 27.72629771473231131, -286.4228632554742831, -305.2921764237661932 ) ) ;
#83902 = CARTESIAN_POINT ( 'NONE',  ( -86.03390104519358772, -294.2867982593514284, -329.2480932924295303 ) ) ;
#83904 = CARTESIAN_POINT ( 'NONE',  ( 15.20710713539905434, -296.1614482322070216, -322.8689835812512570 ) ) ;
#83905 = CARTESIAN_POINT ( 'NONE',  ( -96.98478119270632192, -286.4640131319107468, -227.3984462652104810 ) ) ;
#83906 = EDGE_LOOP ( 'NONE', ( #2501, #15933 ) ) ;
#83907 = CARTESIAN_POINT ( 'NONE',  ( -58.88417168002998636, -292.7213230141007898, -196.6811198025568501 ) ) ;
#83908 = CARTESIAN_POINT ( 'NONE',  ( -58.96036355089380265, -283.8317438056981246, -340.2041435065203814 ) ) ;
#83909 = CARTESIAN_POINT ( 'NONE',  ( -83.95580386430142994, -294.4711059590339346, -331.2156214759936006 ) ) ;
#83910 = CARTESIAN_POINT ( 'NONE',  ( -97.34389577676000727, -291.9992585872445829, -222.3622082161248272 ) ) ;
#83911 = CARTESIAN_POINT ( 'NONE',  ( -81.89984964257409672, -291.9550836814762533, -207.6387279219162565 ) ) ;
#83912 = CARTESIAN_POINT ( 'NONE',  ( 33.08247196139245716, -287.9749944389534448, -289.7694381909022923 ) ) ;
#83913 = ORIENTED_EDGE ( 'NONE', *, *, #33928, .F. ) ;
#83914 = CARTESIAN_POINT ( 'NONE',  ( 139.1539576904058606, 250.5000000000000568, -10.49999999999999822 ) ) ;
#83915 = CARTESIAN_POINT ( 'NONE',  ( -111.3982826323108952, -298.6166201562301126, -254.3027215100758269 ) ) ;
#83916 = CARTESIAN_POINT ( 'NONE',  ( -37.58915063716619898, -296.7339469850733735, -193.8546669906522197 ) ) ;
#83917 = EDGE_CURVE ( 'NONE', #92859, #16590, #16444, .T. ) ;
#83918 = CARTESIAN_POINT ( 'NONE',  ( 21.52523181331077851, -280.0017832391246770, -226.7729005884143305 ) ) ;
#83919 = ORIENTED_EDGE ( 'NONE', *, *, #89946, .T. ) ;
#83920 = CARTESIAN_POINT ( 'NONE',  ( 36.00207379519542172, -275.3521770434582550, -293.6037023895218567 ) ) ;
#83921 = CARTESIAN_POINT ( 'NONE',  ( -109.1482974707535618, -295.2485416031366299, -253.7924628518241548 ) ) ;
#83922 = CARTESIAN_POINT ( 'NONE',  ( -40.53559120196599252, -278.9531250518029992, -344.5402585330048737 ) ) ;
#83923 = CARTESIAN_POINT ( 'NONE',  ( 36.93432641576955433, -273.7081801739291222, -271.6293174504942272 ) ) ;
#83924 = CARTESIAN_POINT ( 'NONE',  ( -101.8087998733637960, -297.2808868785924119, -305.4484882776049517 ) ) ;
#83925 = CARTESIAN_POINT ( 'NONE',  ( -93.86065634821555648, -298.2910649818296633, -223.6528966957968407 ) ) ;
#83926 = DIRECTION ( 'NONE',  ( 0.000000000000000000, 0.000000000000000000, 1.000000000000000000 ) ) ;
#83927 = CARTESIAN_POINT ( 'NONE',  ( -112.8569653684336913, -298.0185950843005003, -280.9392090985708137 ) ) ;
#83928 = CARTESIAN_POINT ( 'NONE',  ( -45.89534905715190405, -295.9437612415042622, -195.6827173879338204 ) ) ;
#83929 = CARTESIAN_POINT ( 'NONE',  ( -70.27405572185325866, -292.2575675818152376, -205.0974020021615161 ) ) ;
#83930 = CARTESIAN_POINT ( 'NONE',  ( -109.2423010203707747, -288.9210545243886372, -286.0939006829962636 ) ) ;
#83931 = DIRECTION ( 'NONE',  ( 1.000000000000000000, 0.000000000000000000, 0.000000000000000000 ) ) ;
#83932 = CARTESIAN_POINT ( 'NONE',  ( 39.56220613950321052, -276.0904791904014246, -274.0347681874903287 ) ) ;
#83933 = CARTESIAN_POINT ( 'NONE',  ( -36.48735443589124117, -298.3964193980501705, -197.3399237719114012 ) ) ;
#83934 = CARTESIAN_POINT ( 'NONE',  ( 29.25610738932950383, -283.0655085084358689, -234.9917681661301856 ) ) ;
#83935 = CARTESIAN_POINT ( 'NONE',  ( 13.34148142253305203, -281.0456735419071492, -327.7422955045147432 ) ) ;
#83936 = CARTESIAN_POINT ( 'NONE',  ( -6.623050125827185219, -276.0078979036036344, -340.8712928156508042 ) ) ;
#83937 = CARTESIAN_POINT ( 'NONE',  ( -84.97463679934691072, -282.9266292620180820, -325.8922360203860080 ) ) ;
#83938 = CARTESIAN_POINT ( 'NONE',  ( -11.36021665909794187, -280.7144261539231138, -340.9500234533661569 ) ) ;
#83939 = EDGE_CURVE ( 'NONE', #45702, #56922, #2249, .T. ) ;
#83940 = CARTESIAN_POINT ( 'NONE',  ( -90.61070835319829087, -271.8534170688649851, -219.5707689357697916 ) ) ;
#83941 = CARTESIAN_POINT ( 'NONE',  ( -98.82319815346400560, -281.1355286006927372, -227.3852875761047869 ) ) ;
#83942 = DIRECTION ( 'NONE',  ( 1.000000000000000000, 0.000000000000000000, 0.000000000000000000 ) ) ;
#83943 = DIRECTION ( 'NONE',  ( -0.9693563597868444237, -0.2456588035076248677, 0.000000000000000000 ) ) ;
#83944 = CARTESIAN_POINT ( 'NONE',  ( -26.36916475778452096, -296.4275949629883371, -194.3776795965844144 ) ) ;
#83945 = VECTOR ( 'NONE', #17174, 1000.000000000000000 ) ;
#83946 = CARTESIAN_POINT ( 'NONE',  ( -70.73298100031612989, -279.4917056420243853, -337.7039037324613560 ) ) ;
#83947 = CARTESIAN_POINT ( 'NONE',  ( -31.14988150182231408, -272.1301938691457849, -195.6041451806287057 ) ) ;
#83948 = CYLINDRICAL_SURFACE ( 'NONE', #33175, 0.5000000000000004441 ) ;
#83949 = CARTESIAN_POINT ( 'NONE',  ( -96.46914734857280393, -287.1141152049804077, -223.3158292909071179 ) ) ;
#83950 = EDGE_LOOP ( 'NONE', ( #92257, #64636, #55823, #59564 ) ) ;
#83951 = CARTESIAN_POINT ( 'NONE',  ( 156.4869342561215433, 15.84738232520326839, -9.998183562659054502 ) ) ;
#83952 = CARTESIAN_POINT ( 'NONE',  ( -36.71322620156909977, -287.0441561253251166, -345.3710874019907919 ) ) ;
#83953 = AXIS2_PLACEMENT_3D ( 'NONE', #60519, #32571, #46279 ) ;
#83954 = DIRECTION ( 'NONE',  ( 0.000000000000000000, 1.000000000000000000, 8.326672684688666165E-15 ) ) ;
#83955 = CARTESIAN_POINT ( 'NONE',  ( 16.43970375136555973, -293.0611164902616679, -320.3080007865403900 ) ) ;
#83956 = CARTESIAN_POINT ( 'NONE',  ( 31.62406566559199206, -286.0548058008955081, -297.9694226751135488 ) ) ;
#83957 = CARTESIAN_POINT ( 'NONE',  ( 154.4364498827578984, 20.25578850496138017, -11.06489058133415959 ) ) ;
#83958 = CARTESIAN_POINT ( 'NONE',  ( -111.7162405794117745, -294.6811226260463741, -260.3039712180333254 ) ) ;
#83959 = CARTESIAN_POINT ( 'NONE',  ( 4.812928341383445385, -285.0898429945812609, -206.6923949498348350 ) ) ;
#83960 = CARTESIAN_POINT ( 'NONE',  ( 35.82316986095185740, -283.0212704428925576, -260.3205806844256358 ) ) ;
#83961 = CARTESIAN_POINT ( 'NONE',  ( 21.20447964399378193, -279.1322222369270776, -221.9223024430743578 ) ) ;
#83962 = CARTESIAN_POINT ( 'NONE',  ( 14.08338210787727718, -288.3050594054060412, -322.1729015556517197 ) ) ;
#83963 = CARTESIAN_POINT ( 'NONE',  ( -109.1859444515794735, -280.1865814893170068, -254.3729092287918547 ) ) ;
#83964 = CARTESIAN_POINT ( 'NONE',  ( -79.15551110448454608, -280.2745213306582173, -210.3260704004291881 ) ) ;
#83965 = EDGE_CURVE ( 'NONE', #45901, #75154, #76195, .T. ) ;
#83966 = CARTESIAN_POINT ( 'NONE',  ( 34.38994614782031078, -289.8286923270100601, -293.4474283241677313 ) ) ;
#83967 = ORIENTED_EDGE ( 'NONE', *, *, #17906, .T. ) ;
#83968 = CARTESIAN_POINT ( 'NONE',  ( -102.7190386961535324, -273.0843339309972180, -229.6818406812649016 ) ) ;
#83969 = CARTESIAN_POINT ( 'NONE',  ( -93.63593261125106437, -291.8478009163669640, -319.4567551299195429 ) ) ;
#83970 = FACE_OUTER_BOUND ( 'NONE', #47429, .T. ) ;
#83971 = CARTESIAN_POINT ( 'NONE',  ( -119.3990491898856732, -293.0519495502701943, -270.3937649182068412 ) ) ;
#83972 = EDGE_LOOP ( 'NONE', ( #60030, #27668, #38585, #72185 ) ) ;
#83973 = CARTESIAN_POINT ( 'NONE',  ( 37.49466387646914001, -273.4550046218384978, -262.7909252614521733 ) ) ;
#83974 = CARTESIAN_POINT ( 'NONE',  ( 175.2296996224750103, 275.0000000000000568, 0.000000000000000000 ) ) ;
#83975 = CARTESIAN_POINT ( 'NONE',  ( -111.1983495673783580, -294.7143219310675022, -289.1658044707526756 ) ) ;
#83976 = CARTESIAN_POINT ( 'NONE',  ( -63.09529223877257920, -297.2152696214330945, -201.9355183477014748 ) ) ;
#83977 = CARTESIAN_POINT ( 'NONE',  ( -34.53236061960532055, -290.5364766707357944, -344.0509371547043997 ) ) ;
#83978 = CARTESIAN_POINT ( 'NONE',  ( -70.65117173693242592, -285.2577022609833648, -336.4695633156177337 ) ) ;
#83979 = CARTESIAN_POINT ( 'NONE',  ( -113.6618864241788600, -291.9305455041455843, -274.0807221493817565 ) ) ;
#83980 = CARTESIAN_POINT ( 'NONE',  ( -113.5175090885641112, -291.9637155526046399, -262.7030824782200398 ) ) ;
#83981 = CARTESIAN_POINT ( 'NONE',  ( -89.09244599986395485, -287.3245327898364962, -216.0761205283811250 ) ) ;
#83982 = CARTESIAN_POINT ( 'NONE',  ( 17.22161360000555419, -280.9709689961040340, -215.9554727689570655 ) ) ;
#83983 = CARTESIAN_POINT ( 'NONE',  ( -112.8691641132310224, -294.6776532690637964, -266.7787020702002678 ) ) ;
#83984 = CARTESIAN_POINT ( 'NONE',  ( -58.48878688903942447, -283.1514003894635607, -344.4558005426727050 ) ) ;
#83985 = CARTESIAN_POINT ( 'NONE',  ( 18.19411868959419820, -276.7196362612757525, -221.0240580767523966 ) ) ;
#83986 = EDGE_CURVE ( 'NONE', #58159, #40166, #44418, .T. ) ;
#83987 = CARTESIAN_POINT ( 'NONE',  ( 30.91033621190086578, -278.2662352645559167, -285.9065529553535612 ) ) ;
#83988 = CARTESIAN_POINT ( 'NONE',  ( -112.5432924226630433, -276.5692437914692050, -279.9984958808888678 ) ) ;
#83989 = CARTESIAN_POINT ( 'NONE',  ( 140.6539576904058606, 249.5000000000000568, -10.49999999999999822 ) ) ;
#83990 = CARTESIAN_POINT ( 'NONE',  ( 33.82175347843743651, -280.8417223679282984, -253.8156862059487935 ) ) ;
#83991 = CARTESIAN_POINT ( 'NONE',  ( -73.89380412828245426, -278.7315646660425159, -337.6958184713817559 ) ) ;
#83992 = CARTESIAN_POINT ( 'NONE',  ( -102.3129323252662033, -284.1479342094740446, -229.4764118025549919 ) ) ;
#83993 = CARTESIAN_POINT ( 'NONE',  ( -47.15064450055134415, -293.6859847864207609, -197.0006475479784740 ) ) ;
#83994 = CARTESIAN_POINT ( 'NONE',  ( 38.12899637370343697, -277.0193627192431904, -259.8437806426530301 ) ) ;
#83995 = CARTESIAN_POINT ( 'NONE',  ( 29.50842678219011717, -276.3806609960516312, -233.0452490753298207 ) ) ;
#83996 = CARTESIAN_POINT ( 'NONE',  ( 34.16413500685495563, -275.5793107147000569, -285.0551829812654319 ) ) ;
#83997 = CARTESIAN_POINT ( 'NONE',  ( -112.2181338329300075, -298.5374536157656848, -271.5162124592046666 ) ) ;
#83998 = CARTESIAN_POINT ( 'NONE',  ( -103.8565817352469338, -283.0067381587821274, -236.0711931027333890 ) ) ;
#83999 = CARTESIAN_POINT ( 'NONE',  ( 37.40243315089014686, -292.9884597069143979, -251.9475677542298797 ) ) ;
#84000 = CARTESIAN_POINT ( 'NONE',  ( 22.67015429275699390, -289.7866894424861925, -317.3397510307340212 ) ) ;
#84001 = CARTESIAN_POINT ( 'NONE',  ( -5.896624094609218325, -291.3958596477193055, -204.1246723523908599 ) ) ;
#84002 = ORIENTED_EDGE ( 'NONE', *, *, #1573, .F. ) ;
#84003 = CARTESIAN_POINT ( 'NONE',  ( 23.51702325323197584, -291.5062184797483269, -224.1354455755057700 ) ) ;
#84004 = CARTESIAN_POINT ( 'NONE',  ( -49.68812433923433503, -291.5571938979070978, -198.3399696207638101 ) ) ;
#84005 = ORIENTED_EDGE ( 'NONE', *, *, #16017, .T. ) ;
#84006 = CARTESIAN_POINT ( 'NONE',  ( 18.42950154959243747, -289.3535682296907225, -323.0020295734032061 ) ) ;
#84007 = CARTESIAN_POINT ( 'NONE',  ( -106.4661191018257256, -279.1999631636301160, -246.6706879880795213 ) ) ;
#84008 = CARTESIAN_POINT ( 'NONE',  ( -96.28270994678318573, -294.8096868399968002, -319.4473130860597507 ) ) ;
#84009 = CARTESIAN_POINT ( 'NONE',  ( -106.5909216263464288, -285.6331027402039808, -236.9267328655530775 ) ) ;
#84010 = CARTESIAN_POINT ( 'NONE',  ( 25.52538447817422806, -287.2971360857175114, -225.9145936532280246 ) ) ;
#84011 = CARTESIAN_POINT ( 'NONE',  ( -51.01769718933186937, -283.5649108888696333, -342.1417447864898804 ) ) ;
#84012 = CARTESIAN_POINT ( 'NONE',  ( 197.4015392562739919, 285.3449900594512201, -111.8235324931284254 ) ) ;
#84013 = CARTESIAN_POINT ( 'NONE',  ( -14.12022291970766474, -91.10070253271963736, -358.9863105665188527 ) ) ;
#84014 = CARTESIAN_POINT ( 'NONE',  ( 200.1442466446337107, 290.5774034492648070, -82.37037781961689120 ) ) ;
#84015 = CARTESIAN_POINT ( 'NONE',  ( 22.41862610576340842, -274.1612628046216855, -228.1339166947878994 ) ) ;
#84016 = CARTESIAN_POINT ( 'NONE',  ( -36.47626270937693960, -275.9614166408631490, -343.6776428654442839 ) ) ;
#84017 = CARTESIAN_POINT ( 'NONE',  ( -98.18144993516297347, -296.6892882913668359, -223.2436612865940333 ) ) ;
#84018 = CARTESIAN_POINT ( 'NONE',  ( 200.2293796500898964, 285.8280805895519165, -96.52018796492004071 ) ) ;
#84019 = CARTESIAN_POINT ( 'NONE',  ( 10.20638625574125413, -275.0971162200386857, -330.3660370820721823 ) ) ;
#84020 = CARTESIAN_POINT ( 'NONE',  ( -111.2016524872315983, -274.3838737416103299, -264.8601563123276605 ) ) ;
#84021 = ORIENTED_EDGE ( 'NONE', *, *, #77324, .F. ) ;
#84022 = CARTESIAN_POINT ( 'NONE',  ( -37.26588926761523624, -298.9943281909984876, -193.5956370025235458 ) ) ;
#84023 =( GEOMETRIC_REPRESENTATION_CONTEXT ( 3 ) GLOBAL_UNCERTAINTY_ASSIGNED_CONTEXT ( ( #40526 ) ) GLOBAL_UNIT_ASSIGNED_CONTEXT ( ( #42925, #86002, #85074 ) ) REPRESENTATION_CONTEXT ( 'NONE', 'WORKASPACE' ) );
#84024 = CARTESIAN_POINT ( 'NONE',  ( 30.01607260997943527, -287.6635068806872368, -241.9296167611089743 ) ) ;
#84025 = CARTESIAN_POINT ( 'NONE',  ( -113.4432621766780898, -297.4892296934866636, -259.6493024644798311 ) ) ;
#84026 = B_SPLINE_CURVE_WITH_KNOTS ( 'NONE', 3,
 ( #38445, #88160, #74916, #75830, #67352, #16217 ),
 .UNSPECIFIED., .F., .F.,
 ( 4, 2, 4 ),
 ( 0.000000000000000000, 0.0005356813221244592508, 0.001071362644248918502 ),
 .UNSPECIFIED. ) ;
#84027 = CARTESIAN_POINT ( 'NONE',  ( -114.0599855068598742, -297.1255947322163706, -263.8818863677628883 ) ) ;
#84028 = CARTESIAN_POINT ( 'NONE',  ( 22.93419184013481882, -294.2928963507961839, -311.6298146364451895 ) ) ;
#84029 = ORIENTED_EDGE ( 'NONE', *, *, #47145, .F. ) ;
#84030 = CARTESIAN_POINT ( 'NONE',  ( 36.22714454532792416, -277.2520323464382841, -253.0729878987292238 ) ) ;
#84031 = CARTESIAN_POINT ( 'NONE',  ( 8.514892865990800530, -280.1687684535842209, -208.5154433925807780 ) ) ;
#84032 = CARTESIAN_POINT ( 'NONE',  ( -71.75417894124989004, -278.4599248798336930, -335.0219151365827770 ) ) ;
#84033 = CARTESIAN_POINT ( 'NONE',  ( 38.13383452523406447, -277.4294042609818689, -279.6021182810642927 ) ) ;
#84034 = CARTESIAN_POINT ( 'NONE',  ( -68.36183585955943443, -275.4777002534902408, -339.0495065716492604 ) ) ;
#84035 = CARTESIAN_POINT ( 'NONE',  ( -36.49022645758874717, -298.7145030422807395, -197.2590868350004314 ) ) ;
#84036 = CARTESIAN_POINT ( 'NONE',  ( -86.90007640237055853, -294.3329166013045324, -324.7609549023745217 ) ) ;
#84037 = FACE_OUTER_BOUND ( 'NONE', #65685, .T. ) ;
#84038 = CARTESIAN_POINT ( 'NONE',  ( 37.61612031612828133, -281.8267443075811798, -252.9581671542618437 ) ) ;
#84039 = CARTESIAN_POINT ( 'NONE',  ( -109.4917394183918731, -278.5723094211032844, -281.4684054514589775 ) ) ;
#84040 = CARTESIAN_POINT ( 'NONE',  ( 27.02080290780034488, -286.7842160521863661, -311.8201808807108364 ) ) ;
#84041 = CARTESIAN_POINT ( 'NONE',  ( -21.03319204225030958, -300.2560068086375509, -195.1888979627098308 ) ) ;
#84042 = CARTESIAN_POINT ( 'NONE',  ( 195.1488485761295237, 20.98501176085694198, -15.11070357071327663 ) ) ;
#84043 = CARTESIAN_POINT ( 'NONE',  ( -37.27811971085482412, -288.2485018991895913, -343.5225674290333018 ) ) ;
#84044 = CARTESIAN_POINT ( 'NONE',  ( -32.87983607865182734, -278.3489949400248520, -196.4823944983590138 ) ) ;
#84046 = CARTESIAN_POINT ( 'NONE',  ( -96.27110465456443933, -282.0038381080028103, -315.8642323000574947 ) ) ;
#84045 = CARTESIAN_POINT ( 'NONE',  ( -22.05442270774257096, -278.8264288725645201, -198.3249938738417768 ) ) ;
#84047 = CARTESIAN_POINT ( 'NONE',  ( -97.94282031743513528, -287.1546922776474844, -226.1525944406728286 ) ) ;
#84048 = CARTESIAN_POINT ( 'NONE',  ( -99.50325845363026644, -279.2200745085292510, -309.4825682434608325 ) ) ;
#84049 = CARTESIAN_POINT ( 'NONE',  ( 153.4663172977970760, 19.61030786773756063, -12.30588869046549227 ) ) ;
#84050 = CARTESIAN_POINT ( 'NONE',  ( 19.77046764803288070, -294.8791675434364947, -221.7287412414027017 ) ) ;
#84051 = CARTESIAN_POINT ( 'NONE',  ( 24.07452561535351876, -276.7527802741784058, -310.1021667802164643 ) ) ;
#84052 = CARTESIAN_POINT ( 'NONE',  ( -87.08866284598654772, -285.7427942203126463, -326.7801127295439869 ) ) ;
#84053 = CARTESIAN_POINT ( 'NONE',  ( 196.1374725241009287, 72.62824853675920167, 11.78667506127216491 ) ) ;
#84054 = CARTESIAN_POINT ( 'NONE',  ( -112.7522582662717667, -292.5328441232037449, -265.6111793545458113 ) ) ;
#84055 = CARTESIAN_POINT ( 'NONE',  ( -96.78370317882382778, -293.9252633432229231, -316.1163539989306628 ) ) ;
#84056 = CARTESIAN_POINT ( 'NONE',  ( 32.56936838143245438, -286.3394379635957421, -238.3488094514989939 ) ) ;
#84057 = DIRECTION ( 'NONE',  ( -1.000000000000000000, -0.000000000000000000, -0.000000000000000000 ) ) ;
#84058 = CARTESIAN_POINT ( 'NONE',  ( 33.33890541901754290, -273.9703632588102664, -250.0422061126269568 ) ) ;
#84059 = CARTESIAN_POINT ( 'NONE',  ( 21.48781892466489296, -292.3186021792932365, -315.6583313237310904 ) ) ;
#84060 = FACE_OUTER_BOUND ( 'NONE', #22367, .T. ) ;
#84061 = CARTESIAN_POINT ( 'NONE',  ( -105.3770830688679041, -289.4822640335980850, -235.6918926359713566 ) ) ;
#84062 = CARTESIAN_POINT ( 'NONE',  ( -109.9840649319341139, -286.3231102046467527, -257.2696543365985349 ) ) ;
#84063 = CARTESIAN_POINT ( 'NONE',  ( 38.68820804717498874, -285.8071789043202671, -271.5579962621189907 ) ) ;
#84064 = CARTESIAN_POINT ( 'NONE',  ( -109.2444953758464550, -286.1831778277103240, -254.6381563084175070 ) ) ;
#84065 = PLANE ( 'NONE',  #54669 ) ;
#84066 = CARTESIAN_POINT ( 'NONE',  ( -57.44855760783973864, -286.5888707866337768, -199.9641180728100949 ) ) ;
#84067 = CARTESIAN_POINT ( 'NONE',  ( 3.234173688355151288, -294.5738760214815102, -206.8012072149851406 ) ) ;
#84068 = CARTESIAN_POINT ( 'NONE',  ( 34.37118292351006232, -273.3247653061418987, -246.3931547603452827 ) ) ;
#84069 = CARTESIAN_POINT ( 'NONE',  ( -4.000165905497466312, -276.9576899198232809, -339.7592308261783955 ) ) ;
#84070 = CARTESIAN_POINT ( 'NONE',  ( 14.46890927587927855, -290.8534963126913340, -215.2894829904719529 ) ) ;
#84071 = CARTESIAN_POINT ( 'NONE',  ( -96.81743442926509147, -279.2092680636500290, -221.4362485684084163 ) ) ;
#84072 = CARTESIAN_POINT ( 'NONE',  ( -56.19492730656106971, -297.2759710845810446, -342.6393439620219965 ) ) ;
#84073 = CARTESIAN_POINT ( 'NONE',  ( -43.52140980873610943, -250.2833644051135593, -485.0314067457711076 ) ) ;
#84074 = LINE ( 'NONE', #33903, #4253 ) ;
#84075 = CARTESIAN_POINT ( 'NONE',  ( -57.51377248618479143, -284.4712050929588827, -199.6375725737202345 ) ) ;
#84076 = CARTESIAN_POINT ( 'NONE',  ( -87.95470032532377047, -275.9086753290813476, -324.6675604123684025 ) ) ;
#84077 = CARTESIAN_POINT ( 'NONE',  ( 29.28837393571043535, -280.0076609207429783, -304.7912483337048570 ) ) ;
#84078 = CARTESIAN_POINT ( 'NONE',  ( 85.55100297371609486, -298.0521521680024080, -521.1711561948568487 ) ) ;
#84079 = CARTESIAN_POINT ( 'NONE',  ( 0.8651884253017493309, -273.0320172676609900, -204.2934029561769478 ) ) ;
#84080 = CARTESIAN_POINT ( 'NONE',  ( -89.16392737490745901, -277.1532573706602989, -321.9921915233116465 ) ) ;
#84081 = CIRCLE ( 'NONE', #43282, 0.5000000000000000000 ) ;
#84082 = CARTESIAN_POINT ( 'NONE',  ( -20.67270286735145390, -296.3545195133043535, -342.1970915529847730 ) ) ;
#84083 = CARTESIAN_POINT ( 'NONE',  ( -14.30744618961798587, -279.2642055532322161, -197.1554856837258853 ) ) ;
#84084 = CARTESIAN_POINT ( 'NONE',  ( -23.46253366839147247, -295.8117527629580650, -342.3210061666968613 ) ) ;
#84085 = CARTESIAN_POINT ( 'NONE',  ( -113.8450012276363452, -297.8766016269611896, -269.6241021796294035 ) ) ;
#84086 = CARTESIAN_POINT ( 'NONE',  ( -107.9594333187077666, -272.4664596222390287, -251.5870827923643560 ) ) ;
#84087 = CARTESIAN_POINT ( 'NONE',  ( -73.61600686124847925, -293.5712964401704994, -204.6584400530958874 ) ) ;
#84088 = CARTESIAN_POINT ( 'NONE',  ( -60.51194358135362705, -285.9265441287558360, -196.8743503303824411 ) ) ;
#84089 = CARTESIAN_POINT ( 'NONE',  ( 25.03623571854281593, -274.2698057247270071, -313.4553565712622003 ) ) ;
#84090 = CARTESIAN_POINT ( 'NONE',  ( -70.64099185393729385, -289.3124471222094485, -339.8029557224502923 ) ) ;
#84091 = CARTESIAN_POINT ( 'NONE',  ( -111.2540434131667837, -280.6712590650361108, -259.5703077420575937 ) ) ;
#84092 = ADVANCED_FACE ( 'NONE', ( #25862 ), #61423, .T. ) ;
#84093 = CARTESIAN_POINT ( 'NONE',  ( 33.30570359326348751, -286.8672414200647154, -289.8456332267057292 ) ) ;
#84094 = CARTESIAN_POINT ( 'NONE',  ( -97.58256009286091626, -289.1620496524165560, -225.6625560703271560 ) ) ;
#84095 = ORIENTED_EDGE ( 'NONE', *, *, #61560, .T. ) ;
#84096 = CARTESIAN_POINT ( 'NONE',  ( 176.3450237082407170, 252.7779579681928510, -162.7338909149122799 ) ) ;
#84097 = CARTESIAN_POINT ( 'NONE',  ( 16.05165294194905101, -287.7771754688169494, -320.3063537571177903 ) ) ;
#84098 = CARTESIAN_POINT ( 'NONE',  ( -22.78264641048746597, -118.9815703160634541, 22.50000000000000000 ) ) ;
#84099 = CARTESIAN_POINT ( 'NONE',  ( 1.983925090223331411, -283.4804891399954272, -336.2877090822796049 ) ) ;
#84100 = CARTESIAN_POINT ( 'NONE',  ( -50.51415945297529930, -290.9466217737974034, -194.7350211132831532 ) ) ;
#84101 = CARTESIAN_POINT ( 'NONE',  ( -14.48732101090178581, -281.9435737816559708, -197.6138661300338413 ) ) ;
#84102 = CARTESIAN_POINT ( 'NONE',  ( 35.69988107971254720, -282.5794911401022773, -247.5965471005750373 ) ) ;
#84103 = CARTESIAN_POINT ( 'NONE',  ( 22.11472592452164676, -280.7938085092188203, -228.0062669549850227 ) ) ;
#84104 = CARTESIAN_POINT ( 'NONE',  ( -32.58905962465235717, -276.1122001142012437, -195.4989794687439826 ) ) ;
#84105 = CARTESIAN_POINT ( 'NONE',  ( 15.47868649755001336, -294.3296984442216626, -326.3879575928647796 ) ) ;
#84106 = CARTESIAN_POINT ( 'NONE',  ( -101.1038103990866261, -289.0950241070623292, -231.5508088503772797 ) ) ;
#84107 = CARTESIAN_POINT ( 'NONE',  ( -93.20608206901290771, -272.0207578132187791, -222.7360364352874740 ) ) ;
#84108 = ORIENTED_EDGE ( 'NONE', *, *, #81466, .F. ) ;
#84109 = CARTESIAN_POINT ( 'NONE',  ( -110.8468703588214197, -286.6254919794216107, -258.5199343540625136 ) ) ;
#84110 = CARTESIAN_POINT ( 'NONE',  ( 36.80126305851634783, -294.8782301631092082, -289.9650339302096427 ) ) ;
#84111 = CARTESIAN_POINT ( 'NONE',  ( 15.90579520830188009, -282.9242760943060944, -320.5200533919816053 ) ) ;
#84112 = CARTESIAN_POINT ( 'NONE',  ( -37.13965649441264105, -276.1083988886247766, -347.1385774689009054 ) ) ;
#84113 = CARTESIAN_POINT ( 'NONE',  ( -99.95288238541117209, -291.7956531773915003, -225.7163798482874029 ) ) ;
#84114 = CARTESIAN_POINT ( 'NONE',  ( -111.1509623143276002, -282.9091233968073311, -253.2585362915878875 ) ) ;
#84115 = CARTESIAN_POINT ( 'NONE',  ( -16.63638181658769710, -292.6458551365373069, -196.2191320025335983 ) ) ;
#84116 = CARTESIAN_POINT ( 'NONE',  ( -80.41655661549687295, -289.9870829716154503, -329.3871107777642351 ) ) ;
#84117 = DIRECTION ( 'NONE',  ( 0.9764705882352960886, 0.000000000000000000, -0.2156506209390900708 ) ) ;
#84118 = DIRECTION ( 'NONE',  ( -0.000000000000000000, -0.000000000000000000, -1.000000000000000000 ) ) ;
#84119 = CARTESIAN_POINT ( 'NONE',  ( -62.54974233798310479, -182.8716734317700059, -358.6490213108781973 ) ) ;
#84120 = CARTESIAN_POINT ( 'NONE',  ( -4.445045077233600317, -284.1466242025010160, -339.2268973405530801 ) ) ;
#84121 = CARTESIAN_POINT ( 'NONE',  ( 31.98288692825983404, -278.6237833571634610, -237.0123917617631264 ) ) ;
#84122 = ORIENTED_EDGE ( 'NONE', *, *, #50265, .F. ) ;
#84123 = CARTESIAN_POINT ( 'NONE',  ( 33.25342124041803515, -280.7325826534128623, -290.1235802061776781 ) ) ;
#84124 = CARTESIAN_POINT ( 'NONE',  ( 20.80149208380332126, -275.9009877011904450, -320.8301847100901796 ) ) ;
#84125 = CARTESIAN_POINT ( 'NONE',  ( -62.95991740281284166, -281.7181222957968885, -199.9947108669112197 ) ) ;
#84126 = CARTESIAN_POINT ( 'NONE',  ( -92.74527687321815961, -240.5677590599414657, -340.2624655071006146 ) ) ;
#84127 = CARTESIAN_POINT ( 'NONE',  ( -7.748305180309949414, -279.0071776040894065, -199.8995148093826231 ) ) ;
#84128 = CARTESIAN_POINT ( 'NONE',  ( -108.5626032521937390, -282.2825884632986799, -292.7090431918928743 ) ) ;
#84129 = CARTESIAN_POINT ( 'NONE',  ( -54.38989971596161155, -299.5961930513086600, -196.3115879226694744 ) ) ;
#84130 = CARTESIAN_POINT ( 'NONE',  ( 20.57582070407850239, -294.6709846207678538, -314.9186583508529793 ) ) ;
#84131 = ORIENTED_EDGE ( 'NONE', *, *, #8590, .T. ) ;
#84132 = CARTESIAN_POINT ( 'NONE',  ( -110.8000162012403393, -289.1903879318553550, -273.9162240245674980 ) ) ;
#84133 = CARTESIAN_POINT ( 'NONE',  ( 12.64465708859684057, -277.0275570290629048, -328.7963545995968389 ) ) ;
#84134 = CARTESIAN_POINT ( 'NONE',  ( -11.49022063468854782, -274.3983538089536864, -202.0377449000611989 ) ) ;
#84135 = CARTESIAN_POINT ( 'NONE',  ( -32.68756867312436043, -273.0298186576122816, -193.7984835137264952 ) ) ;
#84136 = CARTESIAN_POINT ( 'NONE',  ( 191.4749582765727212, 14.19731191252289015, 10.00000000000000000 ) ) ;
#84137 = CARTESIAN_POINT ( 'NONE',  ( 26.19300043881516160, -273.0152211563179776, -230.4115952906718690 ) ) ;
#84138 = DIRECTION ( 'NONE',  ( 0.000000000000000000, 0.000000000000000000, 1.000000000000000000 ) ) ;
#84139 = CARTESIAN_POINT ( 'NONE',  ( -43.49340244127498067, -253.3420193263868896, -491.1679700123006569 ) ) ;
#84140 = CARTESIAN_POINT ( 'NONE',  ( 27.13341569566594202, -283.1058317379639107, -305.2493038379324730 ) ) ;
#84141 = CARTESIAN_POINT ( 'NONE',  ( 38.69629718477778368, -283.3066217929751360, -269.9135659252942219 ) ) ;
#84142 = CARTESIAN_POINT ( 'NONE',  ( -91.74644881309394862, -283.2027375975015389, -319.2063423743621229 ) ) ;
#84143 = CARTESIAN_POINT ( 'NONE',  ( 34.66943698811905250, -274.1635129507852184, -286.5689475532380470 ) ) ;
#84144 = CARTESIAN_POINT ( 'NONE',  ( 20.62593492646530535, -282.7682556194789640, -223.9863536133989896 ) ) ;
#84145 = CARTESIAN_POINT ( 'NONE',  ( 34.80405991124247578, -273.8349051508639604, -255.2762199965054037 ) ) ;
#84146 = ADVANCED_FACE ( 'NONE', ( #19247 ), #88277, .T. ) ;
#84147 = CARTESIAN_POINT ( 'NONE',  ( 31.40343704952015003, -276.2937203482857171, -244.8987499155447836 ) ) ;
#84148 = EDGE_CURVE ( 'NONE', #21852, #16590, #77009, .T. ) ;
#84149 = CARTESIAN_POINT ( 'NONE',  ( 154.7659666677267865, 20.47222690886501439, 12.53936336329526391 ) ) ;
#84150 = CARTESIAN_POINT ( 'NONE',  ( -98.45415997985492140, -279.9774089783627460, -223.7625830552324544 ) ) ;
#84151 = ORIENTED_EDGE ( 'NONE', *, *, #66023, .T. ) ;
#84152 = DIRECTION ( 'NONE',  ( 0.000000000000000000, 1.000000000000000000, 0.000000000000000000 ) ) ;
#84153 = CARTESIAN_POINT ( 'NONE',  ( -82.55801139516458420, -287.3026708528473705, -209.5026648110881240 ) ) ;
#84154 = CARTESIAN_POINT ( 'NONE',  ( -92.31875823276899951, -295.0617875245883965, -318.6324843339914992 ) ) ;
#84155 = CARTESIAN_POINT ( 'NONE',  ( -73.13379150882238378, -288.8625063329561726, -338.4364093612530269 ) ) ;
#84156 = CARTESIAN_POINT ( 'NONE',  ( 35.96089839981687675, -285.9263390169773515, -280.6856460144163066 ) ) ;
#84158 = CARTESIAN_POINT ( 'NONE',  ( -70.65704831901292948, -289.8464033489443636, -204.2698054596178565 ) ) ;
#84157 = CARTESIAN_POINT ( 'NONE',  ( 36.14220381956344141, -286.0641268539903308, -265.5662513061336085 ) ) ;
#84159 = CARTESIAN_POINT ( 'NONE',  ( -110.7876435044199894, -285.7498025887919653, -270.9275964226225142 ) ) ;
#84160 = CARTESIAN_POINT ( 'NONE',  ( 28.76779551838724203, -274.0232732276390379, -305.8901265657968338 ) ) ;
#84161 = CARTESIAN_POINT ( 'NONE',  ( 25.70701391029787430, -285.3816485845841271, -227.5441083139265004 ) ) ;
#84162 = CARTESIAN_POINT ( 'NONE',  ( -74.80360609122205062, -299.5540184186752413, -205.3276152594367829 ) ) ;
#84163 = CARTESIAN_POINT ( 'NONE',  ( 36.02969781357911927, -285.7619569170653904, -286.7497145249767527 ) ) ;
#84164 = CARTESIAN_POINT ( 'NONE',  ( 26.65866895623448229, -282.0082202143072436, -234.7611010640310383 ) ) ;
#84165 = CARTESIAN_POINT ( 'NONE',  ( 9.115335023604126619, -290.4166657407828893, -329.5185726309060783 ) ) ;
#84166 = CARTESIAN_POINT ( 'NONE',  ( 192.9623460957494956, 276.0000000000000568, 16.90571646082668522 ) ) ;
#84167 = CARTESIAN_POINT ( 'NONE',  ( 195.7604110529815387, 40.59022550416383979, 13.56018423268811546 ) ) ;
#84168 = CARTESIAN_POINT ( 'NONE',  ( -16.87301355762895838, -296.7101221609414097, -343.1500955663910872 ) ) ;
#84169 = CARTESIAN_POINT ( 'NONE',  ( -62.96904363096327018, -277.7184462703167469, -199.8205644995465775 ) ) ;
#84170 = CARTESIAN_POINT ( 'NONE',  ( -7.244010252994506516, -291.6341529826215151, -199.6482547733304216 ) ) ;
#84171 = CARTESIAN_POINT ( 'NONE',  ( -108.6028786984695245, -295.2033262722978293, -251.1217236364072107 ) ) ;
#84172 = CARTESIAN_POINT ( 'NONE',  ( 36.18112764911198553, -280.2137410495790846, -268.5882797660400456 ) ) ;
#84173 = CARTESIAN_POINT ( 'NONE',  ( -5.898930076963702973, -272.5486131059699346, -202.8876682933949098 ) ) ;
#84174 = CARTESIAN_POINT ( 'NONE',  ( 8.549077850769588593, -295.7238615259028620, -327.8310636730936949 ) ) ;
#84175 = CARTESIAN_POINT ( 'NONE',  ( -85.28047601435906699, -292.1948066931273615, -330.5268031993605859 ) ) ;
#84176 = CARTESIAN_POINT ( 'NONE',  ( -100.1687146882973707, -295.6092577201411586, -227.0314204285537016 ) ) ;
#84177 = CARTESIAN_POINT ( 'NONE',  ( 28.68293991188527770, -292.2882148593819807, -308.0801322233219253 ) ) ;
#84178 = CARTESIAN_POINT ( 'NONE',  ( -92.84427723113695663, -291.2932706284533992, -318.7574151495228989 ) ) ;
#84179 = CARTESIAN_POINT ( 'NONE',  ( 205.4738562182569694, 293.9636489450776367, -44.00000000000000000 ) ) ;
#84180 = CARTESIAN_POINT ( 'NONE',  ( -93.57048950920508901, -292.0177802440592814, -223.5342393360562880 ) ) ;
#84181 = EDGE_CURVE ( 'NONE', #28384, #69769, #91308, .T. ) ;
#84182 = CARTESIAN_POINT ( 'NONE',  ( -97.83654019666998636, -291.1263561124667376, -317.3545541766117708 ) ) ;
#84184 = CARTESIAN_POINT ( 'NONE',  ( 4.503643228094607487, -292.6340986130241504, -210.4830406153735964 ) ) ;
#84183 = CARTESIAN_POINT ( 'NONE',  ( 8.194400807653430263, -280.4528263285691878, -330.4016901932679389 ) ) ;
#84185 = CARTESIAN_POINT ( 'NONE',  ( -1.135436626899125612, -280.5191310572261614, -202.4044664811583516 ) ) ;
#84186 = CARTESIAN_POINT ( 'NONE',  ( -55.70125157486767620, -282.9489716560196939, -345.1185334148008792 ) ) ;
#84187 = CARTESIAN_POINT ( 'NONE',  ( 22.62777516957125812, -286.1649596509760727, -315.1451604383891549 ) ) ;
#84188 = CARTESIAN_POINT ( 'NONE',  ( -87.78525365492930632, -281.9051142254384104, -324.8953381684161741 ) ) ;
#84189 = CARTESIAN_POINT ( 'NONE',  ( 35.51949101257611829, -279.7446526922947214, -247.6905516401435818 ) ) ;
#84190 = CARTESIAN_POINT ( 'NONE',  ( 1.377537695269205109, -285.4770654264762584, -204.1467979895461156 ) ) ;
#84191 = CARTESIAN_POINT ( 'NONE',  ( 195.5412247871907994, 40.24049585611148672, 14.88037134915001403 ) ) ;
#84192 = CARTESIAN_POINT ( 'NONE',  ( 9.339282516053144079, -294.3057976799779567, -213.1343177603512800 ) ) ;
#84193 = CARTESIAN_POINT ( 'NONE',  ( -20.24018534709207273, -278.2620162812407330, -344.8878623916620541 ) ) ;
#84194 = CARTESIAN_POINT ( 'NONE',  ( -53.96286600050149929, -276.9380423148875252, -341.5175946211983842 ) ) ;
#84195 = CIRCLE ( 'NONE', #16153, 4.025000000000000355 ) ;
#84196 = CARTESIAN_POINT ( 'NONE',  ( -108.3679536379200101, -291.0970613800869842, -240.6244181514893796 ) ) ;
#84197 = CARTESIAN_POINT ( 'NONE',  ( 14.74289963233940881, -280.4051358223019861, -325.1014930634581219 ) ) ;
#84198 = CARTESIAN_POINT ( 'NONE',  ( 34.55308431079621556, -292.7943042307796873, -284.3091794673383106 ) ) ;
#84199 = CARTESIAN_POINT ( 'NONE',  ( -81.76492123804200673, -295.4474594584571605, -209.8683182010375106 ) ) ;
#84200 = VERTEX_POINT ( 'NONE', #47642 ) ;
#84201 = CARTESIAN_POINT ( 'NONE',  ( 2.197429475817664013, -229.5268262511776527, -22.50000000000000000 ) ) ;
#84202 = CARTESIAN_POINT ( 'NONE',  ( 31.59603316035471821, -293.3832952224719293, -294.7112702006300538 ) ) ;
#84203 = CARTESIAN_POINT ( 'NONE',  ( 198.6884013828325521, 64.61450673763174279, 9.555809373750800972 ) ) ;
#84204 = CARTESIAN_POINT ( 'NONE',  ( 7.450504543161054372, -290.1952119285918457, -214.2458315076590907 ) ) ;
#84205 = CARTESIAN_POINT ( 'NONE',  ( -113.7010580509932538, -271.8566991735337410, -261.7933132546746151 ) ) ;
#84206 = CARTESIAN_POINT ( 'NONE',  ( 29.96875611653377547, -280.1473829829694751, -305.1405365804114354 ) ) ;
#84207 = CARTESIAN_POINT ( 'NONE',  ( 32.25640295642875088, -288.4571037273194634, -238.4625537657218786 ) ) ;
#84208 = CARTESIAN_POINT ( 'NONE',  ( -10.74799410011047129, -286.2421762419389779, -202.3639556289292898 ) ) ;
#84209 = CARTESIAN_POINT ( 'NONE',  ( -64.57149029116656891, -278.9341917377763025, -338.8933746296383447 ) ) ;
#84210 = CARTESIAN_POINT ( 'NONE',  ( -93.44316806302283851, -293.8849180890236426, -319.6000466888648930 ) ) ;
#84211 = CARTESIAN_POINT ( 'NONE',  ( -82.96710108700392539, -297.4459863385596918, -328.7042018548107194 ) ) ;
#84212 = CARTESIAN_POINT ( 'NONE',  ( -104.6415815996227821, -276.9538819635504296, -299.7777200734809071 ) ) ;
#84213 = ORIENTED_EDGE ( 'NONE', *, *, #74984, .T. ) ;
#84214 = CARTESIAN_POINT ( 'NONE',  ( -93.67689133787453670, -295.5033907039386349, -322.8409040926529769 ) ) ;
#84215 = CARTESIAN_POINT ( 'NONE',  ( -111.6853062565581354, -292.5330151408027746, -265.6687439620454256 ) ) ;
#84216 = CARTESIAN_POINT ( 'NONE',  ( 24.25178145173790512, -295.7541794308115755, -315.2460453000618941 ) ) ;
#84217 = DIRECTION ( 'NONE',  ( 0.000000000000000000, 0.000000000000000000, 1.000000000000000000 ) ) ;
#84218 = CARTESIAN_POINT ( 'NONE',  ( 14.16107102299992881, -288.9563676298772634, -322.2394104740536704 ) ) ;
#84219 = CARTESIAN_POINT ( 'NONE',  ( -48.18343439339133027, -258.3625464905638296, -448.5700876443999050 ) ) ;
#84220 = CARTESIAN_POINT ( 'NONE',  ( 13.51590753469923634, -281.4195353792096057, -327.9325061032266717 ) ) ;
#84221 = CARTESIAN_POINT ( 'NONE',  ( -114.0198772851753972, -297.2846351305698818, -263.8873078390062119 ) ) ;
#84222 = CARTESIAN_POINT ( 'NONE',  ( -99.01164022056724434, -289.2842297449119542, -226.3483474409320024 ) ) ;
#84223 = CARTESIAN_POINT ( 'NONE',  ( -78.19483769674188522, -297.8518938605167818, -205.1172259904422219 ) ) ;
#84224 = CARTESIAN_POINT ( 'NONE',  ( 200.4551663813218170, 64.49084098419280053, 0.000000000000000000 ) ) ;
#84225 = CARTESIAN_POINT ( 'NONE',  ( 160.5350683151633291, 275.0000000000000568, 20.22542485937379908 ) ) ;
#84226 = DIRECTION ( 'NONE',  ( 0.000000000000000000, 0.000000000000000000, 1.000000000000000000 ) ) ;
#84227 = CARTESIAN_POINT ( 'NONE',  ( -65.17591355673499720, -290.9293396260902682, -341.4659743038619695 ) ) ;
#84228 = CARTESIAN_POINT ( 'NONE',  ( -72.08107566293803359, -276.1233781216987495, -198.2974183793908196 ) ) ;
#84229 = CARTESIAN_POINT ( 'NONE',  ( 38.76919227837110782, -281.0381773904672968, -281.3358545929219758 ) ) ;
#84230 = CARTESIAN_POINT ( 'NONE',  ( -107.2873500578149191, -286.8987710344947004, -243.7597180105432244 ) ) ;
#84231 = CARTESIAN_POINT ( 'NONE',  ( -21.09144749120965301, -284.8314473139080292, -195.6983054148370798 ) ) ;
#84232 = CARTESIAN_POINT ( 'NONE',  ( 26.86152152137588800, -273.0349971875366464, -231.8162567734447350 ) ) ;
#84233 = CARTESIAN_POINT ( 'NONE',  ( -34.00003006958469598, -276.0146693112488379, -195.9961568719902516 ) ) ;
#84234 = CARTESIAN_POINT ( 'NONE',  ( -111.1241051553056138, -288.7646465966976734, -260.1069912797450456 ) ) ;
#84235 = CARTESIAN_POINT ( 'NONE',  ( -109.4831368209674167, -280.1148041854552275, -293.6797821124986854 ) ) ;
#84236 = ORIENTED_EDGE ( 'NONE', *, *, #85093, .T. ) ;
#84238 = CARTESIAN_POINT ( 'NONE',  ( 35.52990753708684224, -280.9851388785493214, -276.7683184864600321 ) ) ;
#84237 = CARTESIAN_POINT ( 'NONE',  ( -34.31332839501501297, -280.0912474586286862, -197.4114168354948049 ) ) ;
#84239 = CARTESIAN_POINT ( 'NONE',  ( 24.12817021593569677, -277.2442940841727932, -316.2190240676875419 ) ) ;
#84240 = CARTESIAN_POINT ( 'NONE',  ( -33.91758640765102228, -278.8892612368916275, -193.8347554364740120 ) ) ;
#84241 = CARTESIAN_POINT ( 'NONE',  ( -111.8926394666918753, -268.1718929385297088, -295.4674195431252315 ) ) ;
#84242 = CARTESIAN_POINT ( 'NONE',  ( 23.33944059232405266, -277.1233348428481804, -317.3996648747249765 ) ) ;
#84243 = CARTESIAN_POINT ( 'NONE',  ( -30.56796663164417893, -299.5606560979661026, -193.9487378532710693 ) ) ;
#84244 = CARTESIAN_POINT ( 'NONE',  ( 39.58706461736021254, -284.0519495502703080, -270.3284710469133074 ) ) ;
#84245 = ORIENTED_EDGE ( 'NONE', *, *, #6444, .T. ) ;
#84246 = CARTESIAN_POINT ( 'NONE',  ( 155.8658096505380684, 20.95954935106544426, -14.18771993490441830 ) ) ;
#84247 = CARTESIAN_POINT ( 'NONE',  ( 35.26844308098985437, -288.7656935109196752, -280.5518043419718310 ) ) ;
#84248 = CARTESIAN_POINT ( 'NONE',  ( 29.48237270153248701, -289.7877105833223368, -306.6446534734146212 ) ) ;
#84249 = CARTESIAN_POINT ( 'NONE',  ( -109.2807042682991323, -289.7296501273459626, -283.3485100116148487 ) ) ;
#84250 = CARTESIAN_POINT ( 'NONE',  ( -87.70492119207074211, -284.8785635359379853, -212.1264027678606681 ) ) ;
#84251 = CARTESIAN_POINT ( 'NONE',  ( -38.48138622635112682, -140.2860406175970525, -364.7253011062631458 ) ) ;
#84252 = CARTESIAN_POINT ( 'NONE',  ( 35.01099711661705527, -280.1426295613439379, -284.9686179619862969 ) ) ;
#84253 = CARTESIAN_POINT ( 'NONE',  ( 10.93623958309508915, -290.2367336015209389, -326.8215340460706102 ) ) ;
#84254 = CARTESIAN_POINT ( 'NONE',  ( -95.67704250042621084, -282.4038054844089629, -315.4116642789221032 ) ) ;
#84255 = ADVANCED_FACE ( 'NONE', ( #39125 ), #8131, .T. ) ;
#84256 = CARTESIAN_POINT ( 'NONE',  ( -49.23812023226650325, -281.2125347697121924, -197.8372000961076935 ) ) ;
#84257 = CARTESIAN_POINT ( 'NONE',  ( -61.80452772538647821, -277.8710622567538735, -339.2593536484066021 ) ) ;
#84258 = CARTESIAN_POINT ( 'NONE',  ( -111.8799066240244429, -289.1243022832196061, -288.0826368843599994 ) ) ;
#84259 = CARTESIAN_POINT ( 'NONE',  ( -109.1483938591909464, -285.0063924531587531, -297.8581417460736702 ) ) ;
#84260 = CARTESIAN_POINT ( 'NONE',  ( -97.99203856796732737, -284.4114506142909136, -317.7009886062413671 ) ) ;
#84261 = CARTESIAN_POINT ( 'NONE',  ( -7.251538131411003008, -282.8128350608000687, -336.8848472271125161 ) ) ;
#84262 = ORIENTED_EDGE ( 'NONE', *, *, #7422, .T. ) ;
#84263 = DIRECTION ( 'NONE',  ( 1.000000000000000000, 0.000000000000000000, 0.000000000000000000 ) ) ;
#84264 = CARTESIAN_POINT ( 'NONE',  ( -76.55065144290706769, -293.3943204828004809, -205.4703344455697618 ) ) ;
#84265 = CARTESIAN_POINT ( 'NONE',  ( -95.27644711963867508, -289.9162994454585487, -220.3724753208754805 ) ) ;
#84266 = CARTESIAN_POINT ( 'NONE',  ( 23.99709799971681434, -274.0582521734554007, -230.3491161291757976 ) ) ;
#84267 = CARTESIAN_POINT ( 'NONE',  ( -84.12976630326390648, -295.0246793856765066, -331.4543991745005087 ) ) ;
#84268 = CARTESIAN_POINT ( 'NONE',  ( -98.86782811605233690, -289.5903964135389401, -229.7068626942543688 ) ) ;
#84269 = CARTESIAN_POINT ( 'NONE',  ( -53.39064865174962193, -293.5005271629672734, -342.6661994042524952 ) ) ;
#84270 = CARTESIAN_POINT ( 'NONE',  ( -109.8087082694134295, -291.6033783781911666, -282.0875244714740688 ) ) ;
#84271 = CARTESIAN_POINT ( 'NONE',  ( 208.6208076322478746, 32.98517505407394168, 13.08022668053247095 ) ) ;
#84272 = CARTESIAN_POINT ( 'NONE',  ( -109.9785144731161211, -292.3117252170790721, -289.0911257362126889 ) ) ;
#84273 = CARTESIAN_POINT ( 'NONE',  ( -33.60442121298309104, -290.0989374290365390, -195.2874130339217515 ) ) ;
#84274 = CARTESIAN_POINT ( 'NONE',  ( -58.64995643420090232, -297.3277305333636491, -342.3238007217727841 ) ) ;
#84275 = CARTESIAN_POINT ( 'NONE',  ( -10.67542976517641229, -287.3499294775880344, -202.1396432910799206 ) ) ;
#84276 = CARTESIAN_POINT ( 'NONE',  ( 37.00701095535362128, -295.6939918885259999, -281.4199419344276407 ) ) ;
#84277 = CARTESIAN_POINT ( 'NONE',  ( 37.50697896403737275, -277.6491198010464814, -279.5223611885564310 ) ) ;
#84278 = CARTESIAN_POINT ( 'NONE',  ( -70.64977880336589067, -296.8211718963902968, -201.1171239006658595 ) ) ;
#84279 = CARTESIAN_POINT ( 'NONE',  ( -35.10921939121834612, -275.2635925825913432, -344.3407776557868374 ) ) ;
#84280 = CARTESIAN_POINT ( 'NONE',  ( -92.34465615442489650, -277.3374061754516333, -220.2014825459703786 ) ) ;
#84281 = CARTESIAN_POINT ( 'NONE',  ( -108.9255479152700303, -273.9699580531637935, -254.1474434379779552 ) ) ;
#84282 = CARTESIAN_POINT ( 'NONE',  ( 29.44144410201021955, -273.6406558548493422, -233.1225251567176144 ) ) ;
#84283 = CARTESIAN_POINT ( 'NONE',  ( -99.21899739887237502, -297.4294650509331177, -310.2862679077778125 ) ) ;
#84284 = CARTESIAN_POINT ( 'NONE',  ( 152.4536156746142410, 249.5000000000000568, -12.00000000000000000 ) ) ;
#84285 = CARTESIAN_POINT ( 'NONE',  ( -108.3341153041739631, -297.5884285414779242, -252.6270757957564967 ) ) ;
#84286 = CARTESIAN_POINT ( 'NONE',  ( -113.5000000000000568, -192.7866584945343504, -447.4016117689005796 ) ) ;
#84288 = CARTESIAN_POINT ( 'NONE',  ( -60.51589897267113116, -297.7431833686640630, -201.0836897982399591 ) ) ;
#84287 = CARTESIAN_POINT ( 'NONE',  ( -88.39602578302967117, -287.7836040645354956, -325.7855046044128358 ) ) ;
#84289 = CARTESIAN_POINT ( 'NONE',  ( -30.88385360709938965, -286.1316094809763513, -193.6191048309662506 ) ) ;
#84290 = CARTESIAN_POINT ( 'NONE',  ( -74.42085929146699641, -289.1980951366976456, -337.8363800987611967 ) ) ;
#84291 = CARTESIAN_POINT ( 'NONE',  ( -111.7690686305628844, -298.6837421102805479, -258.4904968765356443 ) ) ;
#84292 = CARTESIAN_POINT ( 'NONE',  ( 7.132559714435090292, -292.4450679489729623, -330.6093050559271092 ) ) ;
#84293 = CARTESIAN_POINT ( 'NONE',  ( 26.15296653694375806, -280.1763454094890449, -226.9948738121624956 ) ) ;
#84294 = CARTESIAN_POINT ( 'NONE',  ( 39.58706461736020543, -291.0523547857347353, -270.3937649182068981 ) ) ;
#84295 = CARTESIAN_POINT ( 'NONE',  ( -103.3591830014524078, -276.0782298887147590, -306.0594822812865345 ) ) ;
#84296 = CARTESIAN_POINT ( 'NONE',  ( 194.7510731661265595, -163.7219104664116287, -22.50000000000000000 ) ) ;
#84297 = CARTESIAN_POINT ( 'NONE',  ( -84.95421151834061391, -288.5208364814200763, -326.2867783800795110 ) ) ;
#84298 = DIRECTION ( 'NONE',  ( 0.000000000000000000, 0.000000000000000000, 1.000000000000000000 ) ) ;
#84299 = CARTESIAN_POINT ( 'NONE',  ( -20.70994004439706160, -286.8384563345694573, -343.4937728102298706 ) ) ;
#84300 = CARTESIAN_POINT ( 'NONE',  ( -47.40174905920618897, -299.5224585793560550, -197.1982248599935303 ) ) ;
#84301 = CARTESIAN_POINT ( 'NONE',  ( 0.5917316778180724546, -283.9821162239069849, -336.7061761888923570 ) ) ;
#84303 = CARTESIAN_POINT ( 'NONE',  ( 34.56709077066861369, -281.3862695652334196, -257.7863101717085215 ) ) ;
#84302 = CARTESIAN_POINT ( 'NONE',  ( -110.4191644669191419, -270.8793731151073985, -250.9517806020308797 ) ) ;
#84304 = CARTESIAN_POINT ( 'NONE',  ( -66.05969493943618431, -275.0940551891459336, -202.6067698408761828 ) ) ;
#84305 = CARTESIAN_POINT ( 'NONE',  ( -22.97491304383034461, -282.2359772161225351, -196.6971608211119644 ) ) ;
#84306 = CARTESIAN_POINT ( 'NONE',  ( -79.01955879049030784, -272.3960262269687291, -209.9904073063051158 ) ) ;
#84307 = VERTEX_POINT ( 'NONE', #25404 ) ;
#84308 = CARTESIAN_POINT ( 'NONE',  ( 204.9104695348173095, 293.4474168480153367, -54.00000000001035971 ) ) ;
#84309 = CARTESIAN_POINT ( 'NONE',  ( -110.5887428641317030, -286.3465580144860496, -284.7387928971211863 ) ) ;
#84310 = DIRECTION ( 'NONE',  ( -0.000000000000000000, -0.000000000000000000, -1.000000000000000000 ) ) ;
#84311 = CARTESIAN_POINT ( 'NONE',  ( 13.79469577742117181, -279.9094976428775681, -334.5364918783848793 ) ) ;
#84312 = CARTESIAN_POINT ( 'NONE',  ( -113.6072760330506810, -277.6266566226042869, -280.1487678197534592 ) ) ;
#84313 = CARTESIAN_POINT ( 'NONE',  ( -111.8533543602551674, -289.1543620381488040, -254.3480278353933954 ) ) ;
#84314 = CARTESIAN_POINT ( 'NONE',  ( -45.69905321739354065, -284.6799852293620461, -343.6305057929895383 ) ) ;
#84315 = CARTESIAN_POINT ( 'NONE',  ( 34.67840892800860075, -277.3632515014755882, -286.5290304503243419 ) ) ;
#84316 = CARTESIAN_POINT ( 'NONE',  ( -76.44066801212321138, -284.9891923656160770, -336.0721096760068463 ) ) ;
#84317 = CARTESIAN_POINT ( 'NONE',  ( -108.1482501991677196, -283.0925459854659607, -289.7363837125326995 ) ) ;
#84318 = CARTESIAN_POINT ( 'NONE',  ( 26.83482368570765075, -283.0311184685040757, -231.4484905653811495 ) ) ;
#84319 = CARTESIAN_POINT ( 'NONE',  ( -44.04487388210681331, -274.1364358827622709, -193.6001342238260747 ) ) ;
#84320 = CARTESIAN_POINT ( 'NONE',  ( -35.71363750593609865, -276.8656109619170138, -347.3570280709755025 ) ) ;
#84321 = EDGE_CURVE ( 'NONE', #78294, #57275, #15110, .T. ) ;
#84322 = CARTESIAN_POINT ( 'NONE',  ( -98.34979951904632856, -297.8890285824146531, -313.0146759535410865 ) ) ;
#84323 = PLANE ( 'NONE',  #11241 ) ;
#84324 = PLANE ( 'NONE',  #40512 ) ;
#84325 = CARTESIAN_POINT ( 'NONE',  ( -113.1312661829077939, -294.6656637271667591, -272.4123263554637902 ) ) ;
#84326 = CARTESIAN_POINT ( 'NONE',  ( 22.33471725297932409, -274.4716980474815955, -228.1883773466636001 ) ) ;
#84327 = CARTESIAN_POINT ( 'NONE',  ( -102.3900012608572894, -274.2892154395384523, -229.9046322508898754 ) ) ;
#84328 = CARTESIAN_POINT ( 'NONE',  ( -11.69152912976776015, -288.1509467107841829, -200.9345903366583457 ) ) ;
#84329 = CARTESIAN_POINT ( 'NONE',  ( 38.81164438414817397, -295.1430409420499359, -275.9687372257406537 ) ) ;
#84330 = CARTESIAN_POINT ( 'NONE',  ( 38.45669660543479296, -294.6135550070981708, -258.9326703334056674 ) ) ;
#84331 = CARTESIAN_POINT ( 'NONE',  ( -110.2185687365378755, -292.7717898334248616, -253.3054367167377166 ) ) ;
#84332 = CARTESIAN_POINT ( 'NONE',  ( -103.7719087966673328, -277.0104159909346890, -235.7947370955506585 ) ) ;
#84333 = CARTESIAN_POINT ( 'NONE',  ( -111.7921871291635227, -280.5043544641291646, -267.8842725255389610 ) ) ;
#84334 = CARTESIAN_POINT ( 'NONE',  ( -102.7439189514116009, -294.1561601731656879, -305.9119825044945742 ) ) ;
#84335 = CARTESIAN_POINT ( 'NONE',  ( -52.64459181559339385, -285.1064613516277291, -344.6180137707083873 ) ) ;
#84336 = CARTESIAN_POINT ( 'NONE',  ( -109.2293978309542268, -283.6611915346845763, -255.9950122671550901 ) ) ;
#84337 = CARTESIAN_POINT ( 'NONE',  ( -61.61430774310042580, -183.8251665614383228, -361.5569093710298034 ) ) ;
#84338 = ORIENTED_EDGE ( 'NONE', *, *, #20108, .T. ) ;
#84339 = CARTESIAN_POINT ( 'NONE',  ( -46.72338182567795428, -285.5966199948400117, -197.8943661436944410 ) ) ;
#84340 = ORIENTED_EDGE ( 'NONE', *, *, #4248, .T. ) ;
#84341 = CARTESIAN_POINT ( 'NONE',  ( 19.56342512254201793, -283.3334309873904431, -321.8518551017077129 ) ) ;
#84342 = CARTESIAN_POINT ( 'NONE',  ( -85.32725245791327495, -273.7009403575781334, -215.2530619841450630 ) ) ;
#84343 = CARTESIAN_POINT ( 'NONE',  ( -46.44302071083694727, -284.7340151941835984, -194.3007821850058576 ) ) ;
#84344 = CARTESIAN_POINT ( 'NONE',  ( 36.37041645891896735, -282.2232715441088544, -248.8817054813272023 ) ) ;
#84345 = ADVANCED_FACE ( 'NONE', ( #4108 ), #90255, .F. ) ;
#84346 =( NAMED_UNIT ( * ) SI_UNIT ( $, .STERADIAN. ) SOLID_ANGLE_UNIT ( ) );
#84347 = CARTESIAN_POINT ( 'NONE',  ( -102.9992587898963734, -279.5599439612599326, -309.3464719749004530 ) ) ;
#84348 = CARTESIAN_POINT ( 'NONE',  ( -48.11272034212307602, -280.5700980686265780, -194.1673551957038626 ) ) ;
#84349 = CARTESIAN_POINT ( 'NONE',  ( -109.1418805571601069, -288.0523547857347353, -270.3284710469131937 ) ) ;
#84350 = CARTESIAN_POINT ( 'NONE',  ( 139.9169389161443746, 180.0772412164195089, -241.5140256757101724 ) ) ;
#84351 = ORIENTED_EDGE ( 'NONE', *, *, #75975, .T. ) ;
#84352 = CARTESIAN_POINT ( 'NONE',  ( -0.8503445863359465617, -276.5380006608442613, -205.0133822907053229 ) ) ;
#84353 = CARTESIAN_POINT ( 'NONE',  ( 84.07519268682317204, 83.49645322921298884, -302.1015330633007352 ) ) ;
#84354 = CARTESIAN_POINT ( 'NONE',  ( -109.1949021511918403, -276.8342382650922104, -250.0909398370305041 ) ) ;
#84355 = CARTESIAN_POINT ( 'NONE',  ( 5.900922189190457523, -294.3898997889865541, -207.8787234470421765 ) ) ;
#84356 = CARTESIAN_POINT ( 'NONE',  ( -101.5608122019473285, -295.4246967784312687, -305.2867291056866748 ) ) ;
#84357 = CARTESIAN_POINT ( 'NONE',  ( -50.54962184610741360, -291.3954542983861984, -194.5648271302828221 ) ) ;
#84359 = CARTESIAN_POINT ( 'NONE',  ( 16.58171999673249886, -286.6695730069550336, -320.8214340023699265 ) ) ;
#84358 = CARTESIAN_POINT ( 'NONE',  ( -76.79367488908245321, -294.1437925783213814, -335.8608054209029774 ) ) ;
#84360 = CARTESIAN_POINT ( 'NONE',  ( 36.43725941849402261, -295.5250492921121008, -279.0316752182571349 ) ) ;
#84361 = CARTESIAN_POINT ( 'NONE',  ( 26.11344774377200650, -286.7436832053563762, -307.5384696529426947 ) ) ;
#84362 = CARTESIAN_POINT ( 'NONE',  ( -110.3607346243348388, -285.7523831779633383, -279.1337361894713922 ) ) ;
#84363 = ORIENTED_EDGE ( 'NONE', *, *, #52765, .T. ) ;
#84364 = CARTESIAN_POINT ( 'NONE',  ( -107.0518029872466030, -291.9072968687473804, -238.0891048993933623 ) ) ;
#84365 = CARTESIAN_POINT ( 'NONE',  ( 15.87498493154905077, -282.7652357374507233, -320.4938084887062928 ) ) ;
#84366 = CARTESIAN_POINT ( 'NONE',  ( -97.10733412382995766, -294.7015391982949950, -318.2992873502142857 ) ) ;
#84367 = CARTESIAN_POINT ( 'NONE',  ( -113.6519345078848886, -291.2367556376891571, -279.7946161701090659 ) ) ;
#84368 = CARTESIAN_POINT ( 'NONE',  ( -114.1268187167687813, -291.1052671532131058, -265.5059695395955828 ) ) ;
#84369 = CARTESIAN_POINT ( 'NONE',  ( 29.42591672402162573, -288.1175250328088282, -300.0006963423217030 ) ) ;
#84370 = ORIENTED_EDGE ( 'NONE', *, *, #78108, .T. ) ;
#84371 = DIRECTION ( 'NONE',  ( 1.000000000000000000, 0.000000000000000000, 0.000000000000000000 ) ) ;
#84372 = CARTESIAN_POINT ( 'NONE',  ( -70.24960168051377707, -297.3414984183879710, -338.6203604525887272 ) ) ;
#84373 = CARTESIAN_POINT ( 'NONE',  ( -34.05635408497725791, -296.7773065497834750, -193.8549816543329314 ) ) ;
#84374 = ADVANCED_FACE ( 'NONE', ( #82697 ), #83153, .T. ) ;
#84375 = CARTESIAN_POINT ( 'NONE',  ( 26.67029487730599868, -280.1260193048545375, -234.7820097453027870 ) ) ;
#84376 = ORIENTED_EDGE ( 'NONE', *, *, #4626, .T. ) ;
#84377 = CARTESIAN_POINT ( 'NONE',  ( 23.58795260609568700, -274.4320967767723118, -223.3598426134718977 ) ) ;
#84378 = CARTESIAN_POINT ( 'NONE',  ( -55.44543573818710058, -296.2949690949762953, -198.8732915153567831 ) ) ;
#84379 = CARTESIAN_POINT ( 'NONE',  ( -79.31113783129632111, -279.4853316204519160, -331.6563028085305405 ) ) ;
#84380 = CARTESIAN_POINT ( 'NONE',  ( -40.80931946509393526, -272.1477909254060705, -196.1564042169583502 ) ) ;
#84381 = CARTESIAN_POINT ( 'NONE',  ( -93.37565050710217918, -297.0869188970864911, -317.7865627103959127 ) ) ;
#84382 = CARTESIAN_POINT ( 'NONE',  ( -37.83835201206461818, -299.1254603554876894, -197.0536871750575756 ) ) ;
#84383 = PLANE ( 'NONE',  #38155 ) ;
#84384 = CARTESIAN_POINT ( 'NONE',  ( -94.96305480293479206, -297.4715766353095319, -320.2231265894918124 ) ) ;
#84385 = CARTESIAN_POINT ( 'NONE',  ( -30.66177028539085114, -296.1354297406613227, -195.1967136867763770 ) ) ;
#84386 = CARTESIAN_POINT ( 'NONE',  ( 2.288803294583334758, -293.2495721843046681, -208.8738361416342002 ) ) ;
#84387 = CARTESIAN_POINT ( 'NONE',  ( -95.56958125686577432, -289.7553819729196789, -225.3623537982682024 ) ) ;
#84388 = CARTESIAN_POINT ( 'NONE',  ( 194.7510731661265595, -164.3527196417747689, -21.50000000000000000 ) ) ;
#84389 = CARTESIAN_POINT ( 'NONE',  ( 34.66195457170497463, -275.7012276121154173, -243.2502232539497413 ) ) ;
#84390 = CARTESIAN_POINT ( 'NONE',  ( -105.8271387144993838, -297.2248862334024011, -244.8808399273111434 ) ) ;
#84391 = CARTESIAN_POINT ( 'NONE',  ( -4.399904543953398139, -282.4639787289951300, -202.5734303699094596 ) ) ;
#84392 = CARTESIAN_POINT ( 'NONE',  ( 10.52758371878726606, -279.3820119313264740, -210.6121339448463345 ) ) ;
#84393 = ADVANCED_FACE ( 'NONE', ( #69435 ), #26387, .T. ) ;
#84394 = CARTESIAN_POINT ( 'NONE',  ( -102.0157615342755548, -277.3531132128244963, -312.0585213817184922 ) ) ;
#84395 = CARTESIAN_POINT ( 'NONE',  ( 24.26089512400363546, -281.2952303774416691, -309.9222180815027627 ) ) ;
#84396 = CARTESIAN_POINT ( 'NONE',  ( 35.22200958904141288, -279.2998677720605087, -250.7026428831857743 ) ) ;
#84397 = CARTESIAN_POINT ( 'NONE',  ( -19.10821555870619548, -272.8660219129529878, -199.0136997246420094 ) ) ;
#84398 = CARTESIAN_POINT ( 'NONE',  ( -101.8537144878484071, -281.0651545844107773, -232.0094727065487348 ) ) ;
#84399 = LINE ( 'NONE', #10106, #2009 ) ;
#84400 = DIRECTION ( 'NONE',  ( 0.000000000000000000, -0.000000000000000000, -1.000000000000000000 ) ) ;
#84401 = CARTESIAN_POINT ( 'NONE',  ( -75.25460777804273960, -295.7943235094953138, -204.4479841024782729 ) ) ;
#84402 = CARTESIAN_POINT ( 'NONE',  ( -73.43371414927439389, -291.5868802612986315, -202.3288195381723256 ) ) ;
#84403 = CARTESIAN_POINT ( 'NONE',  ( 37.87315669704598520, -277.5621275463726079, -271.1269236137998746 ) ) ;
#84404 = CARTESIAN_POINT ( 'NONE',  ( -54.64900273838330236, -271.8295515904222270, -197.3853828235882872 ) ) ;
#84405 = CARTESIAN_POINT ( 'NONE',  ( 201.2104617360081704, 60.19600395700749829, -7.000000000000000888 ) ) ;
#84406 = CARTESIAN_POINT ( 'NONE',  ( -95.15248760389202687, -285.8044239998201874, -319.0352866211200080 ) ) ;
#84407 = EDGE_LOOP ( 'NONE', ( #67837, #46957, #676, #4961 ) ) ;
#84408 = DIRECTION ( 'NONE',  ( 0.000000000000000000, 0.000000000000000000, 1.000000000000000000 ) ) ;
#84409 = CARTESIAN_POINT ( 'NONE',  ( 32.79333726643868374, -285.8988922467241878, -297.0768020882682094 ) ) ;
#84410 = FACE_OUTER_BOUND ( 'NONE', #91720, .T. ) ;
#84411 = CARTESIAN_POINT ( 'NONE',  ( 17.36634659898984623, -293.0434494363104250, -319.3102177360651126 ) ) ;
#84412 = CARTESIAN_POINT ( 'NONE',  ( 30.54519158094267794, -286.0907552523072468, -300.5257973592997018 ) ) ;
#84413 = CARTESIAN_POINT ( 'NONE',  ( -111.2639016180397959, -258.5489101121608542, -316.4159311957783984 ) ) ;
#84414 = CARTESIAN_POINT ( 'NONE',  ( -61.68578411627769498, -293.3681722875534774, -341.3553400149617119 ) ) ;
#84415 = CARTESIAN_POINT ( 'NONE',  ( -64.28411274121526731, -284.1867824856522589, -198.9551040473461399 ) ) ;
#84416 = CARTESIAN_POINT ( 'NONE',  ( -83.95867758776994094, -280.9998560703292583, -213.0822174579490138 ) ) ;
#84417 = CARTESIAN_POINT ( 'NONE',  ( 22.67118288217023192, -288.1166077668377739, -222.7328368943534826 ) ) ;
#84418 = CARTESIAN_POINT ( 'NONE',  ( 5.629903472503285933, -278.8654579711358110, -207.6920243571024969 ) ) ;
#84419 = CARTESIAN_POINT ( 'NONE',  ( -100.3039510493918698, -290.0436982626653162, -307.4032692991129920 ) ) ;
#84420 = CARTESIAN_POINT ( 'NONE',  ( -83.82386135046982645, -280.8250281173230292, -213.2444390358841417 ) ) ;
#84421 = CARTESIAN_POINT ( 'NONE',  ( 26.59500856852853801, -281.8698230888882676, -234.7985111099180244 ) ) ;
#84422 = CARTESIAN_POINT ( 'NONE',  ( -32.43915910271285696, -288.0935410092928919, -195.1526751699746853 ) ) ;
#84423 = ORIENTED_EDGE ( 'NONE', *, *, #57977, .F. ) ;
#84424 = CARTESIAN_POINT ( 'NONE',  ( -64.90008180760548839, -273.7019828982753324, -198.4474496965166850 ) ) ;
#84425 = CARTESIAN_POINT ( 'NONE',  ( -109.9444822227654726, -292.3083154189519064, -287.7013267156555116 ) ) ;
#84426 = CARTESIAN_POINT ( 'NONE',  ( 206.4403749041381388, 36.15246451355368862, 13.98713712351916172 ) ) ;
#84427 = CARTESIAN_POINT ( 'NONE',  ( 25.22466315766300227, -296.6948066931273047, -320.2154176792147382 ) ) ;
#84428 = ORIENTED_EDGE ( 'NONE', *, *, #11459, .T. ) ;
#84429 = CARTESIAN_POINT ( 'NONE',  ( -46.62862727319261325, -271.9343522624728848, -195.7703584392898506 ) ) ;
#84430 = CARTESIAN_POINT ( 'NONE',  ( 197.4657836131030706, 215.0000000000000568, -12.48225014817974987 ) ) ;
#84431 = CARTESIAN_POINT ( 'NONE',  ( -6.144064501548008650, -293.0488659797035211, -339.8819634091275930 ) ) ;
#84432 = CARTESIAN_POINT ( 'NONE',  ( -109.9861389561575606, -272.0083040098116385, -262.1954474380292481 ) ) ;
#84433 = CARTESIAN_POINT ( 'NONE',  ( -85.11996740817369300, -291.2455956538783539, -326.5350072438603775 ) ) ;
#84434 = CARTESIAN_POINT ( 'NONE',  ( -64.40532340248850574, -285.1704349223907684, -339.2489565985646891 ) ) ;
#84435 = CARTESIAN_POINT ( 'NONE',  ( -67.80218318753259155, -290.8694452443189107, -340.4379705508233656 ) ) ;
#84436 = CARTESIAN_POINT ( 'NONE',  ( -80.25009160482950676, -290.9348400447664176, -333.7667869390358533 ) ) ;
#84437 = CARTESIAN_POINT ( 'NONE',  ( 1.174480116851917000, -288.5661438619765704, -205.9460609092934362 ) ) ;
#84438 = CARTESIAN_POINT ( 'NONE',  ( 20.12727118129029336, -281.0238504726803512, -219.0936848592017725 ) ) ;
#84439 = CARTESIAN_POINT ( 'NONE',  ( -92.65236900269162845, -293.9167738930667042, -321.8587601983239210 ) ) ;
#84440 = CARTESIAN_POINT ( 'NONE',  ( -96.27168324184222570, -283.7179273768416579, -319.9421601307173546 ) ) ;
#84441 = CARTESIAN_POINT ( 'NONE',  ( 10.25926550139060112, -276.5769256824539184, -213.3287994548637698 ) ) ;
#84442 = CARTESIAN_POINT ( 'NONE',  ( -82.13390479932378696, -281.9090924074130839, -214.2458315076590907 ) ) ;
#84443 = CARTESIAN_POINT ( 'NONE',  ( 7.623145230536814587, -274.6881534806597642, -331.6809371522889478 ) ) ;
#84444 = CARTESIAN_POINT ( 'NONE',  ( 185.8264795993290193, 275.5000000000000568, 23.09031830825835385 ) ) ;
#84445 = CARTESIAN_POINT ( 'NONE',  ( 34.54487186711776303, -281.2327362140775904, -283.4814450499389409 ) ) ;
#84446 = CARTESIAN_POINT ( 'NONE',  ( -56.80823074348885626, -278.5026900084931754, -344.5040937399404015 ) ) ;
#84447 = CARTESIAN_POINT ( 'NONE',  ( -73.49157915535057839, -284.6436272365019136, -202.5821886492836654 ) ) ;
#84448 = CARTESIAN_POINT ( 'NONE',  ( 32.75359282100029645, -294.9990178746637639, -246.4399053763661414 ) ) ;
#84449 = CARTESIAN_POINT ( 'NONE',  ( -16.02093885647730787, -275.9233740138575968, -197.1499131875742989 ) ) ;
#84450 = CARTESIAN_POINT ( 'NONE',  ( -44.01653318996780939, -275.2847446179963526, -194.0930282987283135 ) ) ;
#84451 = DIRECTION ( 'NONE',  ( 0.6573509547581669610, 0.1665889405894028785, -0.7349407099568147084 ) ) ;
#84452 = CARTESIAN_POINT ( 'NONE',  ( -3.869357443563839816, -276.4309700254543714, -335.2348590473265517 ) ) ;
#84453 = CARTESIAN_POINT ( 'NONE',  ( -66.75074450077376298, -297.4385148179549674, -339.1734463673220148 ) ) ;
#84454 = CARTESIAN_POINT ( 'NONE',  ( -42.78263105986803083, -283.9831991596627745, -195.7128974807595512 ) ) ;
#84455 = CARTESIAN_POINT ( 'NONE',  ( -13.86886206668244625, -292.0151998331343179, -196.9923333276430242 ) ) ;
#84456 = CARTESIAN_POINT ( 'NONE',  ( 22.82150868883725536, -272.9668845987543477, -226.1770132627099485 ) ) ;
#84457 = CARTESIAN_POINT ( 'NONE',  ( 25.20682555546215653, -289.7344516070701275, -313.9732632313541103 ) ) ;
#84458 = CARTESIAN_POINT ( 'NONE',  ( 32.92932022341919662, -292.1951591364924070, -249.3004424128461380 ) ) ;
#84459 = EDGE_LOOP ( 'NONE', ( #62764, #22864, #92652, #67029 ) ) ;
#84460 = CARTESIAN_POINT ( 'NONE',  ( 17.08276957223457870, -291.3839738596577718, -216.6528036534279806 ) ) ;
#84461 = CARTESIAN_POINT ( 'NONE',  ( -96.57825259539474416, -289.6219187260157355, -313.0591078487359482 ) ) ;
#84462 = VERTEX_POINT ( 'NONE', #39581 ) ;
#84463 = CARTESIAN_POINT ( 'NONE',  ( 23.05257439262340569, -289.2663167028348425, -317.6477320227812129 ) ) ;
#84464 = CARTESIAN_POINT ( 'NONE',  ( -101.8736270309984633, -278.4200904000175001, -304.5330055055263756 ) ) ;
#84465 = CARTESIAN_POINT ( 'NONE',  ( -11.17565106643310813, -293.6394588670135022, -342.5065009999817676 ) ) ;
#84466 = CARTESIAN_POINT ( 'NONE',  ( -112.2622961920221627, -285.4205458410303322, -253.0343446932441509 ) ) ;
#84467 = EDGE_CURVE ( 'NONE', #19834, #13609, #85322, .T. ) ;
#84468 = CARTESIAN_POINT ( 'NONE',  ( -52.17336884950474030, -286.2006795055660859, -194.7702219466202678 ) ) ;
#84469 = CARTESIAN_POINT ( 'NONE',  ( -13.51845849879097727, -283.0675675113317311, -339.4403912660196170 ) ) ;
#84470 = CARTESIAN_POINT ( 'NONE',  ( 197.6044253294050463, 285.2818546706590723, -111.8431199949838799 ) ) ;
#84471 = CARTESIAN_POINT ( 'NONE',  ( -114.3334731447618964, -272.3709480647709711, -270.3588108202161493 ) ) ;
#84472 = CARTESIAN_POINT ( 'NONE',  ( -111.8583052612683559, -270.4238486108535540, -283.6505382273211922 ) ) ;
#84473 = CARTESIAN_POINT ( 'NONE',  ( 25.41959993401218654, -274.2321322206071272, -232.6648183996918249 ) ) ;
#84474 = CARTESIAN_POINT ( 'NONE',  ( 33.19152039684580302, -274.7360800206804470, -290.3892892549357612 ) ) ;
#84475 = CARTESIAN_POINT ( 'NONE',  ( -113.1443483155298111, -295.8911790799460846, -283.8337008503282277 ) ) ;
#84476 = CARTESIAN_POINT ( 'NONE',  ( -20.49356206675482994, -109.5565994813256907, -359.6110413397351522 ) ) ;
#84477 = CARTESIAN_POINT ( 'NONE',  ( 18.53154563780501718, -274.9544382816224015, -322.6246681904901266 ) ) ;
#84478 = CARTESIAN_POINT ( 'NONE',  ( 53.54104891564487900, -301.0620212793358519, -196.0967531908359263 ) ) ;
#84479 = VERTEX_POINT ( 'NONE', #48105 ) ;
#84480 = CARTESIAN_POINT ( 'NONE',  ( -91.47810984396089395, -298.2452671211477195, -215.9362215132393601 ) ) ;
#84481 =( BOUNDED_SURFACE ( )  B_SPLINE_SURFACE ( 3, 2, ( 
 ( #27396, #14604, #379 ),
 ( #58163, #70503, #78067 ),
 ( #22159, #20302, #13210 ),
 ( #34965, #92715, #63877 ),
 ( #20763, #49635, #31591 ),
 ( #38676, #87920, #52880 ) ),
 .UNSPECIFIED., .F., .F., .F. ) 
 B_SPLINE_SURFACE_WITH_KNOTS ( ( 4, 2, 4 ),
 ( 3, 3 ),
 ( 0.005169333131382347624, 0.006119585499877700299, 0.007069837868373052975 ),
 ( 0.000000000000000000, 0.5783792227927410101 ),
 .UNSPECIFIED. ) 
 GEOMETRIC_REPRESENTATION_ITEM ( )  RATIONAL_B_SPLINE_SURFACE ( (
 ( 1.000000000000000000, 0.8305966477414097326, 0.8571520539184362963),
 ( 1.000000000000000000, 0.8412850701494818395, 0.8661649758440579383),
 ( 1.000000000000000000, 0.8530303058598047716, 0.8760690466613954008),
 ( 1.000000000000000000, 0.8717109521664421212, 0.8918213438904722956),
 ( 1.000000000000000000, 0.8783573442016358035, 0.8974258578414773257),
 ( 1.000000000000000000, 0.8782019693812768146, 0.8972948393364408304) ) ) 
 REPRESENTATION_ITEM ( '' )  SURFACE ( )  );
#84482 = CARTESIAN_POINT ( 'NONE',  ( 33.76242309124552321, -288.2659274682625323, -287.1596924186707156 ) ) ;
#84483 = CARTESIAN_POINT ( 'NONE',  ( -34.84961870311571630, -295.8244189115176823, -347.1592192034344748 ) ) ;
#84484 = CARTESIAN_POINT ( 'NONE',  ( -103.7998126312026841, -297.5505082227326170, -231.4895506836044774 ) ) ;
#84485 = CARTESIAN_POINT ( 'NONE',  ( 32.34743403496987924, -294.0068588261889886, -292.0964483023908542 ) ) ;
#84486 = ORIENTED_EDGE ( 'NONE', *, *, #59496, .F. ) ;
#84487 =( BOUNDED_SURFACE ( )  B_SPLINE_SURFACE ( 3, 2, ( 
 ( #13405, #64081, #63612 ),
 ( #25708, #27600, #54590 ),
 ( #22346, #51218, #42718 ),
 ( #80108, #56970, #71635 ),
 ( #20958, #49826, #37470 ),
 ( #13864, #43202, #86268 ) ),
 .UNSPECIFIED., .F., .F., .F. ) 
 B_SPLINE_SURFACE_WITH_KNOTS ( ( 4, 2, 4 ),
 ( 3, 3 ),
 ( 0.006633574617387602568, 0.007266361004544705585, 0.007899147391701808602 ),
 ( 0.000000000000000000, 1.000000000000000000 ),
 .UNSPECIFIED. ) 
 GEOMETRIC_REPRESENTATION_ITEM ( )  RATIONAL_B_SPLINE_SURFACE ( (
 ( 1.000000000000000000, 0.8333723006562869795, 1.000000000000000000),
 ( 1.000000000000000000, 0.8265668121450767680, 1.000000000000000000),
 ( 1.000000000000000000, 0.8184438728316124623, 1.000000000000000000),
 ( 1.000000000000000000, 0.7999168228917755696, 1.000000000000000000),
 ( 1.000000000000000000, 0.7897639513982999127, 1.000000000000000000),
 ( 1.000000000000000000, 0.7791885400064296752, 1.000000000000000000) ) ) 
 REPRESENTATION_ITEM ( '' )  SURFACE ( )  );
#84488 = CARTESIAN_POINT ( 'NONE',  ( 37.49453677952599406, -277.3393367683453334, -259.9279093017450464 ) ) ;
#84489 = EDGE_CURVE ( 'NONE', #74347, #75846, #64210, .T. ) ;
#84490 = ADVANCED_FACE ( 'NONE', ( #11202 ), #67219, .T. ) ;
#84491 = ORIENTED_EDGE ( 'NONE', *, *, #75831, .F. ) ;
#84492 = CARTESIAN_POINT ( 'NONE',  ( 26.23330936383726808, -280.4867806933232828, -226.9351918812147346 ) ) ;
#84493 = CARTESIAN_POINT ( 'NONE',  ( -3.748893341467848028, -277.5387228653668785, -335.4374714524922183 ) ) ;
#84494 = CARTESIAN_POINT ( 'NONE',  ( 13.27257980712055918, -276.5082649256934815, -213.6148257675565958 ) ) ;
#84495 = CARTESIAN_POINT ( 'NONE',  ( -86.05162485144307993, -275.7431319580067566, -327.9250637786943230 ) ) ;
#84496 = CARTESIAN_POINT ( 'NONE',  ( -63.12317116106024173, -298.3588455627964322, -201.9028211954180563 ) ) ;
#84497 = CARTESIAN_POINT ( 'NONE',  ( -109.4658248454135787, -294.9348528856303915, -285.0350917772594244 ) ) ;
#84498 = CARTESIAN_POINT ( 'NONE',  ( 153.1687287787711114, 19.71439303875248683, -10.22517819557502605 ) ) ;
#84499 = CARTESIAN_POINT ( 'NONE',  ( -8.889701417104502568, -280.9068756044500788, -198.8767793298676168 ) ) ;
#84500 = CARTESIAN_POINT ( 'NONE',  ( -11.25205911331266506, -276.8691436503701198, -338.5397849996453488 ) ) ;
#84501 = CARTESIAN_POINT ( 'NONE',  ( 23.47965045459499223, -285.6139985952347615, -223.9277635034149512 ) ) ;
#84502 = CARTESIAN_POINT ( 'NONE',  ( -92.33917107632198906, -299.2684638623280193, -219.0474211882446127 ) ) ;
#84503 = DIRECTION ( 'NONE',  ( 0.000000000000000000, 0.000000000000000000, 1.000000000000000000 ) ) ;
#84504 = CARTESIAN_POINT ( 'NONE',  ( -5.731900617721290558, -287.8226513021683104, -336.3415870812905268 ) ) ;
#84505 = CARTESIAN_POINT ( 'NONE',  ( 3.278600209230730034, -278.8456605912011810, -208.4290573766685952 ) ) ;
#84507 = CARTESIAN_POINT ( 'NONE',  ( -100.2610150942315670, -282.0918041885346952, -310.2379879165210923 ) ) ;
#84506 = CARTESIAN_POINT ( 'NONE',  ( -19.37325337634339206, -278.8624451049915933, -198.9465788586520603 ) ) ;
#84508 = CARTESIAN_POINT ( 'NONE',  ( 5.473358113971913852, -288.6315135154992504, -208.7207170677915826 ) ) ;
#84509 = CARTESIAN_POINT ( 'NONE',  ( -93.40337145249286266, -280.4269895856880908, -222.9685858626709773 ) ) ;
#84510 = CARTESIAN_POINT ( 'NONE',  ( 153.3662540421047424, 20.33090216074013412, 12.12586741969728443 ) ) ;
#84511 = CARTESIAN_POINT ( 'NONE',  ( -28.12091379636063238, -294.1692172861027643, -195.8778125691332264 ) ) ;
#84512 = CARTESIAN_POINT ( 'NONE',  ( -67.32960535011552849, -275.6799215561296705, -340.1801666420981292 ) ) ;
#84513 = CARTESIAN_POINT ( 'NONE',  ( -18.98334697238140123, -277.4609261147664938, -341.1203119947492723 ) ) ;
#84514 = CARTESIAN_POINT ( 'NONE',  ( 17.79756720892234512, -282.8394078394411508, -219.2759966199120640 ) ) ;
#84515 = CARTESIAN_POINT ( 'NONE',  ( 145.2857639756989272, -299.5541904835127980, -195.3611179825600175 ) ) ;
#84516 = CARTESIAN_POINT ( 'NONE',  ( -43.04867894218896396, -291.0438270114022998, -345.7052922174098057 ) ) ;
#84517 = CARTESIAN_POINT ( 'NONE',  ( -23.10655727017623917, -292.8700466203845849, -344.0501218334949840 ) ) ;
#84518 = CARTESIAN_POINT ( 'NONE',  ( -83.17135601502684494, -284.6398509438687938, -208.6198081705028642 ) ) ;
#84519 = CARTESIAN_POINT ( 'NONE',  ( 201.2104617360081704, 60.19600395700749829, -9.000000000000000000 ) ) ;
#84520 = CARTESIAN_POINT ( 'NONE',  ( -79.12175298627666109, -272.1605615289080333, -209.8371671954822375 ) ) ;
#84521 = CARTESIAN_POINT ( 'NONE',  ( -34.79151669280420123, -290.2241130347376838, -196.1697300255089829 ) ) ;
#84522 = CARTESIAN_POINT ( 'NONE',  ( 208.4306832106270804, -198.2391364535880598, 0.000000000000000000 ) ) ;
#84523 = DIRECTION ( 'NONE',  ( 0.5831039236546639026, -0.7661730729848326149, -0.2701270746362063879 ) ) ;
#84524 = CARTESIAN_POINT ( 'NONE',  ( -41.99219267714649817, -290.4744182489737909, -194.1962922932764570 ) ) ;
#84525 = CARTESIAN_POINT ( 'NONE',  ( -23.94227290191253132, -284.4607735636431016, -195.5116938786316894 ) ) ;
#84526 = CARTESIAN_POINT ( 'NONE',  ( -110.8177567921373878, -286.0417802461519727, -265.4437703624051892 ) ) ;
#84527 = CARTESIAN_POINT ( 'NONE',  ( 2.526466785016224126, -287.4046897439871486, -209.0167539895106756 ) ) ;
#84528 = CARTESIAN_POINT ( 'NONE',  ( 14.29238269885748380, -294.7529144959206633, -215.4048136358007923 ) ) ;
#84529 = AXIS2_PLACEMENT_3D ( 'NONE', #19558, #41309, #25263 ) ;
#84530 = CARTESIAN_POINT ( 'NONE',  ( 29.26198385745171038, -274.1032667765052793, -306.1543468366396610 ) ) ;
#84531 = CARTESIAN_POINT ( 'NONE',  ( 38.19718175543830796, -275.7000407672019833, -255.5414818402107358 ) ) ;
#84532 = CARTESIAN_POINT ( 'NONE',  ( -2.693939750755892426, -290.5864108989727015, -203.1986668263294007 ) ) ;
#84533 = CARTESIAN_POINT ( 'NONE',  ( -95.90580814570735413, -279.2266411864729321, -220.3484144840087424 ) ) ;
#84534 = CARTESIAN_POINT ( 'NONE',  ( -109.5545231652896661, -298.2874343649134516, -289.3101322593834652 ) ) ;
#84535 = CARTESIAN_POINT ( 'NONE',  ( -48.18343439339132317, -253.0206516614774728, -472.6442049081569508 ) ) ;
#84536 = CARTESIAN_POINT ( 'NONE',  ( 113.5000000000000568, -218.8335761803644743, -447.4016117689005796 ) ) ;
#84537 = CARTESIAN_POINT ( 'NONE',  ( -96.96516594762569241, -283.8340900648736920, -227.3712274558124307 ) ) ;
#84538 = CARTESIAN_POINT ( 'NONE',  ( -97.80014055207578849, -277.1574277957417962, -225.9572756666332225 ) ) ;
#84539 = CARTESIAN_POINT ( 'NONE',  ( 222.4306832106270804, -135.2391364535880882, -22.50000000000000000 ) ) ;
#84540 = CARTESIAN_POINT ( 'NONE',  ( -18.70044056565021862, -272.7677251476854963, -196.3119100973368631 ) ) ;
#84541 = CARTESIAN_POINT ( 'NONE',  ( -40.51848743638214501, -276.4417018124065066, -343.4064736804778022 ) ) ;
#84542 = CARTESIAN_POINT ( 'NONE',  ( -10.21696186102800930, -296.2116682201667572, -338.8808693452598959 ) ) ;
#84543 = CARTESIAN_POINT ( 'NONE',  ( -3.780416096598072873, -279.4049107028315007, -201.3891861335980309 ) ) ;
#84544 = CARTESIAN_POINT ( 'NONE',  ( -12.91851203659506453, -295.6682028422287090, -339.4574100867980633 ) ) ;
#84545 = CARTESIAN_POINT ( 'NONE',  ( -105.5106409123517039, -297.4158461493966570, -305.2095094465364014 ) ) ;
#84546 = CARTESIAN_POINT ( 'NONE',  ( -98.44640764112762099, -296.9400876153848685, -230.3295074395100528 ) ) ;
#84547 = CARTESIAN_POINT ( 'NONE',  ( -80.70733034375930970, -293.4645102605961142, -209.1057582158795753 ) ) ;
#84548 = CARTESIAN_POINT ( 'NONE',  ( -67.19101861561325961, -285.8381280934745519, -199.3821197482443495 ) ) ;
#84549 = CARTESIAN_POINT ( 'NONE',  ( 37.51103972702107825, -273.5417016604889113, -258.5567114111759679 ) ) ;
#84550 = CARTESIAN_POINT ( 'NONE',  ( -68.05582737115803127, -289.2777502104871132, -340.9701994963284051 ) ) ;
#84551 = CARTESIAN_POINT ( 'NONE',  ( -21.87773377124138108, -282.2310454560187054, -197.2826716088150647 ) ) ;
#84552 = EDGE_CURVE ( 'NONE', #47807, #37341, #27519, .T. ) ;
#84553 = CARTESIAN_POINT ( 'NONE',  ( -17.09536289837461709, -285.3786407768920981, -199.9270325773222510 ) ) ;
#84554 = CARTESIAN_POINT ( 'NONE',  ( -72.47371337224363685, -289.5870430560574960, -204.0839309381270255 ) ) ;
#84555 = CARTESIAN_POINT ( 'NONE',  ( -87.71122462277782006, -229.8683413793775117, -344.1918058839762011 ) ) ;
#84556 = CARTESIAN_POINT ( 'NONE',  ( -8.224665675238146179, -285.9517117804990107, -203.3522622508393738 ) ) ;
#84557 = CARTESIAN_POINT ( 'NONE',  ( 154.3564990690576906, 19.12150670424914267, 10.40578999957047479 ) ) ;
#84558 = CARTESIAN_POINT ( 'NONE',  ( 34.37197863709827317, -282.8411621796157647, -297.7466705684454951 ) ) ;
#84559 = CARTESIAN_POINT ( 'NONE',  ( -111.7634962471925917, -289.8477185536031016, -251.4875653462070773 ) ) ;
#84560 = CARTESIAN_POINT ( 'NONE',  ( -40.99068555384094736, -281.6071083202118075, -194.2354764654441226 ) ) ;
#84561 = CARTESIAN_POINT ( 'NONE',  ( -108.1933901517096359, -279.4983224362807732, -299.2286826949339797 ) ) ;
#84562 = CARTESIAN_POINT ( 'NONE',  ( 32.73518496775560749, -281.1149334008352412, -249.9104412265337487 ) ) ;
#84563 = CARTESIAN_POINT ( 'NONE',  ( 36.12877936576951043, -277.7458007121079504, -285.4306002317723596 ) ) ;
#84564 = CARTESIAN_POINT ( 'NONE',  ( 22.28663472010287805, -294.2063025763596329, -319.1000031672770092 ) ) ;
#84565 = CARTESIAN_POINT ( 'NONE',  ( -78.13338405222577876, -289.5207895896929813, -207.8480367620082916 ) ) ;
#84566 = CARTESIAN_POINT ( 'NONE',  ( -109.5173458489569498, -271.5255873135467937, -256.7551377422548740 ) ) ;
#84567 = ORIENTED_EDGE ( 'NONE', *, *, #75724, .T. ) ;
#84568 = ORIENTED_EDGE ( 'NONE', *, *, #7722, .T. ) ;
#84569 = CARTESIAN_POINT ( 'NONE',  ( -111.0412837155565740, -286.6077944729850628, -259.8880297537694446 ) ) ;
#84570 = CARTESIAN_POINT ( 'NONE',  ( -102.7889931746739904, -295.7786440147611984, -302.8596403196340816 ) ) ;
#84571 = CARTESIAN_POINT ( 'NONE',  ( 24.55680202845721993, -294.0282434784202792, -225.0834420132484013 ) ) ;
#84572 = CARTESIAN_POINT ( 'NONE',  ( -18.70164910337568642, -283.4572461733512796, -341.0991058558648206 ) ) ;
#84573 = CARTESIAN_POINT ( 'NONE',  ( -24.18809762182304723, -273.2747913133352995, -194.6777368749933146 ) ) ;
#84574 = CARTESIAN_POINT ( 'NONE',  ( -113.0730773364861932, -291.3706731435830193, -257.0167823721474747 ) ) ;
#84575 = CARTESIAN_POINT ( 'NONE',  ( -46.33499748532583595, -284.0787806046485002, -195.1319608569893660 ) ) ;
#84576 = CARTESIAN_POINT ( 'NONE',  ( -44.89919570228643408, -292.2923718770568939, -193.7012355447725724 ) ) ;
#84577 = CARTESIAN_POINT ( 'NONE',  ( 35.70139722419138195, -287.8583545154607464, -268.3076320364752405 ) ) ;
#84578 = DIRECTION ( 'NONE',  ( -0.2156506209390900430, 0.000000000000000000, 0.9764705882352960886 ) ) ;
#84579 = CARTESIAN_POINT ( 'NONE',  ( 29.33919985515026596, -282.8906705383787994, 54.50000000000000711 ) ) ;
#84580 = CARTESIAN_POINT ( 'NONE',  ( 179.5473848012214262, 251.1466290182995351, -164.2343626752925729 ) ) ;
#84581 = CARTESIAN_POINT ( 'NONE',  ( 13.23584927058908534, -283.8805131436979536, -327.5683142627717075 ) ) ;
#84582 = CARTESIAN_POINT ( 'NONE',  ( -20.19161114001082069, -283.7666405000204009, -195.3683826091709363 ) ) ;
#84583 = ORIENTED_EDGE ( 'NONE', *, *, #57879, .F. ) ;
#84584 = CARTESIAN_POINT ( 'NONE',  ( 34.64037142633370081, -280.2892074466396366, -256.4094100199512241 ) ) ;
#84585 = CARTESIAN_POINT ( 'NONE',  ( -11.87718457728808374, -276.3963940815153251, -343.0620742489219879 ) ) ;
#84586 = CARTESIAN_POINT ( 'NONE',  ( -73.02580578515330956, -281.5781949007277944, -204.5836671965063545 ) ) ;
#84587 = CARTESIAN_POINT ( 'NONE',  ( 104.8979029556089984, 114.3573006684971176, -281.0218342242372387 ) ) ;
#84588 = CARTESIAN_POINT ( 'NONE',  ( 19.70100152600230103, -279.4321552419335717, -219.5011347623741642 ) ) ;
#84589 = CARTESIAN_POINT ( 'NONE',  ( -71.91821957149345224, -283.6127663966410637, -204.2074248991358445 ) ) ;
#84590 = CARTESIAN_POINT ( 'NONE',  ( -112.2015885280200393, -298.1433036508663577, -283.6952532771364872 ) ) ;
#84591 = CARTESIAN_POINT ( 'NONE',  ( 19.38961205466062054, -293.3934677931824808, -224.3027988332710834 ) ) ;
#84592 = ORIENTED_EDGE ( 'NONE', *, *, #65327, .T. ) ;
#84593 = CARTESIAN_POINT ( 'NONE',  ( -90.15917315633986107, -289.9705278726449365, -219.2577128042854895 ) ) ;
#84594 = CARTESIAN_POINT ( 'NONE',  ( -51.28598297934721728, -277.8773621177044220, -345.9843271319578548 ) ) ;
#84595 = CARTESIAN_POINT ( 'NONE',  ( -37.15174342076831238, -298.2212839986111703, -197.3582636486453339 ) ) ;
#84596 = ORIENTED_EDGE ( 'NONE', *, *, #40020, .T. ) ;
#84597 = CARTESIAN_POINT ( 'NONE',  ( -44.00215429290172153, -272.8902854639284214, -193.9069058675410702 ) ) ;
#84598 = CARTESIAN_POINT ( 'NONE',  ( 205.4738562182569694, 293.9636489450776367, -44.00000000000000000 ) ) ;
#84599 = CARTESIAN_POINT ( 'NONE',  ( 104.1964229570258311, -299.5541904835127980, -195.3611179825600175 ) ) ;
#84600 = VECTOR ( 'NONE', #15725, 1000.000000000000000 ) ;
#84601 = DIRECTION ( 'NONE',  ( -0.000000000000000000, -0.000000000000000000, -1.000000000000000000 ) ) ;
#84602 = CARTESIAN_POINT ( 'NONE',  ( -29.39754862652458201, -284.0289769777061792, -343.2892433025422179 ) ) ;
#84603 = CARTESIAN_POINT ( 'NONE',  ( -5.854689970467189752, -284.4039895035847962, -339.5170447559394802 ) ) ;
#84604 = CIRCLE ( 'NONE', #55904, 1.499999999999999556 ) ;
#84605 = CARTESIAN_POINT ( 'NONE',  ( -110.5441588553734249, -283.6397285687048679, -268.1682924790215452 ) ) ;
#84606 = CARTESIAN_POINT ( 'NONE',  ( -7.524701240498339772, -282.3076679480644202, -202.3633062496137143 ) ) ;
#84607 = CARTESIAN_POINT ( 'NONE',  ( 7.991815190154221149, -274.8999062043310460, -328.5258709774581689 ) ) ;
#84608 = CARTESIAN_POINT ( 'NONE',  ( 194.5881128153457098, -26.00396092263537540, -47.19625681453479871 ) ) ;
#84609 = CARTESIAN_POINT ( 'NONE',  ( 35.66308507941423755, -276.7194845221019364, -277.0340041590820874 ) ) ;
#84610 = DIRECTION ( 'NONE',  ( 0.000000000000000000, 0.000000000000000000, 1.000000000000000000 ) ) ;
#84611 = CARTESIAN_POINT ( 'NONE',  ( -96.92268435407343929, -278.7022862665535285, -318.9024891875315006 ) ) ;
#84612 = EDGE_CURVE ( 'NONE', #52994, #23580, #48574, .T. ) ;
#84613 = ORIENTED_EDGE ( 'NONE', *, *, #48, .F. ) ;
#84614 = EDGE_LOOP ( 'NONE', ( #42434, #27149, #70520, #47887 ) ) ;
#84615 = CARTESIAN_POINT ( 'NONE',  ( -46.38199491702875576, -287.7990128282820592, -195.1375940734226901 ) ) ;
#84616 = CARTESIAN_POINT ( 'NONE',  ( 10.38915617819067982, -293.5703017978193543, -325.8080933981307794 ) ) ;
#84617 = EDGE_CURVE ( 'NONE', #59201, #29874, #29034, .T. ) ;
#84618 = CARTESIAN_POINT ( 'NONE',  ( -48.86192889167434572, -288.5436588147713906, -346.4452298758017150 ) ) ;
#84619 = CARTESIAN_POINT ( 'NONE',  ( -88.37725866931455698, -283.5648368278256726, -216.7575194431497891 ) ) ;
#84621 = CARTESIAN_POINT ( 'NONE',  ( 4.164595750138585295, -286.7245440666101217, -331.7026040310582289 ) ) ;
#84620 = CARTESIAN_POINT ( 'NONE',  ( -107.5534399211838377, -282.8371188648794146, -292.3994144810747571 ) ) ;
#84622 = CARTESIAN_POINT ( 'NONE',  ( -92.84941488616658489, -285.0764923312933661, -318.4013188499606031 ) ) ;
#84623 = CARTESIAN_POINT ( 'NONE',  ( -6.140646871974609233, -274.6419973838914643, -338.5629869318368037 ) ) ;
#84624 = CARTESIAN_POINT ( 'NONE',  ( 21.48569449982180046, -285.2945054122856732, -221.9278849769301871 ) ) ;
#84625 = CARTESIAN_POINT ( 'NONE',  ( -111.4183016896326706, -298.7040071291575600, -258.5468238337924163 ) ) ;
#84626 = CARTESIAN_POINT ( 'NONE',  ( -24.08362996353298868, -284.2207929286254284, -196.3200007184363187 ) ) ;
#84627 = CARTESIAN_POINT ( 'NONE',  ( 13.48981789208581894, -281.7260268329336554, -217.5688768104170379 ) ) ;
#84628 = CARTESIAN_POINT ( 'NONE',  ( -6.358348707647138554, -290.6462704121202592, -338.8451333783993391 ) ) ;
#84629 = DIRECTION ( 'NONE',  ( 0.000000000000000000, -0.000000000000000000, -1.000000000000000000 ) ) ;
#84630 = DIRECTION ( 'NONE',  ( -1.000000000000000000, 0.000000000000000000, 0.000000000000000000 ) ) ;
#84631 = CARTESIAN_POINT ( 'NONE',  ( -6.365254188959164949, -296.5685791259637654, -339.2797221327722923 ) ) ;
#84632 = CARTESIAN_POINT ( 'NONE',  ( -84.68092123261685344, -277.4001464960598469, -212.1217702207200944 ) ) ;
#84633 = CARTESIAN_POINT ( 'NONE',  ( 21.19408760908437372, -292.0766276590422876, -220.5643083970942087 ) ) ;
#84634 = CARTESIAN_POINT ( 'NONE',  ( -61.29184687826233358, -293.7681399212100359, -340.2209503814428899 ) ) ;
#84635 = CARTESIAN_POINT ( 'NONE',  ( -81.57140323778570234, -278.1210370361632727, -211.6033012207521438 ) ) ;
#84636 = CARTESIAN_POINT ( 'NONE',  ( -108.5673262555312562, -270.9150424210555457, -248.5462471325402305 ) ) ;
#84637 = CARTESIAN_POINT ( 'NONE',  ( 22.98321295827224020, -294.2858875596326129, -228.3610005819590469 ) ) ;
#84638 = CARTESIAN_POINT ( 'NONE',  ( -110.4542110544635705, -298.8376638359844719, -287.0812184334320705 ) ) ;
#84639 = CARTESIAN_POINT ( 'NONE',  ( -105.8819918231437356, -295.4666606691158108, -236.8210499260000859 ) ) ;
#84640 = CARTESIAN_POINT ( 'NONE',  ( 36.77791863643169989, -291.5791904114416297, -253.5618488223141469 ) ) ;
#84641 = CARTESIAN_POINT ( 'NONE',  ( -91.01014542618868575, -291.2579636640669491, -320.7850197730614923 ) ) ;
#84642 = LINE ( 'NONE', #10810, #22975 ) ;
#84643 = CARTESIAN_POINT ( 'NONE',  ( -47.02593662354598791, -292.7288303693555349, -197.8434146943737062 ) ) ;
#84644 = CARTESIAN_POINT ( 'NONE',  ( 175.2296996224750103, 128.0000000000000568, 0.000000000000000000 ) ) ;
#84645 = CARTESIAN_POINT ( 'NONE',  ( -104.2705418291623687, -292.2427898216975564, -233.0980147010666030 ) ) ;
#84647 = CARTESIAN_POINT ( 'NONE',  ( 20.18289337632174352, -292.9184244090254765, -225.3973482517065179 ) ) ;
#84646 = CARTESIAN_POINT ( 'NONE',  ( 29.27970278240654523, -279.1063614056792517, -235.0362351616882108 ) ) ;
#84648 = CARTESIAN_POINT ( 'NONE',  ( -19.75622297167328512, -280.2720795538326115, -195.3413490507532799 ) ) ;
#84649 = CARTESIAN_POINT ( 'NONE',  ( -96.25687101198548135, -283.5513531797032556, -319.9269173938301947 ) ) ;
#84650 = CARTESIAN_POINT ( 'NONE',  ( -74.47631261130082692, -287.5470648378947089, -335.3454942629221023 ) ) ;
#84651 = CARTESIAN_POINT ( 'NONE',  ( -32.08142562831677935, -281.1246676961565072, -344.4097168422595132 ) ) ;
#84652 = CARTESIAN_POINT ( 'NONE',  ( -7.787486001178397288, -278.9123432563246752, -199.9959917526237803 ) ) ;
#84653 = CARTESIAN_POINT ( 'NONE',  ( -54.88051069804145499, -284.7520938587618389, -195.7026781873072707 ) ) ;
#84654 = CARTESIAN_POINT ( 'NONE',  ( 196.7035422149454291, 42.02664470600696944, 12.80665658919290628 ) ) ;
#84655 = CARTESIAN_POINT ( 'NONE',  ( -4.495127717372585430, -294.0924533125566995, -204.2596524295456391 ) ) ;
#84656 = CARTESIAN_POINT ( 'NONE',  ( 32.01057792079404152, -276.5624367077597299, -238.1592124264664676 ) ) ;
#84657 = CARTESIAN_POINT ( 'NONE',  ( -99.19526130156747001, -277.6819655194600500, -309.2656835814856322 ) ) ;
#84658 = CARTESIAN_POINT ( 'NONE',  ( -110.7812034713324039, -290.4260214670683808, -293.6791763000610445 ) ) ;
#84659 = CARTESIAN_POINT ( 'NONE',  ( 12.70830716631821389, -280.4407908647269778, -327.0373755569534069 ) ) ;
#84661 = CARTESIAN_POINT ( 'NONE',  ( 34.71683709249455774, -292.4380423093900276, -257.2155570980069115 ) ) ;
#84660 = AXIS2_PLACEMENT_3D ( 'NONE', #12854, #79110, #49281 ) ;
#84662 = CARTESIAN_POINT ( 'NONE',  ( -96.70741020440551949, -293.9239326537086754, -316.1946550473429056 ) ) ;
#84663 = EDGE_LOOP ( 'NONE', ( #75637, #55630, #3030, #89022 ) ) ;
#84664 = DIRECTION ( 'NONE',  ( -0.000000000000000000, -0.000000000000000000, -1.000000000000000000 ) ) ;
#84665 = CARTESIAN_POINT ( 'NONE',  ( -12.23317364619639847, -291.8953423973540566, -201.6956025926079974 ) ) ;
#84666 = CARTESIAN_POINT ( 'NONE',  ( 201.2104617360081704, 60.19600395700749829, 9.000000000000001776 ) ) ;
#84667 = AXIS2_PLACEMENT_3D ( 'NONE', #32678, #54434, #83306 ) ;
#84668 = CARTESIAN_POINT ( 'NONE',  ( -82.13390479932374433, -281.1952119285918457, -326.4764044574609443 ) ) ;
#84669 = CARTESIAN_POINT ( 'NONE',  ( -111.3918943636935808, -295.8673282966256011, -249.9314521311504791 ) ) ;
#84670 = CARTESIAN_POINT ( 'NONE',  ( 38.18235643354120867, -279.6150285160001658, -264.3260240273204431 ) ) ;
#84671 = EDGE_CURVE ( 'NONE', #17165, #46065, #45964, .T. ) ;
#84672 = ADVANCED_FACE ( 'NONE', ( #14838 ), #645, .T. ) ;
#84673 = CARTESIAN_POINT ( 'NONE',  ( -12.87735421558434545, -287.6787865930397743, -197.8711597050102853 ) ) ;
#84674 = CARTESIAN_POINT ( 'NONE',  ( 35.12395899986310610, -287.5017736918570677, -279.1774807049368405 ) ) ;
#84675 = CARTESIAN_POINT ( 'NONE',  ( -36.43843583764431315, -278.5607892142865012, -344.0615033695391958 ) ) ;
#84676 = CARTESIAN_POINT ( 'NONE',  ( -56.24362834746958129, -293.3168239188995585, -342.6266243905814122 ) ) ;
#84677 = CARTESIAN_POINT ( 'NONE',  ( -102.3467730436001801, -297.8358630124637898, -305.7491739687496874 ) ) ;
#84678 = CARTESIAN_POINT ( 'NONE',  ( -108.6719543624020901, -277.5740315345138356, -253.0658776848339073 ) ) ;
#84679 = VERTEX_POINT ( 'NONE', #58394 ) ;
#84680 = CARTESIAN_POINT ( 'NONE',  ( 194.2870706633419218, 39.56969527624839600, 14.58823529460389246 ) ) ;
#84681 = CARTESIAN_POINT ( 'NONE',  ( -110.7808982374902911, -295.9283464484436763, -293.4796578382243410 ) ) ;
#84682 = CARTESIAN_POINT ( 'NONE',  ( -109.7454457200876732, -292.2485869581113889, -287.6530763989714501 ) ) ;
#84683 = CARTESIAN_POINT ( 'NONE',  ( -47.80257052418233599, -229.5268262511776527, 25.50000000000000000 ) ) ;
#84684 = CARTESIAN_POINT ( 'NONE',  ( 33.18245165197373581, -288.4596492910171719, -289.7905777935097831 ) ) ;
#84685 = ORIENTED_EDGE ( 'NONE', *, *, #68972, .T. ) ;
#84686 = CARTESIAN_POINT ( 'NONE',  ( -40.98519899481389928, -279.0661385181588230, -193.6697707235305472 ) ) ;
#84687 = CARTESIAN_POINT ( 'NONE',  ( -104.5098224891832643, -296.7162949563278289, -307.9099859867413898 ) ) ;
#84688 = CARTESIAN_POINT ( 'NONE',  ( -112.8829774453177208, -288.6095878729155970, -276.8242574385814123 ) ) ;
#84689 = EDGE_CURVE ( 'NONE', #84890, #70200, #77475, .T. ) ;
#84690 = CARTESIAN_POINT ( 'NONE',  ( -110.7942305705971080, -297.1769013780221371, -247.1524508713619355 ) ) ;
#84691 = CARTESIAN_POINT ( 'NONE',  ( 33.66733163020020214, -293.6602690152835748, -253.2840564973251674 ) ) ;
#84692 = DIRECTION ( 'NONE',  ( -0.000000000000000000, -1.000000000000000000, -0.000000000000000000 ) ) ;
#84693 = DIRECTION ( 'NONE',  ( -0.000000000000000000, -0.000000000000000000, 1.000000000000000000 ) ) ;
#84694 = DIRECTION ( 'NONE',  ( -0.000000000000000000, -0.000000000000000000, -1.000000000000000000 ) ) ;
#84695 = CARTESIAN_POINT ( 'NONE',  ( 14.15025396002171831, -289.8650275804877197, -326.7469132408336918 ) ) ;
#84696 = CARTESIAN_POINT ( 'NONE',  ( -88.47809603358389552, -280.1948066931273615, -334.5364918783848793 ) ) ;
#84697 = EDGE_LOOP ( 'NONE', ( #17315, #41812, #9066, #42317 ) ) ;
#84698 = CARTESIAN_POINT ( 'NONE',  ( 20.99419836792590388, -280.2234051625807183, -220.2388400288934918 ) ) ;
#84699 = CARTESIAN_POINT ( 'NONE',  ( -63.22018972664060499, -287.7145853112636473, -200.0895239626313469 ) ) ;
#84700 = CARTESIAN_POINT ( 'NONE',  ( 24.23925055052949773, -285.5213923579242987, -225.1240446071109602 ) ) ;
#84701 = CARTESIAN_POINT ( 'NONE',  ( -93.37441368050792789, -271.2433656057248754, -220.7590672161392717 ) ) ;
#84702 = CARTESIAN_POINT ( 'NONE',  ( -46.37734614304641667, -275.8567679110998370, -196.4715294218481461 ) ) ;
#84703 = CARTESIAN_POINT ( 'NONE',  ( -83.45712644497612587, -287.7699418104172651, -328.7963954310883423 ) ) ;
#84704 = CARTESIAN_POINT ( 'NONE',  ( -112.4950573596744334, -280.5397487875893603, -260.3548702983563885 ) ) ;
#84705 = ORIENTED_EDGE ( 'NONE', *, *, #40483, .F. ) ;
#84707 = CARTESIAN_POINT ( 'NONE',  ( 34.16664434493925029, -280.7000024331819645, -255.1208841223880484 ) ) ;
#84706 = CARTESIAN_POINT ( 'NONE',  ( -81.28787849535682142, -279.4359994262300120, -212.0075647879850465 ) ) ;
#84708 = CARTESIAN_POINT ( 'NONE',  ( 16.74700613502275104, -277.3841904788619672, -324.8035154789374133 ) ) ;
#84709 = CARTESIAN_POINT ( 'NONE',  ( -111.3434381929979082, -277.5967651603709214, -250.5178024289012058 ) ) ;
#84710 = CARTESIAN_POINT ( 'NONE',  ( -23.38302767679204308, -107.9165556172637537, -359.8680264726103246 ) ) ;
#84711 = CARTESIAN_POINT ( 'NONE',  ( -112.2164470930137981, -273.7057689388974495, -253.4320754468055839 ) ) ;
#84712 = CARTESIAN_POINT ( 'NONE',  ( -112.3900044434635817, -274.2499993953724129, -256.2779135276613829 ) ) ;
#84713 = CARTESIAN_POINT ( 'NONE',  ( -95.95921662488163406, -286.4090924074130839, -317.1477375740089997 ) ) ;
#84714 = DIRECTION ( 'NONE',  ( 0.7806247497998081153, 0.000000000000000000, 0.6249999999999895639 ) ) ;
#84715 = CARTESIAN_POINT ( 'NONE',  ( 34.31574213812709218, -288.8358157354460900, -285.8937989022575152 ) ) ;
#84716 = CARTESIAN_POINT ( 'NONE',  ( 27.81790765058295634, -288.7944951500990101, -231.1674942962002604 ) ) ;
#84717 = CARTESIAN_POINT ( 'NONE',  ( -108.4515006946262616, -289.6774359606176290, -287.3107177402468437 ) ) ;
#84718 = CARTESIAN_POINT ( 'NONE',  ( -83.85099562316381139, -283.1789729676905267, -331.7176246685296519 ) ) ;
#84719 = CARTESIAN_POINT ( 'NONE',  ( -57.31031176507513436, -278.1899923617590957, -199.3139860024720633 ) ) ;
#84720 = CARTESIAN_POINT ( 'NONE',  ( -86.56256127943112233, -287.2205351154871096, -214.7210659250795288 ) ) ;
#84721 = CARTESIAN_POINT ( 'NONE',  ( 36.38145335926363089, -280.0088260779004372, -268.5860096695554375 ) ) ;
#84722 = CARTESIAN_POINT ( 'NONE',  ( -74.77127618962455813, -280.8582199984024896, -207.0549270406785354 ) ) ;
#84723 = CARTESIAN_POINT ( 'NONE',  ( -1.434521781129437512, -277.0549926395453326, -334.0474746989127084 ) ) ;
#84724 = CARTESIAN_POINT ( 'NONE',  ( 28.55431942628628761, -286.8586337448199970, -309.4216264878447191 ) ) ;
#84725 = CARTESIAN_POINT ( 'NONE',  ( -10.74830540271383228, -283.5169672535341761, -342.5075242484209070 ) ) ;
#84726 = CARTESIAN_POINT ( 'NONE',  ( -95.28425453745306584, -284.3593478299513890, -320.9791710059241723 ) ) ;
#84727 = CARTESIAN_POINT ( 'NONE',  ( -16.13047405776010024, -282.9367921103295203, -340.2115574449022120 ) ) ;
#84728 = ORIENTED_EDGE ( 'NONE', *, *, #65538, .F. ) ;
#84729 = DIRECTION ( 'NONE',  ( -1.000000000000000000, 0.000000000000000000, 0.000000000000000000 ) ) ;
#84730 = CARTESIAN_POINT ( 'NONE',  ( -106.1487629417414098, -292.8263129146864117, -238.5202094795858443 ) ) ;
#84731 = CARTESIAN_POINT ( 'NONE',  ( -22.27441263933424409, -290.9259218194210348, -195.2986374772053466 ) ) ;
#84732 = CARTESIAN_POINT ( 'NONE',  ( -11.39567996390432292, -273.4572536321517759, -201.8217678506137531 ) ) ;
#84733 = CARTESIAN_POINT ( 'NONE',  ( 19.44879114161051703, -293.6072841746498057, -322.2860680568882685 ) ) ;
#84734 = VECTOR ( 'NONE', #71909, 1000.000000000000000 ) ;
#84735 = CARTESIAN_POINT ( 'NONE',  ( -105.7639325553857645, -288.6675410030409807, -297.8679640479024897 ) ) ;
#84736 = CARTESIAN_POINT ( 'NONE',  ( 34.94427830642977995, -291.5844112301731457, -254.4055386044406646 ) ) ;
#84737 = CARTESIAN_POINT ( 'NONE',  ( -109.3251579806793075, -291.5682997801242209, -284.7610372288885401 ) ) ;
#84738 = CARTESIAN_POINT ( 'NONE',  ( 150.6539576904058606, 293.9636489450775230, -9.103929867429224387 ) ) ;
#84739 = CARTESIAN_POINT ( 'NONE',  ( -109.6078751263233784, -292.2942188588540375, -290.4260276988350711 ) ) ;
#84740 = CARTESIAN_POINT ( 'NONE',  ( 30.54150309095506799, -291.1267789772827541, -237.9616072299320138 ) ) ;
#84741 = AXIS2_PLACEMENT_3D ( 'NONE', #41810, #20532, #4902 ) ;
#84742 = CARTESIAN_POINT ( 'NONE',  ( 36.88765235938980425, -295.6911480231632368, -281.1738630368813574 ) ) ;
#84743 = CARTESIAN_POINT ( 'NONE',  ( -33.23741947741860514, -287.0462135641232067, -197.1909391565655199 ) ) ;
#84744 = CARTESIAN_POINT ( 'NONE',  ( 26.56108238362537932, -296.0836441875538299, -310.0375213366009461 ) ) ;
#84745 = CARTESIAN_POINT ( 'NONE',  ( 34.16107026347832232, -277.2241827566902543, -246.4110790618088629 ) ) ;
#84746 = CARTESIAN_POINT ( 'NONE',  ( -99.78435095805376420, -296.3439619059403185, -225.5830633345405545 ) ) ;
#84747 = CARTESIAN_POINT ( 'NONE',  ( 36.10887726020285982, -273.9158375105640175, -279.8785685496325186 ) ) ;
#84748 = CARTESIAN_POINT ( 'NONE',  ( -54.80738866751382687, -277.9058833096234480, -197.9458621699358787 ) ) ;
#84749 = CARTESIAN_POINT ( 'NONE',  ( -92.32574634542643821, -274.4480840224735516, -221.7413157714183569 ) ) ;
#84750 = CARTESIAN_POINT ( 'NONE',  ( -110.3230004952766166, -298.1060029764889237, -260.5359188559763766 ) ) ;
#84751 = CARTESIAN_POINT ( 'NONE',  ( 198.7962788613918690, 70.38469146216345962, 8.627472241157438049 ) ) ;
#84752 = CARTESIAN_POINT ( 'NONE',  ( -77.60936398729224095, -298.2995312104695813, -209.2173654003723016 ) ) ;
#84753 = CARTESIAN_POINT ( 'NONE',  ( 169.2744399300530347, -11.64849832608277325, 10.00000000000000000 ) ) ;
#84755 = CARTESIAN_POINT ( 'NONE',  ( 94.40996231196450594, -299.7467194292196382, -197.3612517501071864 ) ) ;
#84754 = CARTESIAN_POINT ( 'NONE',  ( 31.22608769093933745, -285.1625677516429960, -238.9805696521124503 ) ) ;
#84756 = CARTESIAN_POINT ( 'NONE',  ( -36.56543202773214318, -286.0616424611802131, -193.3519920686951536 ) ) ;
#84757 = CARTESIAN_POINT ( 'NONE',  ( -103.7823230088408479, -289.7115626355816289, -309.3431339259833521 ) ) ;
#84758 = CARTESIAN_POINT ( 'NONE',  ( -94.34380924369031618, -299.2129856554471417, -220.9966340517623564 ) ) ;
#84759 = CARTESIAN_POINT ( 'NONE',  ( -2.307449892412390735, -292.5872080995020497, -336.4869808458252578 ) ) ;
#84760 = CARTESIAN_POINT ( 'NONE',  ( 22.75543048566671800, -280.1067417238356256, -222.4602033218193924 ) ) ;
#84761 = CARTESIAN_POINT ( 'NONE',  ( -54.49178911615187815, -292.7666405000204577, -345.3538533559490702 ) ) ;
#84762 = CARTESIAN_POINT ( 'NONE',  ( -112.2682631038234575, -276.6075373647698825, -266.0347761404772200 ) ) ;
#84763 = CARTESIAN_POINT ( 'NONE',  ( -0.8070456546349069615, -287.3506722593737095, -334.0776805057863044 ) ) ;
#84764 = CARTESIAN_POINT ( 'NONE',  ( 222.4306832106270804, -135.2391364535880882, 21.50000000000000000 ) ) ;
#84765 = CARTESIAN_POINT ( 'NONE',  ( -10.01859092377965865, -286.6953941853980155, -340.2627007679978988 ) ) ;
#84766 = CARTESIAN_POINT ( 'NONE',  ( -108.6156099153904933, -274.3195619663922002, -251.4372613403305650 ) ) ;
#84767 = CARTESIAN_POINT ( 'NONE',  ( 4.240385071979641651, -283.9290616604112643, -334.5293289439453019 ) ) ;
#84769 = CARTESIAN_POINT ( 'NONE',  ( 31.35459803861290240, -281.8828075987588022, -295.2050829412053758 ) ) ;
#84768 = CARTESIAN_POINT ( 'NONE',  ( -32.02832856230393332, -296.1384645152230064, -195.0076918465410643 ) ) ;
#84770 = CARTESIAN_POINT ( 'NONE',  ( -105.9567382910251041, -296.2675369939992720, -305.4210399779860268 ) ) ;
#84771 = CARTESIAN_POINT ( 'NONE',  ( -93.37414077111203881, -274.6506805554784592, -222.6369382647161217 ) ) ;
#84772 = CARTESIAN_POINT ( 'NONE',  ( 37.92269054352076552, -285.5397119971207758, -263.1200446917670774 ) ) ;
#84773 = CARTESIAN_POINT ( 'NONE',  ( 33.43170347536704412, -283.2290831294160398, -245.3842730494966702 ) ) ;
#84774 = CARTESIAN_POINT ( 'NONE',  ( -33.78576006705885248, -297.1564869643439124, -197.1264078654978107 ) ) ;
#84775 = ORIENTED_EDGE ( 'NONE', *, *, #12020, .F. ) ;
#84776 = DIRECTION ( 'NONE',  ( -0.7666168903225496489, 0.000000000000000000, 0.6421047760857910847 ) ) ;
#84777 = CARTESIAN_POINT ( 'NONE',  ( -111.8721599483374689, -286.5963108412518636, -265.3800139427193585 ) ) ;
#84778 = CARTESIAN_POINT ( 'NONE',  ( 180.7287904564219332, 249.5000000000000568, -24.90000000000002345 ) ) ;
#84779 = CARTESIAN_POINT ( 'NONE',  ( 13.84574458161073807, -278.1952119285919025, -206.2264541496106460 ) ) ;
#84780 = CARTESIAN_POINT ( 'NONE',  ( 37.43235747293748261, -274.9717021062375579, -288.1095405543710513 ) ) ;
#84781 = EDGE_CURVE ( 'NONE', #68679, #81769, #18821, .T. ) ;
#84782 = EDGE_CURVE ( 'NONE', #14615, #37664, #74714, .T. ) ;
#84783 = CARTESIAN_POINT ( 'NONE',  ( -99.60657900625787420, -285.5315257133872819, -309.8747869485899287 ) ) ;
#84784 = CARTESIAN_POINT ( 'NONE',  ( 1.307565994427088985, -278.1271181248552580, -333.2914747882579718 ) ) ;
#84785 = CARTESIAN_POINT ( 'NONE',  ( -111.1567905624018096, -286.2288391469839439, -250.4152047535799284 ) ) ;
#84786 = CARTESIAN_POINT ( 'NONE',  ( -24.00833709386140313, -281.6729526445915326, -342.5369583582279347 ) ) ;
#84787 = CARTESIAN_POINT ( 'NONE',  ( -4.710738447983236377, -282.4821269235096111, -202.8317096219167013 ) ) ;
#84788 = CARTESIAN_POINT ( 'NONE',  ( -64.90206425053058581, -273.8686360474692378, -198.4482093745783686 ) ) ;
#84789 = CARTESIAN_POINT ( 'NONE',  ( 14.88162004000146688, -276.1737655366200102, -327.0174710811662635 ) ) ;
#84790 = CARTESIAN_POINT ( 'NONE',  ( -25.96364965714505857, -296.8262925768906939, -343.9264234137226595 ) ) ;
#84791 = CARTESIAN_POINT ( 'NONE',  ( 154.1407330040854333, 275.5000000000000568, 13.42592592592592915 ) ) ;
#84792 = CYLINDRICAL_SURFACE ( 'NONE', #85898, 1.000000000000000888 ) ;
#84793 = CARTESIAN_POINT ( 'NONE',  ( -108.2893624237504469, -294.3482952930792749, -297.0937443386634413 ) ) ;
#84794 = CARTESIAN_POINT ( 'NONE',  ( -9.971123134216737682, -276.1925234148372397, -338.1156714925178903 ) ) ;
#84795 = CIRCLE ( 'NONE', #28872, 4.999999999999997335 ) ;
#84796 = CARTESIAN_POINT ( 'NONE',  ( -55.01980313128539990, -287.5820087059923935, -198.4369648561895758 ) ) ;
#84797 = CARTESIAN_POINT ( 'NONE',  ( 37.92563509238276964, -295.2316685289459315, -282.9917432509762421 ) ) ;
#84798 = CARTESIAN_POINT ( 'NONE',  ( 39.25836179704051432, -294.7204588572359398, -267.4363748337179345 ) ) ;
#84799 = CARTESIAN_POINT ( 'NONE',  ( -109.5269139884052834, -292.8066095119255010, -250.6298400540872819 ) ) ;
#84800 = CARTESIAN_POINT ( 'NONE',  ( -77.79194998776431191, -277.5077983818829921, -207.3405966366347855 ) ) ;
#84801 = CARTESIAN_POINT ( 'NONE',  ( -93.30690106862569166, -281.1594645595143902, -221.2580104515446919 ) ) ;
#84802 = CARTESIAN_POINT ( 'NONE',  ( -39.75983852277892083, -293.1625717972547704, -344.7745111140371250 ) ) ;
#84803 = CARTESIAN_POINT ( 'NONE',  ( -80.83282669348670879, -285.4954627753491536, -332.4638488983590605 ) ) ;
#84804 = CARTESIAN_POINT ( 'NONE',  ( -98.35675271117310103, -284.0342402880223176, -229.7238268332223470 ) ) ;
#84805 = CARTESIAN_POINT ( 'NONE',  ( 195.6780093180179563, 277.3413982316666875, -125.4371938877353898 ) ) ;
#84806 = ORIENTED_EDGE ( 'NONE', *, *, #11577, .T. ) ;
#84807 = CARTESIAN_POINT ( 'NONE',  ( -108.7416330140586638, -284.0162923708891185, -285.7220592454714847 ) ) ;
#84808 = ORIENTED_EDGE ( 'NONE', *, *, #22107, .F. ) ;
#84809 = CARTESIAN_POINT ( 'NONE',  ( 15.55032856930039742, -283.4044780371802972, -325.8942235091454904 ) ) ;
#84810 = CARTESIAN_POINT ( 'NONE',  ( -91.61080955759018707, -284.0945860664872953, -216.2975213594836816 ) ) ;
#84811 = CARTESIAN_POINT ( 'NONE',  ( -77.38005555113339540, -280.4706140308082354, -204.8033902624935365 ) ) ;
#84812 = CARTESIAN_POINT ( 'NONE',  ( -37.10946225639649754, -278.5693742099411452, -346.6803751457239855 ) ) ;
#84813 = CARTESIAN_POINT ( 'NONE',  ( -68.63864484960069490, -280.3029480464213066, -200.1056368983956304 ) ) ;
#84814 = CARTESIAN_POINT ( 'NONE',  ( -37.30987171927208834, -271.5523547857346784, -200.3611179825600459 ) ) ;
#84815 = CARTESIAN_POINT ( 'NONE',  ( -70.18950016389896973, -196.7549604899246560, -360.5100559345433453 ) ) ;
#84816 = ORIENTED_EDGE ( 'NONE', *, *, #83604, .T. ) ;
#84817 = CARTESIAN_POINT ( 'NONE',  ( -35.36684806826554706, -276.0771255001219515, -195.5410233525968522 ) ) ;
#84818 = CARTESIAN_POINT ( 'NONE',  ( -22.85399180902964744, -107.9061763485807575, -362.3883434141006319 ) ) ;
#84819 = CARTESIAN_POINT ( 'NONE',  ( -38.35132707659149531, -278.0595478403196807, -195.7104624054299222 ) ) ;
#84820 = CARTESIAN_POINT ( 'NONE',  ( 3.576728897784181793, -294.3541604621228771, -206.2702029395413774 ) ) ;
#84821 = CARTESIAN_POINT ( 'NONE',  ( -106.0858749912648165, -295.5682328616630912, -295.3722504882852604 ) ) ;
#84822 = CARTESIAN_POINT ( 'NONE',  ( -114.3071169708805002, -290.0849770803972092, -268.3500589904878666 ) ) ;
#84823 = DIRECTION ( 'NONE',  ( 0.000000000000000000, 0.000000000000000000, 1.000000000000000000 ) ) ;
#84825 = CARTESIAN_POINT ( 'NONE',  ( -7.917463025506221719, -284.8441096491782218, -202.6805839453087685 ) ) ;
#84824 = CARTESIAN_POINT ( 'NONE',  ( -65.40412269765339204, -293.9866170260205536, -341.4463711949826461 ) ) ;
#84826 = CARTESIAN_POINT ( 'NONE',  ( -22.51672697835618564, -294.1043819849616625, -197.6212688720690096 ) ) ;
#84827 = CARTESIAN_POINT ( 'NONE',  ( -6.710822767611735351, -284.9416101420918608, -203.3214644756497762 ) ) ;
#84828 = CARTESIAN_POINT ( 'NONE',  ( -110.8110360097829954, -285.8238852202031808, -273.6769757991029337 ) ) ;
#84829 = ORIENTED_EDGE ( 'NONE', *, *, #80305, .F. ) ;
#84830 = CARTESIAN_POINT ( 'NONE',  ( -110.2113524460009444, -291.8000903049033923, -246.0527354650368750 ) ) ;
#84831 = CARTESIAN_POINT ( 'NONE',  ( -40.23052004740426923, -283.5817903235462154, -343.3655230638606781 ) ) ;
#84832 = CARTESIAN_POINT ( 'NONE',  ( -90.44791490317665250, -294.5786128598911091, -325.6404907111116245 ) ) ;
#84833 = CARTESIAN_POINT ( 'NONE',  ( -112.1031967444912425, -291.1318852902273875, -288.1621713047666731 ) ) ;
#84834 = CARTESIAN_POINT ( 'NONE',  ( -113.7516712763731590, -290.9263203072271722, -279.8029483380072406 ) ) ;
#84835 = CARTESIAN_POINT ( 'NONE',  ( 33.70157724005862576, -287.9403130411283200, -287.1495885898339111 ) ) ;
#84836 = ORIENTED_EDGE ( 'NONE', *, *, #50049, .F. ) ;
#84837 = CARTESIAN_POINT ( 'NONE',  ( 139.6925840978351516, -141.7221692137691775, 22.50000000000000000 ) ) ;
#84838 = CARTESIAN_POINT ( 'NONE',  ( -55.74692182794782269, -297.1470581060739278, -343.8563783195525048 ) ) ;
#84839 = CARTESIAN_POINT ( 'NONE',  ( -67.96458247795152374, -296.3434408782087530, -200.1937976084643367 ) ) ;
#84840 = CARTESIAN_POINT ( 'NONE',  ( -74.61525198448114793, -278.6021579599489542, -207.2624438366001698 ) ) ;
#84841 = ORIENTED_EDGE ( 'NONE', *, *, #72825, .F. ) ;
#84842 = CARTESIAN_POINT ( 'NONE',  ( 39.07569942218166403, -275.1772789667185179, -279.7466177749163307 ) ) ;
#84843 = CARTESIAN_POINT ( 'NONE',  ( -75.55375752995296068, -296.0126425416032134, -207.2896907608808590 ) ) ;
#84844 = CARTESIAN_POINT ( 'NONE',  ( 12.59584276663795066, -278.2080731425076010, -325.3590930503311824 ) ) ;
#84845 = CARTESIAN_POINT ( 'NONE',  ( -2.310188958453692987, -272.6605247745145562, -204.9114525339362274 ) ) ;
#84846 = CARTESIAN_POINT ( 'NONE',  ( -41.04398173148692308, -296.3048248823506583, -343.6773935663883321 ) ) ;
#84847 = CARTESIAN_POINT ( 'NONE',  ( -26.14669701250242895, -295.9859452670694964, -342.8103966413188459 ) ) ;
#84848 = DIRECTION ( 'NONE',  ( 1.000000000000000000, 0.000000000000000000, 0.000000000000000000 ) ) ;
#84849 = CARTESIAN_POINT ( 'NONE',  ( -34.86007271588531609, -296.6215858104486074, -346.5207000627032130 ) ) ;
#84850 = CARTESIAN_POINT ( 'NONE',  ( -69.91106507176493778, -295.6240379100742075, -202.6170045935101029 ) ) ;
#84851 = CARTESIAN_POINT ( 'NONE',  ( -57.69126134834083786, -292.4339055353319168, -200.0957162742227240 ) ) ;
#84852 = CARTESIAN_POINT ( 'NONE',  ( -83.49128943082487808, -274.2405127590476468, -208.8585822593338150 ) ) ;
#84853 = CARTESIAN_POINT ( 'NONE',  ( -108.2987918063060135, -288.8689973908423667, -290.0546149252017472 ) ) ;
#84854 = CARTESIAN_POINT ( 'NONE',  ( 72.69263585473569833, -301.4297953448794374, -195.3235991646452305 ) ) ;
#84855 = CARTESIAN_POINT ( 'NONE',  ( -99.52102728028046386, -273.6473780954311792, -224.9598749675746490 ) ) ;
#84856 = CARTESIAN_POINT ( 'NONE',  ( -65.58481138269844735, -298.0056301264149283, -203.0230592528929776 ) ) ;
#84857 = CARTESIAN_POINT ( 'NONE',  ( -1.931131629580074893, -282.4987032624279664, -203.8442145391391875 ) ) ;
#84858 = CARTESIAN_POINT ( 'NONE',  ( 12.68245189519852190, -279.4178322048057908, -212.4743104539741125 ) ) ;
#84859 = CARTESIAN_POINT ( 'NONE',  ( -107.4865335111504834, -277.4962938740018785, -302.0028618746571283 ) ) ;
#84860 = ADVANCED_FACE ( 'NONE', ( #73051 ), #91096, .T. ) ;
#84861 = CARTESIAN_POINT ( 'NONE',  ( -17.18380655957072278, -278.7080205149388235, -196.8757470545449451 ) ) ;
#84862 = CARTESIAN_POINT ( 'NONE',  ( 31.86769885117764289, -279.9358960448640801, -299.8211820090648985 ) ) ;
#84863 = CARTESIAN_POINT ( 'NONE',  ( -54.33008881778547305, -272.4043472460634234, -198.7596545537465715 ) ) ;
#84864 = CARTESIAN_POINT ( 'NONE',  ( -5.607782151842636509, -278.6350174575242704, -338.3305266278346153 ) ) ;
#84865 = DIRECTION ( 'NONE',  ( -0.4472135954999548191, 0.4472135954999599261, 0.7745966692414840704 ) ) ;
#84866 = CARTESIAN_POINT ( 'NONE',  ( 196.0143093133015384, 19.33012701892219098, 12.49999999999999467 ) ) ;
#84867 = CARTESIAN_POINT ( 'NONE',  ( -65.15000598038282931, -295.9337240579027366, -199.5894554512790364 ) ) ;
#84868 = AXIS2_PLACEMENT_3D ( 'NONE', #58926, #80688, #30984 ) ;
#84869 = CARTESIAN_POINT ( 'NONE',  ( -37.79503013874025896, -292.0466210835031120, -193.3624524622963747 ) ) ;
#84870 = CARTESIAN_POINT ( 'NONE',  ( 32.49071750981946849, -277.9153491248761156, -298.3127502029152538 ) ) ;
#84871 = CARTESIAN_POINT ( 'NONE',  ( -8.170028999098940758, -272.4338772151675698, -201.2114776745634117 ) ) ;
#84872 = DIRECTION ( 'NONE',  ( 1.000000000000000000, 0.000000000000000000, 0.000000000000000000 ) ) ;
#84873 = CARTESIAN_POINT ( 'NONE',  ( -49.83095356496649231, -285.1302866145171038, -344.9346702000764253 ) ) ;
#84874 = FILL_AREA_STYLE ('',( #20513 ) ) ;
#84875 = CARTESIAN_POINT ( 'NONE',  ( -1.551112478440801468, -284.5260410164028144, -204.3946948250082869 ) ) ;
#84876 = CYLINDRICAL_SURFACE ( 'NONE', #37627, 1.000000000000000888 ) ;
#84877 = CARTESIAN_POINT ( 'NONE',  ( 18.26326524469824619, -293.0258933389397953, -318.2887129829994137 ) ) ;
#84878 = CARTESIAN_POINT ( 'NONE',  ( 36.18046615318034753, -285.8260804812475158, -280.7177935575422225 ) ) ;
#84879 = DIRECTION ( 'NONE',  ( 0.000000000000000000, 1.000000000000000000, 0.000000000000000000 ) ) ;
#84880 = CARTESIAN_POINT ( 'NONE',  ( 11.57728245303386316, -292.3731666270389837, -327.2112172708158937 ) ) ;
#84881 = CARTESIAN_POINT ( 'NONE',  ( -23.88894097986979759, -284.7007541918591755, -195.1959296855863215 ) ) ;
#84882 = CARTESIAN_POINT ( 'NONE',  ( -111.1924062690921176, -280.1483698570180536, -270.6614252967327161 ) ) ;
#84883 = CARTESIAN_POINT ( 'NONE',  ( -4.955841750281797964, -287.6742364407118657, -200.9409127292508686 ) ) ;
#84884 = CARTESIAN_POINT ( 'NONE',  ( 29.83657330895386295, -279.3260770113772082, -234.7375636802884742 ) ) ;
#84885 = CARTESIAN_POINT ( 'NONE',  ( 35.27439374902280633, -287.4535204284661631, -262.8842931195853794 ) ) ;
#84886 = CARTESIAN_POINT ( 'NONE',  ( -27.49737763341369501, -281.6048002811040760, -197.3817137364107737 ) ) ;
#84887 = CARTESIAN_POINT ( 'NONE',  ( -51.86940424075815059, -280.6644473029521123, -198.6046865971727300 ) ) ;
#84888 = EDGE_CURVE ( 'NONE', #70448, #12291, #42261, .T. ) ;
#84889 = CARTESIAN_POINT ( 'NONE',  ( -29.65630261754789032, -288.1289141567871752, -195.3988510269741710 ) ) ;
#84890 = VERTEX_POINT ( 'NONE', #52643 ) ;
#84891 = CARTESIAN_POINT ( 'NONE',  ( -91.63402372937669327, -297.1375136660911380, -215.7594366671517037 ) ) ;
#84892 = CARTESIAN_POINT ( 'NONE',  ( -81.35751155469240814, -291.6334289761899754, -330.7118640853988154 ) ) ;
#84893 = LINE ( 'NONE', #48923, #38259 ) ;
#84894 = CARTESIAN_POINT ( 'NONE',  ( -54.49178911615187815, -276.3376638359844151, -195.3683826091709363 ) ) ;
#84895 = EDGE_LOOP ( 'NONE', ( #58941, #70976, #34962, #45795 ) ) ;
#84896 = CARTESIAN_POINT ( 'NONE',  ( -84.63452168851617330, -271.4021107462828581, -211.9366586157784695 ) ) ;
#84897 = EDGE_CURVE ( 'NONE', #22426, #77986, #15775, .T. ) ;
#84898 = DIRECTION ( 'NONE',  ( 0.000000000000000000, 1.000000000000000000, 0.000000000000000000 ) ) ;
#84899 = CARTESIAN_POINT ( 'NONE',  ( -41.91809878868544104, -293.5086537330012675, -346.4754211083483142 ) ) ;
#84900 = CARTESIAN_POINT ( 'NONE',  ( -39.16358283339859270, -297.5363618254613698, -197.3098788183234547 ) ) ;
#84901 = CARTESIAN_POINT ( 'NONE',  ( -23.63743177913956117, -290.3941044910961295, -342.8211883146426544 ) ) ;
#84902 = CARTESIAN_POINT ( 'NONE',  ( 29.88382654553237927, -282.8988336313091736, -239.2754536350166745 ) ) ;
#84903 = CARTESIAN_POINT ( 'NONE',  ( -36.07824168314350999, -290.4619016368691291, -346.7744547805619959 ) ) ;
#84904 = CARTESIAN_POINT ( 'NONE',  ( -57.14698346822036967, -290.6175147624210808, -344.3147773715898552 ) ) ;
#84905 = CARTESIAN_POINT ( 'NONE',  ( -70.89955365870332571, -287.6096530891726957, -203.2731652206429942 ) ) ;
#84906 = CARTESIAN_POINT ( 'NONE',  ( -67.36441661612408893, -279.8358102449926719, -199.4552895959129728 ) ) ;
#84907 = CARTESIAN_POINT ( 'NONE',  ( -58.47250858125631368, -293.4029460493510442, -342.9608360133648830 ) ) ;
#84908 = CARTESIAN_POINT ( 'NONE',  ( 35.60840098083281191, -281.6977358413952288, -295.1699114067511687 ) ) ;
#84909 = CARTESIAN_POINT ( 'NONE',  ( 36.83746114244013370, -277.4643956643378715, -274.3558725303914230 ) ) ;
#84910 = EDGE_CURVE ( 'NONE', #2619, #26019, #81523, .T. ) ;
#84911 = CARTESIAN_POINT ( 'NONE',  ( 17.40634833298267736, -278.6948066931273047, -313.9805196606274080 ) ) ;
#84912 = CARTESIAN_POINT ( 'NONE',  ( 31.64265073936129724, -273.3775357678563296, -238.3745803437362838 ) ) ;
#84913 = CARTESIAN_POINT ( 'NONE',  ( 19.39586235373092649, -281.7107656293368336, -316.4116675856188863 ) ) ;
#84914 = CARTESIAN_POINT ( 'NONE',  ( -75.12691378274729459, -278.7491654808909516, -336.9965916272910817 ) ) ;
#84915 = CARTESIAN_POINT ( 'NONE',  ( -104.8392231956981817, -274.2569284932557707, -241.1575596628881613 ) ) ;
#84916 = CARTESIAN_POINT ( 'NONE',  ( -112.7647670213274154, -283.7935797413243790, -255.7955779959871734 ) ) ;
#84917 = CARTESIAN_POINT ( 'NONE',  ( -109.0963412854132031, -292.5491035610610879, -252.1643872380254265 ) ) ;
#84918 = CARTESIAN_POINT ( 'NONE',  ( -68.53540802779889418, -275.2492049255736788, -200.8242624724241523 ) ) ;
#84919 = CARTESIAN_POINT ( 'NONE',  ( -105.1794743133070256, -274.3278742879541028, -234.8723594374499442 ) ) ;
#84920 = FACE_BOUND ( 'NONE', #72376, .T. ) ;
#84921 = CARTESIAN_POINT ( 'NONE',  ( -19.01899488175570951, -276.6429645257778134, -341.0242517719701141 ) ) ;
#84922 = CARTESIAN_POINT ( 'NONE',  ( -111.9241880270047602, -298.4657364798912909, -277.0891985200167937 ) ) ;
#84923 = CARTESIAN_POINT ( 'NONE',  ( -68.28304432140735969, -283.6446333453809530, -202.2240381397060673 ) ) ;
#84924 = CARTESIAN_POINT ( 'NONE',  ( -0.8101501031219983107, -292.1905315015141582, -202.6027963951183608 ) ) ;
#84925 = CARTESIAN_POINT ( 'NONE',  ( 25.18474047723890052, -273.0197794820817876, -229.5899145719604348 ) ) ;
#84926 = CARTESIAN_POINT ( 'NONE',  ( 38.80595800771392589, -289.2028216164353012, -274.3604172580151044 ) ) ;
#84927 = CARTESIAN_POINT ( 'NONE',  ( -103.1288549890172277, -289.0360352589741524, -302.7073129355213723 ) ) ;
#84928 = ORIENTED_EDGE ( 'NONE', *, *, #25761, .T. ) ;
#84929 = CARTESIAN_POINT ( 'NONE',  ( -73.14146154720549475, -290.1618383140167339, -202.8409016208236437 ) ) ;
#84930 = CARTESIAN_POINT ( 'NONE',  ( -96.77609858494014361, -290.8124272117787541, -227.8534361110645250 ) ) ;
#84931 = ORIENTED_EDGE ( 'NONE', *, *, #41482, .T. ) ;
#84932 = CARTESIAN_POINT ( 'NONE',  ( 38.24983755128842233, -288.4683809945918256, -257.3451653380889752 ) ) ;
#84933 = CARTESIAN_POINT ( 'NONE',  ( -110.4130751150576515, -278.8817264824106132, -270.6423695624922630 ) ) ;
#84934 = CARTESIAN_POINT ( 'NONE',  ( -19.37310057854351797, -293.7466992563412305, -344.9719473593676184 ) ) ;
#84935 = CARTESIAN_POINT ( 'NONE',  ( -37.98991983772272363, -286.6956400288447639, -193.4657826341520206 ) ) ;
#84936 = CARTESIAN_POINT ( 'NONE',  ( -87.73930435206074208, -285.7040590267891389, -212.1026971947967752 ) ) ;
#84937 = CARTESIAN_POINT ( 'NONE',  ( 32.25276550568090528, -282.1804106144927573, -292.6323394454112758 ) ) ;
#84938 = CARTESIAN_POINT ( 'NONE',  ( 153.9038455766559252, 207.1106375885822786, -217.3830698506460521 ) ) ;
#84939 = CIRCLE ( 'NONE', #39554, 0.5000000000000048850 ) ;
#84940 = CARTESIAN_POINT ( 'NONE',  ( 166.5459560125245275, 232.5563224728020373, -191.9177544221001028 ) ) ;
#84941 = CARTESIAN_POINT ( 'NONE',  ( 192.2295762369160457, 276.4233758247025889, -124.0683339759032435 ) ) ;
#84942 = AXIS2_PLACEMENT_3D ( 'NONE', #86274, #14349, #81956 ) ;
#84943 = CARTESIAN_POINT ( 'NONE',  ( 17.41319056084516959, -274.0568178855980932, -221.7628093281351482 ) ) ;
#84944 = CARTESIAN_POINT ( 'NONE',  ( 33.16109047770582663, -274.2058278414356209, -250.0902415138952506 ) ) ;
#84945 = CARTESIAN_POINT ( 'NONE',  ( -114.3048253765348647, -296.0335123176099614, -272.4618511282888562 ) ) ;
#84946 = CARTESIAN_POINT ( 'NONE',  ( 26.53395668783571182, -24.55290782687918139, -341.8058727006235813 ) ) ;
#84947 = CARTESIAN_POINT ( 'NONE',  ( 23.96239827260135868, -274.8498358534708927, -316.1334436095236811 ) ) ;
#84948 = CARTESIAN_POINT ( 'NONE',  ( -89.00205447178591101, -299.1775367070667926, -216.9782278248142404 ) ) ;
#84949 = CARTESIAN_POINT ( 'NONE',  ( -81.92789847499841471, -292.5081938149662051, -212.1049742978525785 ) ) ;
#84950 = VERTEX_POINT ( 'NONE', #24234 ) ;
#84951 = CARTESIAN_POINT ( 'NONE',  ( -110.9862564060357073, -297.2203015256591243, -292.0707797470780065 ) ) ;
#84952 = VECTOR ( 'NONE', #13184, 1000.000000000000000 ) ;
#84953 = CARTESIAN_POINT ( 'NONE',  ( 34.58337333767331501, -288.2136916304594365, -283.1974822935964653 ) ) ;
#84954 = CARTESIAN_POINT ( 'NONE',  ( -112.4451590605510063, -297.1514918223394943, -286.5977825920128907 ) ) ;
#84955 = CARTESIAN_POINT ( 'NONE',  ( -58.82811829318622188, -295.8150589477813810, -344.2939800234042877 ) ) ;
#84956 = CARTESIAN_POINT ( 'NONE',  ( 16.73675102980893570, -293.0155130479860190, -221.2510649776955063 ) ) ;
#84957 = ORIENTED_EDGE ( 'NONE', *, *, #4770, .T. ) ;
#84958 = CARTESIAN_POINT ( 'NONE',  ( 35.11960803832374012, -277.7466278287836303, -291.8234714321406500 ) ) ;
#84959 = VERTEX_POINT ( 'NONE', #67806 ) ;
#84960 = CARTESIAN_POINT ( 'NONE',  ( -8.878044875214289533, -279.9223401578673247, -198.8814199354349057 ) ) ;
#84961 = CARTESIAN_POINT ( 'NONE',  ( 13.90451201885680987, -277.2532243289963958, -322.7503405305836282 ) ) ;
#84962 = CARTESIAN_POINT ( 'NONE',  ( 36.94986507705546330, -277.1092387535302350, -254.3391954089093190 ) ) ;
#84963 = CARTESIAN_POINT ( 'NONE',  ( -111.1869626077413642, -276.3796360804223582, -285.4344538218659864 ) ) ;
#84964 = CARTESIAN_POINT ( 'NONE',  ( -103.8147315674224984, -297.6146669658842256, -239.8216752366159028 ) ) ;
#84965 = CARTESIAN_POINT ( 'NONE',  ( -67.55358021487614906, -294.0311696544250140, -337.4764806566925017 ) ) ;
#84966 = CARTESIAN_POINT ( 'NONE',  ( -107.5173985441935969, -278.6398702184750391, -302.0327398168233799 ) ) ;
#84967 = CARTESIAN_POINT ( 'NONE',  ( -68.03548982078876861, -277.6334048858773826, -336.6084767317124147 ) ) ;
#84968 = APPLICATION_CONTEXT ( 'automotive_design' ) ;
#84969 = EDGE_CURVE ( 'NONE', #75719, #10071, #84026, .T. ) ;
#84970 = CARTESIAN_POINT ( 'NONE',  ( 32.27032689822701172, -285.8271789734006916, -238.4929518292211412 ) ) ;
#84971 = CARTESIAN_POINT ( 'NONE',  ( -23.79882560928694701, -300.2214628073405720, -195.1898382442023774 ) ) ;
#84972 = CARTESIAN_POINT ( 'NONE',  ( 82.63422563859604963, -300.7068507995575715, -197.5857633699117741 ) ) ;
#84973 = CARTESIAN_POINT ( 'NONE',  ( 34.16633119161235044, -286.9536168546941894, -285.8860302165797407 ) ) ;
#84974 = CARTESIAN_POINT ( 'NONE',  ( -52.00651184383531955, -278.1018859024631524, -197.7627052112191564 ) ) ;
#84976 = CARTESIAN_POINT ( 'NONE',  ( -109.1567198465016730, -282.3775832054524813, -290.0031066220593630 ) ) ;
#84975 = CARTESIAN_POINT ( 'NONE',  ( -38.34378613340424380, -278.6140778668016651, -196.7662097404028998 ) ) ;
#84977 = CARTESIAN_POINT ( 'NONE',  ( -37.40560091916179886, -288.0514730517481894, -195.3485665393942554 ) ) ;
#84978 = CARTESIAN_POINT ( 'NONE',  ( 21.16266784627691067, -277.3766754572978925, -314.6823254777914372 ) ) ;
#84979 = CYLINDRICAL_SURFACE ( 'NONE', #68452, 4.999999999999990230 ) ;
#84980 = CARTESIAN_POINT ( 'NONE',  ( -91.38897937504209779, -293.2837682531524024, -218.2882407209644953 ) ) ;
#84981 = CARTESIAN_POINT ( 'NONE',  ( -110.4714660641430015, -276.5298901964705465, -291.0011603537972178 ) ) ;
#84982 = CARTESIAN_POINT ( 'NONE',  ( -9.942470107421407022, -277.3360991616660272, -338.1476689253897803 ) ) ;
#84983 = CARTESIAN_POINT ( 'NONE',  ( 21.11399038967085318, -284.2015567204788908, -317.6356483939983377 ) ) ;
#84984 = CARTESIAN_POINT ( 'NONE',  ( 216.5288609127277084, 293.9636489450776935, -40.00000000000000711 ) ) ;
#84985 = CARTESIAN_POINT ( 'NONE',  ( 35.97356913955299973, -289.2392332292763513, -252.0803769219947981 ) ) ;
#84986 = CARTESIAN_POINT ( 'NONE',  ( -100.8917166006252444, -295.0883993059197223, -230.4351542719718395 ) ) ;
#84987 = DIRECTION ( 'NONE',  ( -0.000000000000000000, -1.000000000000000000, -0.000000000000000000 ) ) ;
#84988 = CARTESIAN_POINT ( 'NONE',  ( -36.71515387767735916, -272.7450092991016959, -196.8581369266514685 ) ) ;
#84989 = CARTESIAN_POINT ( 'NONE',  ( 35.16122893312238062, -291.4841527466867888, -254.3588944933474636 ) ) ;
#84990 = CARTESIAN_POINT ( 'NONE',  ( 209.7513585654923816, 282.2246705312486483, 13.99999999999999112 ) ) ;
#84991 = CARTESIAN_POINT ( 'NONE',  ( 175.2296996224750103, 140.2072866198470251, 0.000000000000000000 ) ) ;
#84992 = CARTESIAN_POINT ( 'NONE',  ( -39.17545016596928065, -290.5094486551427053, -194.0635676381172914 ) ) ;
#84993 = CARTESIAN_POINT ( 'NONE',  ( -109.1996264325236581, -285.9321616995211457, -287.2352679458221587 ) ) ;
#84994 = CARTESIAN_POINT ( 'NONE',  ( 38.56668245091941571, -285.7354812931919241, -265.9005228054472241 ) ) ;
#84995 = CARTESIAN_POINT ( 'NONE',  ( -106.7232414177929058, -285.6518306470258040, -295.0398112443616583 ) ) ;
#84996 = CARTESIAN_POINT ( 'NONE',  ( -62.62825852687898021, -286.5174504684008525, -201.6543986694567536 ) ) ;
#84997 = ADVANCED_FACE ( 'NONE', ( #81072, #89085, #39351 ), #10954, .T. ) ;
#84998 = CARTESIAN_POINT ( 'NONE',  ( -33.64580452643579633, -294.0783471029640168, -195.0966033673003608 ) ) ;
#84999 = CARTESIAN_POINT ( 'NONE',  ( 27.84113642410498812, -274.1389517394873678, -308.5777637675636811 ) ) ;
#85000 = VECTOR ( 'NONE', #28635, 1000.000000000000000 ) ;
#85001 = CARTESIAN_POINT ( 'NONE',  ( 36.86637103746694777, -276.1424552926130218, -290.8774825076309298 ) ) ;
#85002 = VECTOR ( 'NONE', #16952, 1000.000000000000000 ) ;
#85003 = CARTESIAN_POINT ( 'NONE',  ( -103.3400973420037019, -289.1180632144612446, -233.5708235992334778 ) ) ;
#85004 = CARTESIAN_POINT ( 'NONE',  ( -97.92890798767126626, -277.9168926245682201, -317.8815372123905263 ) ) ;
#85005 = CARTESIAN_POINT ( 'NONE',  ( -108.4280933938048719, -298.2347514992417814, -293.3004310822690854 ) ) ;
#85006 = CARTESIAN_POINT ( 'NONE',  ( -48.18343439339133027, -248.3668650810686529, -472.6442049081570076 ) ) ;
#85007 = CARTESIAN_POINT ( 'NONE',  ( 208.2940771383659069, 37.39347744730360290, 12.94649967098113841 ) ) ;
#85008 = CARTESIAN_POINT ( 'NONE',  ( -107.8231473814541062, -283.5127527382658741, -249.3614744254330446 ) ) ;
#85009 = AXIS2_PLACEMENT_3D ( 'NONE', #92934, #7232, #28548 ) ;
#85010 = CARTESIAN_POINT ( 'NONE',  ( -47.81366247784037427, -277.9189514113317045, -196.0433481135916622 ) ) ;
#85011 = LINE ( 'NONE', #28217, #54328 ) ;
#85012 = CARTESIAN_POINT ( 'NONE',  ( 29.35105616525251548, -273.5458214539480082, -233.1743350792007732 ) ) ;
#85013 = CARTESIAN_POINT ( 'NONE',  ( -108.5874797671769869, -277.6843782749242564, -286.7852344899939112 ) ) ;
#85014 = VECTOR ( 'NONE', #3609, 1000.000000000000000 ) ;
#85015 = CARTESIAN_POINT ( 'NONE',  ( 17.61037683689601607, -295.7682070007553534, -319.4818498119317951 ) ) ;
#85016 = CARTESIAN_POINT ( 'NONE',  ( 34.04176770134874630, -280.1140271836077886, -242.1823243726990711 ) ) ;
#85017 = CARTESIAN_POINT ( 'NONE',  ( -78.07067670734340936, -296.5554807102024029, -331.2874521303659208 ) ) ;
#85018 = CARTESIAN_POINT ( 'NONE',  ( -3.432195700594277810, -295.9290958468386634, -338.9572874588480431 ) ) ;
#85019 = CARTESIAN_POINT ( 'NONE',  ( -94.44999314464222095, -297.0276148570155215, -224.8897767523308175 ) ) ;
#85020 = CARTESIAN_POINT ( 'NONE',  ( -14.25428822253264727, -294.3517285943561319, -199.0030626670235279 ) ) ;
#85021 = CARTESIAN_POINT ( 'NONE',  ( -32.30853939835375144, -286.2806215865667809, -193.5126258549709632 ) ) ;
#85022 = CARTESIAN_POINT ( 'NONE',  ( 23.50230962071297469, -273.0816993731379512, -225.2134495984524278 ) ) ;
#85023 = CARTESIAN_POINT ( 'NONE',  ( 3.178330159813210987, -288.3574600643131589, -335.8998220271025730 ) ) ;
#85024 = CARTESIAN_POINT ( 'NONE',  ( -34.27033393422726704, -282.0708196800877090, -195.7667020218742664 ) ) ;
#85025 = EDGE_CURVE ( 'NONE', #69004, #85642, #2930, .T. ) ;
#85026 = CARTESIAN_POINT ( 'NONE',  ( -14.48121458390158089, -285.4145089231023462, -200.7320195045245441 ) ) ;
#85027 = CARTESIAN_POINT ( 'NONE',  ( -88.15564890472626303, -287.7633390326610083, -325.5239973142273584 ) ) ;
#85028 = CARTESIAN_POINT ( 'NONE',  ( -98.31850732666445936, -258.1384851437703674, -325.6453615436536211 ) ) ;
#85029 = CARTESIAN_POINT ( 'NONE',  ( 26.42414952981355469, -286.5711500632839943, -234.5938157740320378 ) ) ;
#85030 = CARTESIAN_POINT ( 'NONE',  ( 190.2832783574276903, 8.542400036368780647, 25.74970488511327815 ) ) ;
#85031 = CARTESIAN_POINT ( 'NONE',  ( 24.92348424847820354, -283.0907775280153942, -315.2818436728126130 ) ) ;
#85032 = EDGE_CURVE ( 'NONE', #13010, #17769, #58101, .T. ) ;
#85033 = CARTESIAN_POINT ( 'NONE',  ( -103.0083337835546047, -290.1325745038440687, -230.5004701966750531 ) ) ;
#85034 = CARTESIAN_POINT ( 'NONE',  ( -95.31061226682197685, -280.8265108970002757, -220.8835565826972527 ) ) ;
#85035 = CARTESIAN_POINT ( 'NONE',  ( -92.72838467810875329, -280.5942064235289308, -217.5064947537138949 ) ) ;
#85036 = CARTESIAN_POINT ( 'NONE',  ( 32.23067187854067583, -281.6805300397424503, -292.6319561521697210 ) ) ;
#85037 = CARTESIAN_POINT ( 'NONE',  ( 34.43772122113939105, -277.8330348420646487, -292.1477060132437487 ) ) ;
#85038 = CARTESIAN_POINT ( 'NONE',  ( 24.88627965927573626, -294.1543096074584014, -315.7339456628644712 ) ) ;
#85039 = CARTESIAN_POINT ( 'NONE',  ( -110.0233630504302909, -288.7923819366740190, -253.2989071530174954 ) ) ;
#85040 =( BOUNDED_CURVE ( )  B_SPLINE_CURVE ( 3, ( #34562, #68680, #40226, #70564 ),
 .UNSPECIFIED., .F., .F. ) 
 B_SPLINE_CURVE_WITH_KNOTS ( ( 4, 4 ),
 ( 0.000000000000000000, 0.2609887789853130857 ),
 .UNSPECIFIED. ) 
 CURVE ( )  GEOMETRIC_REPRESENTATION_ITEM ( )  RATIONAL_B_SPLINE_CURVE ( ( 1.000000000000000000, 0.9943317885200935180, 0.9943317885200935180, 1.000000000000000000 ) ) 
 REPRESENTATION_ITEM ( '' )  );
#85041 = CARTESIAN_POINT ( 'NONE',  ( -110.5510762278442201, -295.4222589701827246, -274.1838557289810296 ) ) ;
#85042 = ORIENTED_EDGE ( 'NONE', *, *, #46621, .F. ) ;
#85043 = ORIENTED_EDGE ( 'NONE', *, *, #33978, .F. ) ;
#85044 = CARTESIAN_POINT ( 'NONE',  ( 35.35181989373702294, -283.6796792428266372, -286.3912879321316041 ) ) ;
#85045 = CARTESIAN_POINT ( 'NONE',  ( -84.49499115023635909, -295.3889148290286357, -326.1828206211164343 ) ) ;
#85046 =( BOUNDED_SURFACE ( )  B_SPLINE_SURFACE ( 3, 3, ( 
 ( #41429, #18748, #70816, #57545, #79773, #71765, #51340, #13066, #13988, #71284, #27729, #41902, #64214, #42849, #78842, #79329, #93043, #6888, #22022, #86390, #50424, #63733, #236, #43771 ),
 ( #5948, #34820, #21541, #14916, #35762, #92558, #56626, #64675, #6411, #85476, #20623, #28200, #93502, #28657, #14466, #57088, #43323, #50892, #72219, #7335, #49494, #29116, #72672, #78383 ),
 ( #13524, #7792, #58012, #712, #35286, #42372, #85928, #29597, #36215, #21078, #36677, #65599, #49949, #65135, #86868, #87320, #58476, #22468, #73605, #81158, #73141, #24805, #67441, #2099 ),
 ( #1623, #16763, #52731, #74054, #1167, #59401, #81614, #15370, #60336, #23865, #9173, #51801, #8267, #87781, #16302, #30506, #30990, #58931, #88255, #44704, #45617, #2568, #89635, #75005 ),
 ( #45155, #15847, #74518, #88717, #37147, #52279, #89173, #9653, #80693, #38538, #22931, #3019, #23413, #31447, #66960, #53202, #66504, #30050, #38983, #24325, #44232, #80234, #59877, #8716 ),
 ( #37593, #38051, #82080, #66054, #17238, #46100, #10117, #67896, #60797, #31905, #83473, #26675, #69758, #68358, #11526, #19561, #11990, #39442, #46559, #32838, #84413, #4419, #10579, #17706 ),
 ( #19106, #48427, #47961, #47495, #70249, #54143, #83012, #62195, #3486, #54602, #18164, #76865, #91025, #75458, #25718, #33773, #26194, #47017, #55088, #90114, #5384, #61728, #40839, #40373 ) ),
 .UNSPECIFIED., .T., .F., .F. ) 
 B_SPLINE_SURFACE_WITH_KNOTS ( ( 4, 3, 4 ),
 ( 4, 2, 2, 2, 2, 2, 2, 2, 2, 2, 2, 4 ),
 ( 0.000000000000000000, 0.5000000000000000000, 1.000000000000000000 ),
 ( 0.000000000000000000, 0.06250000000000000000, 0.1250000000000000000, 0.2500000000000000000, 0.3750000000000000000, 0.5000000000000000000, 0.6250000000000000000, 0.7500000000000000000, 0.8125000000000000000, 0.8750000000000000000, 0.9375000000000000000, 1.000000000000000000 ),
 .UNSPECIFIED. ) 
 GEOMETRIC_REPRESENTATION_ITEM ( )  RATIONAL_B_SPLINE_SURFACE ( (
 ( 1.000000000000000000, 1.000000000000000000, 1.000000000000000000, 1.000000000000000000, 1.000000000000000000, 1.000000000000000000, 1.000000000000000000, 1.000000000000000000, 1.000000000000000000, 1.000000000000000000, 1.000000000000000000, 1.000000000000000000, 1.000000000000000000, 1.000000000000000000, 1.000000000000000000, 1.000000000000000000, 1.000000000000000000, 1.000000000000000000, 1.000000000000000000, 1.000000000000000000, 1.000000000000000000, 1.000000000000000000, 1.000000000000000000, 1.000000000000000000),
 ( 0.3333333333333333703, 0.3333333333333333703, 0.3333333333333333703, 0.3333333333333333703, 0.3333333333333333703, 0.3333333333333333703, 0.3333333333333333703, 0.3333333333333333703, 0.3333333333333333703, 0.3333333333333333703, 0.3333333333333333703, 0.3333333333333333703, 0.3333333333333333703, 0.3333333333333333703, 0.3333333333333333703, 0.3333333333333333703, 0.3333333333333333703, 0.3333333333333333703, 0.3333333333333333703, 0.3333333333333333703, 0.3333333333333333703, 0.3333333333333333703, 0.3333333333333333703, 0.3333333333333333703),
 ( 0.3333333333333333703, 0.3333333333333333703, 0.3333333333333333703, 0.3333333333333333703, 0.3333333333333333703, 0.3333333333333333703, 0.3333333333333333703, 0.3333333333333333703, 0.3333333333333333703, 0.3333333333333333703, 0.3333333333333333703, 0.3333333333333333703, 0.3333333333333333703, 0.3333333333333333703, 0.3333333333333333703, 0.3333333333333333703, 0.3333333333333333703, 0.3333333333333333703, 0.3333333333333333703, 0.3333333333333333703, 0.3333333333333333703, 0.3333333333333333703, 0.3333333333333333703, 0.3333333333333333703),
 ( 1.000000000000000000, 1.000000000000000000, 1.000000000000000000, 1.000000000000000000, 1.000000000000000000, 1.000000000000000000, 1.000000000000000000, 1.000000000000000000, 1.000000000000000000, 1.000000000000000000, 1.000000000000000000, 1.000000000000000000, 1.000000000000000000, 1.000000000000000000, 1.000000000000000000, 1.000000000000000000, 1.000000000000000000, 1.000000000000000000, 1.000000000000000000, 1.000000000000000000, 1.000000000000000000, 1.000000000000000000, 1.000000000000000000, 1.000000000000000000),
 ( 0.3333333333333333703, 0.3333333333333333703, 0.3333333333333333703, 0.3333333333333333703, 0.3333333333333333703, 0.3333333333333333703, 0.3333333333333333703, 0.3333333333333333703, 0.3333333333333333703, 0.3333333333333333703, 0.3333333333333333703, 0.3333333333333333703, 0.3333333333333333703, 0.3333333333333333703, 0.3333333333333333703, 0.3333333333333333703, 0.3333333333333333703, 0.3333333333333333703, 0.3333333333333333703, 0.3333333333333333703, 0.3333333333333333703, 0.3333333333333333703, 0.3333333333333333703, 0.3333333333333333703),
 ( 0.3333333333333333703, 0.3333333333333333703, 0.3333333333333333703, 0.3333333333333333703, 0.3333333333333333703, 0.3333333333333333703, 0.3333333333333333703, 0.3333333333333333703, 0.3333333333333333703, 0.3333333333333333703, 0.3333333333333333703, 0.3333333333333333703, 0.3333333333333333703, 0.3333333333333333703, 0.3333333333333333703, 0.3333333333333333703, 0.3333333333333333703, 0.3333333333333333703, 0.3333333333333333703, 0.3333333333333333703, 0.3333333333333333703, 0.3333333333333333703, 0.3333333333333333703, 0.3333333333333333703),
 ( 1.000000000000000000, 1.000000000000000000, 1.000000000000000000, 1.000000000000000000, 1.000000000000000000, 1.000000000000000000, 1.000000000000000000, 1.000000000000000000, 1.000000000000000000, 1.000000000000000000, 1.000000000000000000, 1.000000000000000000, 1.000000000000000000, 1.000000000000000000, 1.000000000000000000, 1.000000000000000000, 1.000000000000000000, 1.000000000000000000, 1.000000000000000000, 1.000000000000000000, 1.000000000000000000, 1.000000000000000000, 1.000000000000000000, 1.000000000000000000) ) ) 
 REPRESENTATION_ITEM ( '' )  SURFACE ( )  );
#85047 = CARTESIAN_POINT ( 'NONE',  ( 37.11851156330262569, -294.4011836843862966, -251.9989452932912570 ) ) ;
#85048 = CARTESIAN_POINT ( 'NONE',  ( -61.56067988772937127, -284.0265586835061526, -339.3878532841630999 ) ) ;
#85049 = CARTESIAN_POINT ( 'NONE',  ( -34.10109514277978349, -273.1507284015519872, -193.6648423704500033 ) ) ;
#85050 = CARTESIAN_POINT ( 'NONE',  ( -113.2580984399872790, -291.0501817850090447, -282.6091077774356108 ) ) ;
#85051 = CARTESIAN_POINT ( 'NONE',  ( -26.76964319381484358, -284.3246883260927689, -195.2848990172662695 ) ) ;
#85052 = CARTESIAN_POINT ( 'NONE',  ( -113.9862107040246570, -290.9819809125345955, -262.6433005713994930 ) ) ;
#85053 = CARTESIAN_POINT ( 'NONE',  ( -21.12051624089891888, -289.1715224738794632, -341.5577518915829955 ) ) ;
#85054 = CYLINDRICAL_SURFACE ( 'NONE', #27811, 28.04691768583012035 ) ;
#85055 = DIRECTION ( 'NONE',  ( 1.000000000000000000, 0.000000000000000000, 0.000000000000000000 ) ) ;
#85056 = CARTESIAN_POINT ( 'NONE',  ( 188.8180124195482108, 268.1546957682879224, -137.4927483566484341 ) ) ;
#85057 = CARTESIAN_POINT ( 'NONE',  ( -0.6912889005501295925, -284.0945348494694258, -337.3046558309981151 ) ) ;
#85058 = CARTESIAN_POINT ( 'NONE',  ( 10.59707575819633618, -279.9094976428775681, -330.5268031993606428 ) ) ;
#85059 = ORIENTED_EDGE ( 'NONE', *, *, #13462, .T. ) ;
#85060 = CARTESIAN_POINT ( 'NONE',  ( 7.974294312517242744, -281.3367078454543844, -328.0513402115038275 ) ) ;
#85061 = CARTESIAN_POINT ( 'NONE',  ( 1.032808759574668445, -276.2216535144020781, -337.1534396982845010 ) ) ;
#85062 = CARTESIAN_POINT ( 'NONE',  ( -77.31410124693465491, -279.5892618874532900, -333.6852744555749837 ) ) ;
#85063 = CARTESIAN_POINT ( 'NONE',  ( 175.1846718914974588, 240.5146751456763923, -177.8570858195099333 ) ) ;
#85064 = CARTESIAN_POINT ( 'NONE',  ( 30.20946171836731153, -279.6608920481897371, -234.5348671969436793 ) ) ;
#85065 = CARTESIAN_POINT ( 'NONE',  ( -49.66887700636713276, -283.9144179399754080, -196.6885766365219297 ) ) ;
#85066 = CARTESIAN_POINT ( 'NONE',  ( -97.44640746834767242, -298.9414116627343105, -223.8492702237638241 ) ) ;
#85067 = CARTESIAN_POINT ( 'NONE',  ( 35.35589676719921215, -293.9420632498192276, -262.5891425576214715 ) ) ;
#85068 = ORIENTED_EDGE ( 'NONE', *, *, #17385, .F. ) ;
#85069 = CARTESIAN_POINT ( 'NONE',  ( -98.70210651318809880, -289.7953113110343111, -229.8194318841307791 ) ) ;
#85070 = CARTESIAN_POINT ( 'NONE',  ( 37.18438702983876709, -275.9660981556214665, -251.4092019869858063 ) ) ;
#85071 = CARTESIAN_POINT ( 'NONE',  ( -103.2050763408169303, -272.9778981233729951, -238.8807165578695049 ) ) ;
#85072 = VERTEX_POINT ( 'NONE', #3392 ) ;
#85073 = CARTESIAN_POINT ( 'NONE',  ( -55.24805428201199220, -272.7473504839670113, -195.7899775206671791 ) ) ;
#85074 =( NAMED_UNIT ( * ) SI_UNIT ( $, .STERADIAN. ) SOLID_ANGLE_UNIT ( ) );
#85075 = CARTESIAN_POINT ( 'NONE',  ( 184.7149167944524493, -12.49482340714361506, 10.00000000000000000 ) ) ;
#85076 = CIRCLE ( 'NONE', #3422, 6.286090667950827715 ) ;
#85077 = CARTESIAN_POINT ( 'NONE',  ( 197.1123855246549113, 19.09807621135331601, 10.09807621135331246 ) ) ;
#85078 = CIRCLE ( 'NONE', #50341, 4.103083949679980691 ) ;
#85079 = CARTESIAN_POINT ( 'NONE',  ( 7.995872605634569474, -283.4957032231836820, -328.0343832530571717 ) ) ;
#85080 = CARTESIAN_POINT ( 'NONE',  ( -39.58016678030841717, -281.7845742691787336, -194.3945476324544757 ) ) ;
#85081 = CARTESIAN_POINT ( 'NONE',  ( -59.02920927561647346, -282.3983754484648898, -340.3648477261895664 ) ) ;
#85082 = CARTESIAN_POINT ( 'NONE',  ( 36.80074759569227894, -283.4606995728644847, -274.0709594013600281 ) ) ;
#85083 = CARTESIAN_POINT ( 'NONE',  ( 36.39223134863493669, -274.0484193847123038, -271.6159080386087794 ) ) ;
#85085 = FACE_OUTER_BOUND ( 'NONE', #56227, .T. ) ;
#85084 = VECTOR ( 'NONE', #61923, 1000.000000000000000 ) ;
#85086 = DIRECTION ( 'NONE',  ( 1.000000000000000000, 0.000000000000000000, 0.000000000000000000 ) ) ;
#85087 = AXIS2_PLACEMENT_3D ( 'NONE', #25915, #54798, #47695 ) ;
#85088 = CARTESIAN_POINT ( 'NONE',  ( -65.02732640655588625, -278.2074936529761544, -342.0947888608088192 ) ) ;
#85089 = EDGE_LOOP ( 'NONE', ( #70563, #66472 ) ) ;
#85090 = ORIENTED_EDGE ( 'NONE', *, *, #42395, .T. ) ;
#85091 = DIRECTION ( 'NONE',  ( 0.000000000000000000, 1.000000000000000000, 0.000000000000000000 ) ) ;
#85092 = CARTESIAN_POINT ( 'NONE',  ( -96.73218599766430259, -285.8987548337361204, -316.7419005904325218 ) ) ;
#85093 = EDGE_CURVE ( 'NONE', #56465, #41591, #33679, .T. ) ;
#85094 = CARTESIAN_POINT ( 'NONE',  ( -5.963122567394080420, -291.6726536459932504, -204.2565593400196349 ) ) ;
#85095 = CARTESIAN_POINT ( 'NONE',  ( -38.92640092054078593, -288.4201354131334369, -347.2428551534226813 ) ) ;
#85096 = CARTESIAN_POINT ( 'NONE',  ( -49.56713993043211985, -284.1341335259228913, -197.3122452978345507 ) ) ;
#85098 = CARTESIAN_POINT ( 'NONE',  ( 12.82642582302400491, -286.5808177466368534, -324.8470345085156055 ) ) ;
#85097 = CARTESIAN_POINT ( 'NONE',  ( -73.83216537073211327, -284.1322001869087899, -206.4417270484278504 ) ) ;
#85099 = CARTESIAN_POINT ( 'NONE',  ( 33.34597996191038760, -283.0169606376890670, -290.1192147791099956 ) ) ;
#85100 = CARTESIAN_POINT ( 'NONE',  ( -20.59804235624495306, -274.8371346787785114, -343.5215281646900962 ) ) ;
#85101 = CARTESIAN_POINT ( 'NONE',  ( 28.02290218778222552, -285.4347668228930388, -231.0941579304074480 ) ) ;
#85102 = CARTESIAN_POINT ( 'NONE',  ( -107.0396811834525721, -298.9146376407643970, -242.5232011649561343 ) ) ;
#85103 = CARTESIAN_POINT ( 'NONE',  ( -72.72688878428748183, -283.5848898605697173, -203.9866864869890151 ) ) ;
#85104 = CARTESIAN_POINT ( 'NONE',  ( -54.55969900859885513, -280.7668289612183230, -199.1262457046966290 ) ) ;
#85105 = CARTESIAN_POINT ( 'NONE',  ( 24.82639920173008363, -288.9813564662231329, -228.0870313837762353 ) ) ;
#85106 = CARTESIAN_POINT ( 'NONE',  ( 61.37083282337847123, -250.8548725835408391, 22.50000000000000000 ) ) ;
#85107 = FACE_OUTER_BOUND ( 'NONE', #41754, .T. ) ;
#85108 = CARTESIAN_POINT ( 'NONE',  ( 1.059069738076139355, -296.4639095254632934, -335.4356527227207039 ) ) ;
#85109 = CARTESIAN_POINT ( 'NONE',  ( -90.88400694663341994, -277.2926712029276928, -217.7687666443969761 ) ) ;
#85110 = CARTESIAN_POINT ( 'NONE',  ( -114.0260403342920767, -289.8102959298465748, -265.4958546589053867 ) ) ;
#85111 = CARTESIAN_POINT ( 'NONE',  ( -63.87544708689493689, -293.8037395226788249, -339.2803606632087394 ) ) ;
#85112 = CARTESIAN_POINT ( 'NONE',  ( -72.34997182512830705, -278.2633960628332375, -205.7417370536588521 ) ) ;
#85113 = CARTESIAN_POINT ( 'NONE',  ( -79.65387282725808404, -271.5556788880574004, -209.0531563296729303 ) ) ;
#85114 = CARTESIAN_POINT ( 'NONE',  ( 14.67709267725359723, -295.6162941855350823, -322.3488598585770433 ) ) ;
#85115 = CARTESIAN_POINT ( 'NONE',  ( -69.91165696735023971, -288.1233781216987495, -202.8022627189028810 ) ) ;
#85116 = CARTESIAN_POINT ( 'NONE',  ( -111.6352531339310730, -294.8115846643840428, -287.8296368892456485 ) ) ;
#85117 = CARTESIAN_POINT ( 'NONE',  ( -15.59669151028512601, -290.3663005782199775, -340.9382469843984609 ) ) ;
#85118 = CARTESIAN_POINT ( 'NONE',  ( -14.15406459776590964, -290.5885695910864115, -197.9435387665427584 ) ) ;
#85119 = CARTESIAN_POINT ( 'NONE',  ( -108.9193483062363015, -291.7537852849898741, -287.4495702318347412 ) ) ;
#85120 = DIRECTION ( 'NONE',  ( 0.000000000000000000, -1.000000000000000000, 0.000000000000000000 ) ) ;
#85121 = CARTESIAN_POINT ( 'NONE',  ( -52.41299710682623214, -292.6571432814385503, -198.7167985291134471 ) ) ;
#85122 = EDGE_CURVE ( 'NONE', #13924, #77289, #76262, .T. ) ;
#85123 = DIRECTION ( 'NONE',  ( -0.000000000000000000, 1.000000000000000000, -0.000000000000000000 ) ) ;
#85124 = CARTESIAN_POINT ( 'NONE',  ( -109.1072627452599590, -292.0995016353652431, -243.4197103671865250 ) ) ;
#85126 = CARTESIAN_POINT ( 'NONE',  ( 19.34579087098954631, -292.9012003052814634, -224.3464744986668506 ) ) ;
#85125 = CARTESIAN_POINT ( 'NONE',  ( 26.88952970955130795, -280.0995232924028073, -309.8649764031260929 ) ) ;
#85127 = CARTESIAN_POINT ( 'NONE',  ( 26.28061663383780555, -280.9790484413255172, -226.8952720309916913 ) ) ;
#85128 = CARTESIAN_POINT ( 'NONE',  ( -102.9022936410183036, -283.6914472266286111, -310.7040587492527948 ) ) ;
#85129 = CARTESIAN_POINT ( 'NONE',  ( -89.96800694927424047, -287.7974552624789908, -323.5635639376462791 ) ) ;
#85130 = CARTESIAN_POINT ( 'NONE',  ( 26.20571468236173729, -279.1711639553267901, -231.8870890982719857 ) ) ;
#85131 = CARTESIAN_POINT ( 'NONE',  ( -86.42140543987619594, -283.3709929050452843, -213.5809814034779777 ) ) ;
#85132 = CARTESIAN_POINT ( 'NONE',  ( 1.042114091244876084, -279.0342162657594827, -204.3510423811589760 ) ) ;
#85133 = CARTESIAN_POINT ( 'NONE',  ( 31.15191992416325917, -286.0267907822830011, -235.8630525147888477 ) ) ;
#85134 = DIRECTION ( 'NONE',  ( 1.000000000000000000, 0.000000000000000000, 0.000000000000000000 ) ) ;
#85135 = CARTESIAN_POINT ( 'NONE',  ( 34.22681023159566394, -295.3874046876959483, -288.3719131358678283 ) ) ;
#85136 = CARTESIAN_POINT ( 'NONE',  ( 33.16280089125246633, -276.5983525594442085, -240.7674246092316821 ) ) ;
#85137 = CARTESIAN_POINT ( 'NONE',  ( -104.2924725162575186, -277.8255362276186133, -299.6371340139624522 ) ) ;
#85138 = CARTESIAN_POINT ( 'NONE',  ( -72.17416494254028692, -291.7709689234059169, -201.6755684035830143 ) ) ;
#85139 = CIRCLE ( 'NONE', #82086, 4.999999999999985789 ) ;
#85140 = CARTESIAN_POINT ( 'NONE',  ( -67.33270816540002102, -281.5222478761535854, -339.7142263270876583 ) ) ;
#85141 = EDGE_CURVE ( 'NONE', #41846, #16234, #77763, .T. ) ;
#85142 = CARTESIAN_POINT ( 'NONE',  ( -110.2057910997127692, -289.7077302493710249, -262.9968329055291179 ) ) ;
#85143 = CIRCLE ( 'NONE', #74603, 4.999999999999986677 ) ;
#85144 = CARTESIAN_POINT ( 'NONE',  ( -79.47973234395216480, -295.4833137047606328, -208.2552614602541610 ) ) ;
#85145 = ORIENTED_EDGE ( 'NONE', *, *, #31275, .F. ) ;
#85146 = CARTESIAN_POINT ( 'NONE',  ( 151.4851178187871312, 20.00000000000000000, 3.492110388858642889 ) ) ;
#85147 = AXIS2_PLACEMENT_3D ( 'NONE', #82296, #1363, #89374 ) ;
#85148 = CARTESIAN_POINT ( 'NONE',  ( -37.54383090720561000, -291.5572420757261511, -197.2874045456559600 ) ) ;
#85149 = CYLINDRICAL_SURFACE ( 'NONE', #33825, 25.00000000000001066 ) ;
#85150 = CARTESIAN_POINT ( 'NONE',  ( -21.33282851196157992, -277.7666405000204577, -200.3683826091710216 ) ) ;
#85151 = CARTESIAN_POINT ( 'NONE',  ( -79.35822855277511678, -294.6633583261095168, -334.6062076911250074 ) ) ;
#85152 = CARTESIAN_POINT ( 'NONE',  ( 33.42520733454561110, -280.0399455443528041, -297.4230892120960448 ) ) ;
#85153 = CARTESIAN_POINT ( 'NONE',  ( -108.8360934830187432, -285.5186513751361304, -297.7455786420215418 ) ) ;
#85154 = CARTESIAN_POINT ( 'NONE',  ( 33.71080274108204833, -287.1638068335643084, -253.5577049223417418 ) ) ;
#85155 = CIRCLE ( 'NONE', #20140, 0.4999999999999998335 ) ;
#85156 = CARTESIAN_POINT ( 'NONE',  ( 28.66001379598199605, -277.5139176392491436, -303.2555014726411287 ) ) ;
#85157 = CARTESIAN_POINT ( 'NONE',  ( -110.7644855535513244, -294.3978074591867085, -283.8834992514319424 ) ) ;
#85158 = CARTESIAN_POINT ( 'NONE',  ( -110.0452475343240337, -298.4935408777866428, -256.4310379988921795 ) ) ;
#85159 = CARTESIAN_POINT ( 'NONE',  ( -105.8795943025450441, -277.6976001720707359, -243.9569400051724983 ) ) ;
#85160 = ORIENTED_EDGE ( 'NONE', *, *, #42029, .F. ) ;
#85161 = FACE_OUTER_BOUND ( 'NONE', #31848, .T. ) ;
#85162 = CARTESIAN_POINT ( 'NONE',  ( -113.1837907185554002, -296.0502194031610657, -283.8427757149162289 ) ) ;
#85163 = CARTESIAN_POINT ( 'NONE',  ( 35.70180492342255718, -289.6588162466495646, -284.7784461973581642 ) ) ;
#85164 = DIRECTION ( 'NONE',  ( -0.000000000000000000, -0.000000000000000000, -1.000000000000000000 ) ) ;
#85165 = AXIS2_PLACEMENT_3D ( 'NONE', #12452, #4877, #69279 ) ;
#85166 = ADVANCED_FACE ( 'NONE', ( #61641 ), #41219, .T. ) ;
#85167 = CARTESIAN_POINT ( 'NONE',  ( 34.86120687879893865, -288.3551833419904256, -281.8704210473467811 ) ) ;
#85168 = ORIENTED_EDGE ( 'NONE', *, *, #53277, .T. ) ;
#85169 = CARTESIAN_POINT ( 'NONE',  ( -73.64376054616512590, -278.6411536812860845, -202.7076109665544834 ) ) ;
#85170 = CARTESIAN_POINT ( 'NONE',  ( -113.0402375488554725, -297.3729904463028220, -256.8317344364228916 ) ) ;
#85171 = CARTESIAN_POINT ( 'NONE',  ( -111.9216962285983499, -288.5211690208938649, -283.7810469209765643 ) ) ;
#85172 = CARTESIAN_POINT ( 'NONE',  ( -99.98882173819012564, -296.2916962489630919, -315.1843537141244838 ) ) ;
#85173 = CARTESIAN_POINT ( 'NONE',  ( 20.19693193804779341, -293.2516516346162234, -225.3809688278342662 ) ) ;
#85174 = CARTESIAN_POINT ( 'NONE',  ( 198.6801208295229344, 66.92094681839049031, -8.363400713796702135 ) ) ;
#85175 = AXIS2_PLACEMENT_3D ( 'NONE', #80344, #67088, #59046 ) ;
#85176 = DIRECTION ( 'NONE',  ( 0.000000000000000000, -1.000000000000000000, 0.000000000000000000 ) ) ;
#85177 = DIRECTION ( 'NONE',  ( 1.000000000000000000, 0.000000000000000000, 0.000000000000000000 ) ) ;
#85178 = CARTESIAN_POINT ( 'NONE',  ( -74.07639917867282975, -291.0511989299233733, -337.2585403909363322 ) ) ;
#85179 = CARTESIAN_POINT ( 'NONE',  ( 36.57525178469696669, -283.6233781216987495, -234.7283546768995564 ) ) ;
#85180 = ORIENTED_EDGE ( 'NONE', *, *, #23115, .F. ) ;
#85181 = CARTESIAN_POINT ( 'NONE',  ( 33.46881879726637266, -281.2844262409695375, -300.4834513702567733 ) ) ;
#85182 = CARTESIAN_POINT ( 'NONE',  ( -72.24187692466479405, -285.5151786685437401, -336.5578406255497725 ) ) ;
#85183 = CARTESIAN_POINT ( 'NONE',  ( 36.12973860835963080, -285.8596019781211339, -249.1837030589231006 ) ) ;
#85184 = CARTESIAN_POINT ( 'NONE',  ( -94.53073418536543215, -289.2952341018810216, -222.6890646630564561 ) ) ;
#85185 = CARTESIAN_POINT ( 'NONE',  ( 36.42673736179660438, -277.1923038942890685, -253.0269380266633164 ) ) ;
#85186 = VECTOR ( 'NONE', #47271, 1000.000000000000114 ) ;
#85187 = ORIENTED_EDGE ( 'NONE', *, *, #63994, .T. ) ;
#85189 = CARTESIAN_POINT ( 'NONE',  ( -5.506616776514092315, -279.8309826340072846, -204.5551901600002225 ) ) ;
#85188 = CARTESIAN_POINT ( 'NONE',  ( -69.25141642484055637, -277.4839857884362573, -336.0314094350834466 ) ) ;
#85190 = CARTESIAN_POINT ( 'NONE',  ( -51.24304084389724778, -278.3055513681374009, -345.7815743271923452 ) ) ;
#85191 = CARTESIAN_POINT ( 'NONE',  ( -111.4472420527611121, -277.1023955594365589, -289.8131474838088479 ) ) ;
#85192 = CARTESIAN_POINT ( 'NONE',  ( 187.4789372167241766, 270.1634884999963901, -138.2063514411550500 ) ) ;
#85193 = CARTESIAN_POINT ( 'NONE',  ( -107.8660944823039074, -273.8822899904735664, -239.9094819157917300 ) ) ;
#85194 = CARTESIAN_POINT ( 'NONE',  ( -70.48996840331989233, -299.0489159655415961, -201.5149226909154550 ) ) ;
#85195 = CARTESIAN_POINT ( 'NONE',  ( -95.99890600148557951, -293.6948066931273615, -223.6242672951989618 ) ) ;
#85196 = CARTESIAN_POINT ( 'NONE',  ( 35.76128761417646729, -288.7123855299365687, -276.4935646971462688 ) ) ;
#85197 = CARTESIAN_POINT ( 'NONE',  ( -95.06171104682378825, -286.9886611357956099, -220.8617912217218588 ) ) ;
#85198 = CARTESIAN_POINT ( 'NONE',  ( 33.81144287587709840, -286.6791522105248760, -253.5402735174342581 ) ) ;
#85199 = CARTESIAN_POINT ( 'NONE',  ( -67.86271102804410305, -282.9498239865104097, -340.9868554797391198 ) ) ;
#85200 = CARTESIAN_POINT ( 'NONE',  ( 33.50826380960220519, -279.6817165435378456, -249.7038426051238389 ) ) ;
#85201 = CARTESIAN_POINT ( 'NONE',  ( 25.99240659234478557, -288.8878690167856007, -231.6357205683218865 ) ) ;
#85202 = CARTESIAN_POINT ( 'NONE',  ( 29.61062113970190168, -279.6190982408054992, -239.4476131005396837 ) ) ;
#85203 = CARTESIAN_POINT ( 'NONE',  ( -99.58389348133435703, -279.3301550459626128, -309.5349483311418339 ) ) ;
#85204 = CARTESIAN_POINT ( 'NONE',  ( 13.77886254513190778, -276.8043918556671770, -322.6300176060282183 ) ) ;
#85205 = CARTESIAN_POINT ( 'NONE',  ( -73.00270171123558782, -288.3089333092536890, -338.1718296038213225 ) ) ;
#85206 = CARTESIAN_POINT ( 'NONE',  ( -74.18954128489318123, -284.3315523653108130, -337.8474452113295570 ) ) ;
#85207 = CARTESIAN_POINT ( 'NONE',  ( -113.4275307794020762, -285.1918653366378180, -258.5871256592184864 ) ) ;
#85208 = CARTESIAN_POINT ( 'NONE',  ( 30.02067659130888444, -281.3414847057487691, -242.2308814531408245 ) ) ;
#85209 = ORIENTED_EDGE ( 'NONE', *, *, #29336, .F. ) ;
#85210 = ORIENTED_EDGE ( 'NONE', *, *, #31277, .F. ) ;
#85211 = CARTESIAN_POINT ( 'NONE',  ( 196.0143093133017658, 19.33012701892200624, -12.49999999999967315 ) ) ;
#85212 = CARTESIAN_POINT ( 'NONE',  ( -93.80682671813032414, -293.1089328461043237, -219.8438440976675281 ) ) ;
#85213 = CARTESIAN_POINT ( 'NONE',  ( -68.11494070989996885, -290.3412934247321573, -200.3018168022576333 ) ) ;
#85214 = CARTESIAN_POINT ( 'NONE',  ( -108.1645366271926605, -271.8585874837364713, -251.5245032702783021 ) ) ;
#85215 = CARTESIAN_POINT ( 'NONE',  ( 39.55438786971591014, -292.8642687002558773, -267.4487499859367290 ) ) ;
#85216 = CARTESIAN_POINT ( 'NONE',  ( -92.94751270179145308, -288.3483522770085870, -318.7975232286609071 ) ) ;
#85217 = CARTESIAN_POINT ( 'NONE',  ( 36.72188640440895568, -291.7975550469133168, -270.7878293311848665 ) ) ;
#85218 = COLOUR_RGB ( '',0.7921568627450980005, 0.8196078431372548767, 0.9333333333333333481 ) ;
#85219 = CARTESIAN_POINT ( 'NONE',  ( -26.40062462343085770, -290.1150390258587777, -342.9894628698535826 ) ) ;
#85220 = FACE_OUTER_BOUND ( 'NONE', #82022, .T. ) ;
#85221 = AXIS2_PLACEMENT_3D ( 'NONE', #64304, #20240, #70450 ) ;
#85222 = CARTESIAN_POINT ( 'NONE',  ( -109.7098821290231285, -292.8061080222270220, -250.6184949141938034 ) ) ;
#85223 = CARTESIAN_POINT ( 'NONE',  ( -111.8453999614888801, -288.6844786862233718, -260.0197317116807767 ) ) ;
#85224 = CARTESIAN_POINT ( 'NONE',  ( -104.3897491143448377, -292.9974844449021703, -236.6378879720811881 ) ) ;
#85225 = CARTESIAN_POINT ( 'NONE',  ( -39.99440614488874957, -286.9592598977974376, -197.1738813941064734 ) ) ;
#85226 = CARTESIAN_POINT ( 'NONE',  ( 30.51958622879578087, -295.1264562719712785, -237.9157287464351782 ) ) ;
#85227 = CARTESIAN_POINT ( 'NONE',  ( 199.5308170082192021, 67.35660163415921886, -10.35296668938369180 ) ) ;
#85228 = DIRECTION ( 'NONE',  ( 0.000000000000000000, 0.000000000000000000, 1.000000000000000000 ) ) ;
#85229 = TOROIDAL_SURFACE ( 'NONE', #61047, 24.00000000000002132, 2.046895004029262388 ) ;
#85230 = CARTESIAN_POINT ( 'NONE',  ( 37.67724985461494924, -277.4344160468858718, -262.7214806844898476 ) ) ;
#85231 = CARTESIAN_POINT ( 'NONE',  ( -101.4990905596771853, -295.1910754121335003, -312.7419710783055393 ) ) ;
#85232 = CARTESIAN_POINT ( 'NONE',  ( 36.38978654180912997, -273.7007394384947361, -263.3466997308307782 ) ) ;
#85233 = CARTESIAN_POINT ( 'NONE',  ( -98.07443147968626818, -276.0423527495618146, -313.4280044050193510 ) ) ;
#85234 = CARTESIAN_POINT ( 'NONE',  ( -109.9779857038130473, -273.9000898063000022, -259.4728672392996032 ) ) ;
#85235 = CARTESIAN_POINT ( 'NONE',  ( 26.44872250418129411, -273.5695005989383048, -228.2970207857106573 ) ) ;
#85236 = AXIS2_PLACEMENT_3D ( 'NONE', #89506, #24672, #54015 ) ;
#85237 = AXIS2_PLACEMENT_3D ( 'NONE', #75623, #11227, #12158 ) ;
#85238 = CARTESIAN_POINT ( 'NONE',  ( -110.6389399451682607, -298.0703472837783465, -263.2607094851260854 ) ) ;
#85239 = DIRECTION ( 'NONE',  ( 0.000000000000000000, 0.000000000000000000, -1.000000000000000000 ) ) ;
#85240 = CARTESIAN_POINT ( 'NONE',  ( -103.8696764246535480, -297.7660619708098579, -239.7985426181126911 ) ) ;
#85241 = CARTESIAN_POINT ( 'NONE',  ( -113.5000000000000568, -298.0521521680024080, -540.3336712212508246 ) ) ;
#85243 = CARTESIAN_POINT ( 'NONE',  ( -94.61138920322240153, -273.0242730988997550, -225.0932185639196064 ) ) ;
#85242 = CARTESIAN_POINT ( 'NONE',  ( 33.32080440664549315, -285.2341006420001577, -244.1844632316892785 ) ) ;
#85244 = AXIS2_PLACEMENT_3D ( 'NONE', #18858, #33997, #11279 ) ;
#85245 = CARTESIAN_POINT ( 'NONE',  ( -2.222905909516156964, -286.5039514251818105, -201.8214042656358913 ) ) ;
#85246 = CARTESIAN_POINT ( 'NONE',  ( -95.44513266483720315, -289.5361669816564358, -320.8560228644030872 ) ) ;
#85247 = CARTESIAN_POINT ( 'NONE',  ( -99.41050082484480299, -299.1087069299199470, -227.6082222131907145 ) ) ;
#85248 = CARTESIAN_POINT ( 'NONE',  ( 34.87951317196877454, -291.8051198922510139, -290.0088780720487875 ) ) ;
#85249 = CARTESIAN_POINT ( 'NONE',  ( 39.47964225627480772, -280.7081309644808016, -267.0745029167381404 ) ) ;
#85250 = CARTESIAN_POINT ( 'NONE',  ( -114.2704648735229114, -294.0523547857347353, -270.3284710469133074 ) ) ;
#85251 = DIRECTION ( 'NONE',  ( -0.000000000000000000, -1.000000000000000000, -0.000000000000000000 ) ) ;
#85252 = CARTESIAN_POINT ( 'NONE',  ( -3.195244146020708609, -287.3858593435825242, -335.3877774959526050 ) ) ;
#85253 = FACE_OUTER_BOUND ( 'NONE', #16934, .T. ) ;
#85254 = CARTESIAN_POINT ( 'NONE',  ( -2.458236550231002404, -286.5909035662497217, -336.8124834570580219 ) ) ;
#85255 = CARTESIAN_POINT ( 'NONE',  ( -110.5769288073768308, -274.1794891676080965, -262.1569097855852419 ) ) ;
#85256 = CARTESIAN_POINT ( 'NONE',  ( 12.59329519745948822, -282.1578373837249387, -212.5242566118509160 ) ) ;
#85258 = CARTESIAN_POINT ( 'NONE',  ( 20.18097106163576626, -282.1856796499242819, -315.3071111209888500 ) ) ;
#85257 = CARTESIAN_POINT ( 'NONE',  ( -112.5929422392180044, -294.5103187762870220, -275.2079067232778016 ) ) ;
#85259 = CARTESIAN_POINT ( 'NONE',  ( -114.3379842354461147, -296.7282924929146475, -269.6046537453748329 ) ) ;
#85260 = CARTESIAN_POINT ( 'NONE',  ( -96.76785638608127726, -274.5813251528768433, -226.8724341962961262 ) ) ;
#85261 = CARTESIAN_POINT ( 'NONE',  ( -7.061807674329386941, -282.4495544396286277, -201.7314135402912143 ) ) ;
#85262 = CARTESIAN_POINT ( 'NONE',  ( -68.13556585643250685, -296.6963354173360017, -203.9008431247150099 ) ) ;
#85263 = EDGE_LOOP ( 'NONE', ( #49818, #37084, #14601, #29560 ) ) ;
#85264 = CARTESIAN_POINT ( 'NONE',  ( 180.7287904564219332, 250.5000000000000568, -24.90000000000003411 ) ) ;
#85265 = CARTESIAN_POINT ( 'NONE',  ( -48.55135453237547694, -285.1754691331672689, -344.1594272355102362 ) ) ;
#85266 = CARTESIAN_POINT ( 'NONE',  ( 208.4306832106270804, -199.2391364535880882, 0.000000000000000000 ) ) ;
#85267 = CARTESIAN_POINT ( 'NONE',  ( 10.59707575819633618, -291.9094976428776818, -330.5268031993606428 ) ) ;
#85268 = CARTESIAN_POINT ( 'NONE',  ( 38.02199148988064081, -274.9370930083411508, -285.3435345675689518 ) ) ;
#85269 = CARTESIAN_POINT ( 'NONE',  ( 4.505380487589857985, -292.4674454044224490, -210.4842547104564687 ) ) ;
#85270 = CARTESIAN_POINT ( 'NONE',  ( 18.13949038304979666, -283.7577681207872047, -318.8641617330839608 ) ) ;
#85271 = CARTESIAN_POINT ( 'NONE',  ( 33.28788691199553540, -277.4330673097487079, -291.8036074388513157 ) ) ;
#85272 = CARTESIAN_POINT ( 'NONE',  ( -63.69166261321188216, -284.8143236728391230, -342.0847944742351956 ) ) ;
#85273 = CARTESIAN_POINT ( 'NONE',  ( -106.5532703262639700, -283.0219064618000857, -294.9438690124823097 ) ) ;
#85274 = CARTESIAN_POINT ( 'NONE',  ( -26.20972853582104989, -298.1879210266415612, -193.3611172013085024 ) ) ;
#85275 = CARTESIAN_POINT ( 'NONE',  ( 5.869528243787705435, -276.3170591412307999, -334.0932899766542050 ) ) ;
#85276 = CARTESIAN_POINT ( 'NONE',  ( -7.386843470316971860, -296.5764373502184981, -338.5220181679449638 ) ) ;
#85277 = DIRECTION ( 'NONE',  ( -0.000000000000000000, -1.000000000000000000, -0.000000000000000000 ) ) ;
#85278 = EDGE_CURVE ( 'NONE', #25728, #25873, #71761, .T. ) ;
#85279 = FACE_OUTER_BOUND ( 'NONE', #42103, .T. ) ;
#85280 = CARTESIAN_POINT ( 'NONE',  ( -106.6336108941719942, -295.0905608128484801, -239.5894245375911282 ) ) ;
#85281 = CARTESIAN_POINT ( 'NONE',  ( 20.06692595758643094, -275.6969610454101485, -315.5723923917195748 ) ) ;
#85282 = VECTOR ( 'NONE', #92540, 1000.000000000000000 ) ;
#85283 = CARTESIAN_POINT ( 'NONE',  ( 38.16294094168111428, -294.9285504027546381, -258.9728401621232479 ) ) ;
#85284 = CARTESIAN_POINT ( 'NONE',  ( 35.07219688184650863, -294.4388301522570828, -245.2159277609581522 ) ) ;
#85285 = CARTESIAN_POINT ( 'NONE',  ( -110.1278127687702977, -292.3285804350342119, -287.7453130306989237 ) ) ;
#85286 = CARTESIAN_POINT ( 'NONE',  ( -103.4890587661245860, -276.0870243290940493, -305.3547655319710543 ) ) ;
#85287 = AXIS2_PLACEMENT_3D ( 'NONE', #45381, #60565, #29820 ) ;
#85288 = CARTESIAN_POINT ( 'NONE',  ( -110.0178722561057612, -280.6813831034252757, -254.1940392802580106 ) ) ;
#85289 = CARTESIAN_POINT ( 'NONE',  ( -78.77108140683492365, -293.6945354681253093, -332.2693337293206355 ) ) ;
#85290 = CARTESIAN_POINT ( 'NONE',  ( 37.03749106470723973, -283.2292351932150609, -255.9374776507845581 ) ) ;
#85291 = CARTESIAN_POINT ( 'NONE',  ( -71.30928882695380366, -284.5128416489520760, -205.3962890952580551 ) ) ;
#85292 = CARTESIAN_POINT ( 'NONE',  ( -87.93210667360744992, -231.3106068285471224, -347.0561263492803619 ) ) ;
#85293 = VERTEX_POINT ( 'NONE', #55936 ) ;
#85294 = CARTESIAN_POINT ( 'NONE',  ( -109.5199196913323050, -284.0686913048139104, -281.7487380331803024 ) ) ;
#85295 = ORIENTED_EDGE ( 'NONE', *, *, #3119, .T. ) ;
#85296 = CARTESIAN_POINT ( 'NONE',  ( 39.33101504801366843, -282.5903319552435278, -267.0569256189247653 ) ) ;
#85297 = VECTOR ( 'NONE', #21195, 1000.000000000000000 ) ;
#85298 = CARTESIAN_POINT ( 'NONE',  ( -73.41240170980816515, -284.3798461233395756, -202.7234327738455306 ) ) ;
#85299 = AXIS2_PLACEMENT_3D ( 'NONE', #21379, #63100, #49329 ) ;
#85300 = CARTESIAN_POINT ( 'NONE',  ( -112.5606587759765205, -279.3003077765673083, -285.7534072906063329 ) ) ;
#85301 = CARTESIAN_POINT ( 'NONE',  ( -113.5386302917111152, -280.0206454456625238, -274.4520328841388732 ) ) ;
#85302 = CARTESIAN_POINT ( 'NONE',  ( -84.51095865778017924, -280.0735979586750659, -209.5617438996513897 ) ) ;
#85303 = CARTESIAN_POINT ( 'NONE',  ( -92.05005921254146983, -270.6952119285918457, -226.6919474004047572 ) ) ;
#85304 = CARTESIAN_POINT ( 'NONE',  ( 186.5495922466713239, 262.9189426707559960, -153.3149145016442105 ) ) ;
#85305 = VERTEX_POINT ( 'NONE', #84791 ) ;
#85306 = CARTESIAN_POINT ( 'NONE',  ( -21.57191473664897075, -276.2549749433813986, -197.2082486465691602 ) ) ;
#85307 = CARTESIAN_POINT ( 'NONE',  ( -100.3960620948416960, -247.6577473148603303, -334.0155409199911105 ) ) ;
#85308 = AXIS2_PLACEMENT_3D ( 'NONE', #21401, #14783, #58796 ) ;
#85309 = CARTESIAN_POINT ( 'NONE',  ( -60.21417990973924361, -277.7744246008469418, -199.2524386249262989 ) ) ;
#85310 = CARTESIAN_POINT ( 'NONE',  ( 37.61051428378693373, -295.4716490251918231, -282.9356773867759784 ) ) ;
#85311 = CARTESIAN_POINT ( 'NONE',  ( 35.74349899309140710, -292.9421053615432697, -273.5016115750136692 ) ) ;
#85312 = CARTESIAN_POINT ( 'NONE',  ( -97.24611791307208364, -289.4118717051399017, -318.6621994282728565 ) ) ;
#85313 = CARTESIAN_POINT ( 'NONE',  ( 196.7510731661265595, -141.7221692137691775, -22.50000000000000000 ) ) ;
#85315 = CARTESIAN_POINT ( 'NONE',  ( -95.57589920714340792, -283.5841081472163410, -225.0060873182454202 ) ) ;
#85314 = CARTESIAN_POINT ( 'NONE',  ( 19.08222239640173257, -292.8335499964741189, -321.9643450534176168 ) ) ;
#85316 = CARTESIAN_POINT ( 'NONE',  ( -60.66921659047097393, -293.6068536820058625, -199.8324090037635585 ) ) ;
#85317 = CARTESIAN_POINT ( 'NONE',  ( -97.92946719213840368, -285.2910866066442850, -312.0474536373212686 ) ) ;
#85318 = ORIENTED_EDGE ( 'NONE', *, *, #72303, .T. ) ;
#85319 = CARTESIAN_POINT ( 'NONE',  ( -42.05153703266179122, -292.9353947670043112, -193.7410315202664606 ) ) ;
#85320 = CARTESIAN_POINT ( 'NONE',  ( 21.86548535142082983, -282.6430840897753001, -313.1902230019342142 ) ) ;
#85321 = CARTESIAN_POINT ( 'NONE',  ( 17.26765468212770926, -293.0891392166258811, -324.1564427928163354 ) ) ;
#85322 = CIRCLE ( 'NONE', #88341, 2.046895004029262832 ) ;
#85323 = CARTESIAN_POINT ( 'NONE',  ( -38.90661529880382830, -289.8741459623522019, -347.1837049061523430 ) ) ;
#85324 = CARTESIAN_POINT ( 'NONE',  ( -69.32599892440725853, -289.9541410488120050, -340.3507502568501195 ) ) ;
#85325 = CARTESIAN_POINT ( 'NONE',  ( 33.02870052079136798, -287.4622644176563995, -250.9444571718619272 ) ) ;
#85326 = ORIENTED_EDGE ( 'NONE', *, *, #34702, .T. ) ;
#85327 = CARTESIAN_POINT ( 'NONE',  ( 208.4306832106270804, -148.7221692137691491, 0.000000000000000000 ) ) ;
#85328 = CARTESIAN_POINT ( 'NONE',  ( -97.83368150893323900, -295.8665948216546440, -223.4996305552631384 ) ) ;
#85329 = CARTESIAN_POINT ( 'NONE',  ( 33.34382439534415710, -280.3580891893270177, -251.1567770347494672 ) ) ;
#85330 = CARTESIAN_POINT ( 'NONE',  ( -64.87220129343742769, -273.2097151345325869, -198.5026791848366656 ) ) ;
#85331 = CARTESIAN_POINT ( 'NONE',  ( -18.05753358120802687, -293.2788770718879050, -341.4865611886954753 ) ) ;
#85332 = CARTESIAN_POINT ( 'NONE',  ( 36.02203325793278310, -277.1849917597225499, -260.5766079305047924 ) ) ;
#85333 = CARTESIAN_POINT ( 'NONE',  ( -39.17121545107871583, -296.2687728475834206, -196.3578148628117788 ) ) ;
#85334 = CARTESIAN_POINT ( 'NONE',  ( -9.063793263993545679, -295.8790172259487576, -338.1058149697218482 ) ) ;
#85335 = CARTESIAN_POINT ( 'NONE',  ( -63.66720964127983962, -296.4831069969220039, -338.8341469933401982 ) ) ;
#85336 = DIRECTION ( 'NONE',  ( -1.000000000000000000, -0.000000000000000000, 0.000000000000000000 ) ) ;
#85337 = CARTESIAN_POINT ( 'NONE',  ( -90.14289132493765067, -297.3833651113022256, -325.3743899141696829 ) ) ;
#85338 = CARTESIAN_POINT ( 'NONE',  ( -107.1756566770312702, -294.9149607304752863, -242.4140483279979037 ) ) ;
#85339 = CARTESIAN_POINT ( 'NONE',  ( -17.41276450388166808, -292.9674788075290621, -199.9754590976942552 ) ) ;
#85340 = CARTESIAN_POINT ( 'NONE',  ( -14.85548855148504188, -298.9781657277604268, -193.4606360843729647 ) ) ;
#85341 = CARTESIAN_POINT ( 'NONE',  ( -107.5194736246562570, -288.8336646049432943, -292.6760122069681529 ) ) ;
#85342 = CARTESIAN_POINT ( 'NONE',  ( -43.67574994848473580, -275.9724079498772653, -195.5769595042413584 ) ) ;
#85343 = CARTESIAN_POINT ( 'NONE',  ( -114.2803945993239978, -273.0802817338963564, -267.5021993077760953 ) ) ;
#85344 = ADVANCED_FACE ( 'NONE', ( #40287 ), #68697, .T. ) ;
#85345 = CARTESIAN_POINT ( 'NONE',  ( -94.78744396980151521, -296.2499511348794954, -315.4396494731284974 ) ) ;
#85346 = ADVANCED_FACE ( 'NONE', ( #69204 ), #5751, .F. ) ;
#85347 = CARTESIAN_POINT ( 'NONE',  ( -64.18059975866478339, -281.6837639149981101, -199.8924440197786225 ) ) ;
#85348 = CARTESIAN_POINT ( 'NONE',  ( 25.88259953915978784, -279.6640866499496383, -227.1874935540791682 ) ) ;
#85349 = CARTESIAN_POINT ( 'NONE',  ( 15.67724591466546791, -281.6736722920717853, -326.0594496172246863 ) ) ;
#85350 = CARTESIAN_POINT ( 'NONE',  ( 10.45620175047695177, -275.7607702168896822, -330.6675780036783294 ) ) ;
#85351 = CARTESIAN_POINT ( 'NONE',  ( 20.47257553036742195, -279.2748433380169786, -220.7030801668565516 ) ) ;
#85352 = CARTESIAN_POINT ( 'NONE',  ( 36.34319700263598207, -279.7422620152529475, -285.2125275018509569 ) ) ;
#85353 = CARTESIAN_POINT ( 'NONE',  ( 7.705813286384870509, -273.2558397446632057, -212.1709431193758917 ) ) ;
#85354 = CARTESIAN_POINT ( 'NONE',  ( -46.01798673481732749, -279.1622160332308908, -344.9091645557127208 ) ) ;
#85355 = LINE ( 'NONE', #1386, #12566 ) ;
#85356 = CARTESIAN_POINT ( 'NONE',  ( -74.94434090351494149, -282.8906705383787994, 74.50000000000001421 ) ) ;
#85357 = CARTESIAN_POINT ( 'NONE',  ( -97.41883034708538958, -295.4216997323484293, -223.8136569756578638 ) ) ;
#85358 = CARTESIAN_POINT ( 'NONE',  ( -11.68895326348806485, -290.4045086914899798, -199.4518877087343185 ) ) ;
#85359 = CARTESIAN_POINT ( 'NONE',  ( -33.53936521356042277, -292.0987747743462819, -193.4550567832122852 ) ) ;
#85360 = CARTESIAN_POINT ( 'NONE',  ( 37.72185028693903774, -277.4904424940166336, -265.5315688099045701 ) ) ;
#85361 = CARTESIAN_POINT ( 'NONE',  ( 1.674055110504922395, -272.5737339518336171, -206.3082375524538179 ) ) ;
#85362 = DIRECTION ( 'NONE',  ( 0.000000000000000000, 1.000000000000000000, 9.656854691831248164E-17 ) ) ;
#85363 = CARTESIAN_POINT ( 'NONE',  ( 35.10516137891819710, -283.7488129434112807, -292.0067881129322700 ) ) ;
#85364 = DIRECTION ( 'NONE',  ( -1.000000000000000000, 0.000000000000000000, 0.000000000000000000 ) ) ;
#85365 = CARTESIAN_POINT ( 'NONE',  ( -111.0247452101357908, -282.7325274017208585, -256.3006823243030112 ) ) ;
#85366 = CARTESIAN_POINT ( 'NONE',  ( 196.8702642586143270, 40.96915988761478644, 12.42857142857141994 ) ) ;
#85367 = CARTESIAN_POINT ( 'NONE',  ( -6.612568104887075471, -293.4343224025716950, -337.0158323780170804 ) ) ;
#85368 = CARTESIAN_POINT ( 'NONE',  ( 33.01875402797421089, -285.3825332752226132, -246.6910531174620473 ) ) ;
#85369 = DIRECTION ( 'NONE',  ( 0.000000000000000000, 1.000000000000000000, 0.000000000000000000 ) ) ;
#85370 = CARTESIAN_POINT ( 'NONE',  ( -7.207478984242021269, -292.6567565507618838, -339.0549699003111073 ) ) ;
#85371 = CARTESIAN_POINT ( 'NONE',  ( -61.03494739089646970, -281.8339807779076409, -342.9513861241897530 ) ) ;
#85372 = CARTESIAN_POINT ( 'NONE',  ( -39.74750515157573005, -281.6216008673962961, -196.5876821948639304 ) ) ;
#85373 = CARTESIAN_POINT ( 'NONE',  ( -106.3282113879519244, -286.1866761557398036, -237.0614185597411563 ) ) ;
#85374 = CARTESIAN_POINT ( 'NONE',  ( 31.11837850745464351, -279.3620110375047147, -237.2674021643780122 ) ) ;
#85375 = CARTESIAN_POINT ( 'NONE',  ( -4.594561174994372443, -286.4961386153739227, -205.1183031261544443 ) ) ;
#85376 = AXIS2_PLACEMENT_3D ( 'NONE', #40785, #31854, #46049 ) ;
#85377 = CARTESIAN_POINT ( 'NONE',  ( -110.9410942854753586, -280.0095523428630599, -267.9065712911786932 ) ) ;
#85378 = CARTESIAN_POINT ( 'NONE',  ( -106.6008990167036359, -279.6694388792457744, -246.6308072624681245 ) ) ;
#85379 = CARTESIAN_POINT ( 'NONE',  ( -84.50354520639299949, -287.3862664607104307, -211.5889547711989280 ) ) ;
#85380 = ORIENTED_EDGE ( 'NONE', *, *, #46511, .F. ) ;
#85381 = CARTESIAN_POINT ( 'NONE',  ( -97.34501241894210466, -297.0321885429960957, -222.1055222587203275 ) ) ;
#85382 = CARTESIAN_POINT ( 'NONE',  ( -53.74600324994583644, -291.2436144459783236, -343.1810715573777202 ) ) ;
#85383 = LINE ( 'NONE', #11060, #66643 ) ;
#85384 = CARTESIAN_POINT ( 'NONE',  ( 36.60358173371528068, -290.4805209788416391, -305.9350535429201159 ) ) ;
#85385 = ORIENTED_EDGE ( 'NONE', *, *, #20244, .F. ) ;
#85386 = CARTESIAN_POINT ( 'NONE',  ( -29.99218240839089233, -272.1448144039434851, -195.5546141523136043 ) ) ;
#85387 = CARTESIAN_POINT ( 'NONE',  ( 38.91108047583755081, -291.9516414418151271, -270.3308287414987490 ) ) ;
#85388 = CARTESIAN_POINT ( 'NONE',  ( -69.27878068144187296, -297.1278496948397105, -204.6495411668220754 ) ) ;
#85389 = CARTESIAN_POINT ( 'NONE',  ( -10.45325000053184006, -290.2151086143339853, -339.0286747491756500 ) ) ;
#85390 = AXIS2_PLACEMENT_3D ( 'NONE', #84683, #68634, #11330 ) ;
#85391 = CARTESIAN_POINT ( 'NONE',  ( -30.18642673180180580, -281.9039182815166669, -196.6434089596836827 ) ) ;
#85392 = CARTESIAN_POINT ( 'NONE',  ( -72.88356861356207617, -290.9388561554251851, -338.0173291965904241 ) ) ;
#85393 = CARTESIAN_POINT ( 'NONE',  ( -112.3810011312560704, -291.6787743110392626, -285.3405846625454956 ) ) ;
#85394 = CARTESIAN_POINT ( 'NONE',  ( -75.76605108457408733, -287.5393609507518136, -205.9517250169661224 ) ) ;
#85395 = CARTESIAN_POINT ( 'NONE',  ( -71.23650637898326465, -279.7836696436721127, -201.2225461593754687 ) ) ;
#85396 = CARTESIAN_POINT ( 'NONE',  ( -19.64864832398396643, -292.9063518290886350, -343.8742824224568153 ) ) ;
#85397 = CARTESIAN_POINT ( 'NONE',  ( 38.79505494141974964, -281.2373538934267572, -258.5176527606635091 ) ) ;
#85398 = CARTESIAN_POINT ( 'NONE',  ( 36.33497591933855375, -277.5358108856356125, -279.8612989999423917 ) ) ;
#85399 = CARTESIAN_POINT ( 'NONE',  ( 34.45848030099739390, -278.0519495502701375, -270.3284710469131937 ) ) ;
#85400 = CARTESIAN_POINT ( 'NONE',  ( 37.18408174626422635, -273.9799391725375699, -285.1895316596790053 ) ) ;
#85401 = CARTESIAN_POINT ( 'NONE',  ( 152.4536156746142410, 275.5000000000000568, 12.49999999999999289 ) ) ;
#85402 = CARTESIAN_POINT ( 'NONE',  ( 30.08069009637267399, -280.6825635611310190, -242.2148973141834460 ) ) ;
#85403 = CARTESIAN_POINT ( 'NONE',  ( -110.2838281678035912, -279.4595696811803691, -293.9295440567838114 ) ) ;
#85404 = CARTESIAN_POINT ( 'NONE',  ( -24.52679693562780017, -275.5341701822347886, -197.9419132277197662 ) ) ;
#85405 = CARTESIAN_POINT ( 'NONE',  ( -114.0908887220844150, -283.6516562711590836, -267.1123721748851949 ) ) ;
#85406 = CARTESIAN_POINT ( 'NONE',  ( -106.6675788237325548, -292.6550733738876033, -244.2946033630293527 ) ) ;
#85407 = CARTESIAN_POINT ( 'NONE',  ( -32.75137001562904970, -275.7091857408825604, -194.2864888338620517 ) ) ;
#85408 = CARTESIAN_POINT ( 'NONE',  ( -108.7126526473435035, -274.2203027110222138, -242.6564437103182854 ) ) ;
#85409 = CARTESIAN_POINT ( 'NONE',  ( 165.2494399300530290, -11.64849832608277325, 10.00000000000000000 ) ) ;
#85410 = CARTESIAN_POINT ( 'NONE',  ( -110.2692839601484565, -298.7682539721303101, -253.5802971519963194 ) ) ;
#85411 = CARTESIAN_POINT ( 'NONE',  ( -72.28702149830643009, -281.5155043557019212, -336.5340198642109613 ) ) ;
#85412 = CARTESIAN_POINT ( 'NONE',  ( -86.49626782610978637, -291.0578643194762662, -211.0502616425293638 ) ) ;
#85413 = CARTESIAN_POINT ( 'NONE',  ( 30.64214181755867017, -273.9785493321141985, -301.1839023142103429 ) ) ;
#85414 = CARTESIAN_POINT ( 'NONE',  ( 5.128514372995561565, -290.0883040165365969, -333.6281812478321740 ) ) ;
#85415 = CARTESIAN_POINT ( 'NONE',  ( -108.0275319073851392, -289.2145424529018101, -289.9838342090316701 ) ) ;
#85416 = ORIENTED_EDGE ( 'NONE', *, *, #50473, .T. ) ;
#85417 = CARTESIAN_POINT ( 'NONE',  ( -110.6616201043788408, -289.3988017178612608, -248.8484327011938717 ) ) ;
#85418 = CARTESIAN_POINT ( 'NONE',  ( -88.67894768929343741, -289.4640659242472793, -322.2896698550895280 ) ) ;
#85419 = ORIENTED_EDGE ( 'NONE', *, *, #35340, .F. ) ;
#85420 = CARTESIAN_POINT ( 'NONE',  ( 1.353790694844288822, -287.6360598240672175, -204.1329171591973761 ) ) ;
#85421 = CARTESIAN_POINT ( 'NONE',  ( -104.2890772281016325, -278.4919913213654468, -299.6448968440159888 ) ) ;
#85422 = CARTESIAN_POINT ( 'NONE',  ( -27.79998188165951589, -293.8541569591969846, -346.5091900082400116 ) ) ;
#85423 = CARTESIAN_POINT ( 'NONE',  ( -108.1300546628084192, -284.8191650665347083, -300.5359739669268038 ) ) ;
#85424 = CARTESIAN_POINT ( 'NONE',  ( -95.80328488195675618, -285.5620326133076787, -220.2013545995151560 ) ) ;
#85425 = CARTESIAN_POINT ( 'NONE',  ( 29.33549912996144116, -282.2876754222617706, -300.2550449009398221 ) ) ;
#85426 = CARTESIAN_POINT ( 'NONE',  ( 103.2429438805325930, 116.4356071745880996, -282.9982326746781496 ) ) ;
#85427 = CARTESIAN_POINT ( 'NONE',  ( -113.0914918815083325, -269.8132127191667564, -296.0580370876392067 ) ) ;
#85428 = CARTESIAN_POINT ( 'NONE',  ( 137.7094901139326737, 178.8809403604650754, -238.3456290536556423 ) ) ;
#85429 = CARTESIAN_POINT ( 'NONE',  ( 35.86023183603892761, -274.7655933550383907, -271.5978758200953962 ) ) ;
#85430 = CARTESIAN_POINT ( 'NONE',  ( -5.160002530986704805, -273.4063308220990507, -204.4794539677491514 ) ) ;
#85431 = CARTESIAN_POINT ( 'NONE',  ( -96.46815393572545361, -295.3969160455825431, -319.6115696248878066 ) ) ;
#85432 = CARTESIAN_POINT ( 'NONE',  ( -29.67131002704720188, -125.4300734434975766, -360.8905850898509584 ) ) ;
#85433 = CARTESIAN_POINT ( 'NONE',  ( -2.765335570163358181, -273.1843892286717619, -202.0986268218431405 ) ) ;
#85434 = CARTESIAN_POINT ( 'NONE',  ( -78.21144900091205443, -299.3569442172352524, -208.3273320104813138 ) ) ;
#85435 = CARTESIAN_POINT ( 'NONE',  ( -64.19759731154091753, -292.7730358496651775, -202.1347207499361218 ) ) ;
#85436 = VERTEX_POINT ( 'NONE', #34162 ) ;
#85437 = CARTESIAN_POINT ( 'NONE',  ( -80.50266295016409401, -298.4242525308100653, -206.8153012810754490 ) ) ;
#85438 = CARTESIAN_POINT ( 'NONE',  ( 35.18605994602095421, -288.1606946722600355, -279.1765850866558480 ) ) ;
#85439 = CARTESIAN_POINT ( 'NONE',  ( 37.60153573046810038, -294.1417491567841580, -253.3413171082922304 ) ) ;
#85440 = CARTESIAN_POINT ( 'NONE',  ( -41.93561398675245755, -295.6007914749510519, -347.2146602143050700 ) ) ;
#85441 = CARTESIAN_POINT ( 'NONE',  ( 34.83830210746106815, -293.8671038216530178, -281.6008562030149847 ) ) ;
#85442 = ORIENTED_EDGE ( 'NONE', *, *, #87369, .F. ) ;
#85443 = CIRCLE ( 'NONE', #23396, 0.5000000000000004441 ) ;
#85444 = CARTESIAN_POINT ( 'NONE',  ( 24.94344187158408488, -276.8966981663572824, -227.5611537256123995 ) ) ;
#85445 = VERTEX_POINT ( 'NONE', #4333 ) ;
#85446 = CARTESIAN_POINT ( 'NONE',  ( -77.45507643787013308, -279.0372459774230265, -204.6454729271333974 ) ) ;
#85447 = UNCERTAINTY_MEASURE_WITH_UNIT (LENGTH_MEASURE( 1.000000000000000082E-05 ), #20907, 'distance_accuracy_value', 'NONE');
#85448 = CARTESIAN_POINT ( 'NONE',  ( -11.41811196136254303, -275.3394539857553696, -201.8132811880556403 ) ) ;
#85449 = CARTESIAN_POINT ( 'NONE',  ( 38.54093798138981697, -277.2504618690291522, -265.4822052030980899 ) ) ;
#85450 = CARTESIAN_POINT ( 'NONE',  ( -61.89442254362924700, -275.3896969983617851, -341.6592695692138477 ) ) ;
#85451 = CARTESIAN_POINT ( 'NONE',  ( -98.53744200381302676, -297.7580489460414697, -230.2823291423905800 ) ) ;
#85452 = CARTESIAN_POINT ( 'NONE',  ( -104.4815924179346212, -294.7228439471268757, -300.6123129739608544 ) ) ;
#85453 = LINE ( 'NONE', #4976, #53238 ) ;
#85454 = CARTESIAN_POINT ( 'NONE',  ( -100.2023290044299557, -279.6319692578316563, -225.9982028329368404 ) ) ;
#85455 = EDGE_CURVE ( 'NONE', #82501, #38497, #39938, .T. ) ;
#85456 = CARTESIAN_POINT ( 'NONE',  ( 22.46705677812836655, -276.3035800437105536, -312.3037599124360781 ) ) ;
#85457 = CARTESIAN_POINT ( 'NONE',  ( 11.77389624498925258, -285.4022830271741213, -211.6323089209319619 ) ) ;
#85458 = CARTESIAN_POINT ( 'NONE',  ( -35.55276828753007834, -300.0746522698417493, -195.1938344133556313 ) ) ;
#85459 = CARTESIAN_POINT ( 'NONE',  ( 160.5350683151633291, 275.5000000000000568, 20.22542485937379908 ) ) ;
#85460 = CARTESIAN_POINT ( 'NONE',  ( 30.11461380323548198, -286.3685355557229855, -241.9059047431724423 ) ) ;
#85461 = CARTESIAN_POINT ( 'NONE',  ( -46.56075853841169021, -278.1735434440051904, -196.8723759676163354 ) ) ;
#85463 = CARTESIAN_POINT ( 'NONE',  ( -74.53711531305629023, -281.6304886815091777, -334.9009908338637160 ) ) ;
#85462 = CARTESIAN_POINT ( 'NONE',  ( -109.7082703757403976, -277.3016884326154923, -257.0024343338664607 ) ) ;
#85464 = CARTESIAN_POINT ( 'NONE',  ( 17.01494065473467998, -288.8269988651681501, -218.6671186982148640 ) ) ;
#85465 = CARTESIAN_POINT ( 'NONE',  ( -40.50761639806828640, -278.2978907447136976, -343.7024132494160540 ) ) ;
#85466 = CARTESIAN_POINT ( 'NONE',  ( 183.0442525570908288, 293.9636489450775230, 0.000000000000000000 ) ) ;
#85467 = CARTESIAN_POINT ( 'NONE',  ( -107.7263555860935611, -276.4235023735220125, -298.9963111501773483 ) ) ;
#85468 = CARTESIAN_POINT ( 'NONE',  ( -0.5020590240191551423, -275.2071284404660787, -207.2059222955260509 ) ) ;
#85469 = CARTESIAN_POINT ( 'NONE',  ( 24.75141919173618277, -282.9788861606731984, -227.9091212399665096 ) ) ;
#85470 = FACE_OUTER_BOUND ( 'NONE', #41722, .T. ) ;
#85471 = CARTESIAN_POINT ( 'NONE',  ( -7.466347824704368641, -290.5836748055257317, -339.7781022376486249 ) ) ;
#85472 = CARTESIAN_POINT ( 'NONE',  ( -107.1503436277639310, -294.9104573035562566, -242.8028733357952831 ) ) ;
#85473 = CARTESIAN_POINT ( 'NONE',  ( 82.15976772225275226, -298.6975972703625644, -197.1770246269288691 ) ) ;
#85474 = CARTESIAN_POINT ( 'NONE',  ( 20.25235203416342955, -273.5967206732531167, -224.6882792085102949 ) ) ;
#85475 = CARTESIAN_POINT ( 'NONE',  ( 19.43636954527508465, -291.0236384560634519, -222.5373133760767814 ) ) ;
#85476 = CARTESIAN_POINT ( 'NONE',  ( 88.37812178648184158, 82.46720509654242903, -304.8213980281626618 ) ) ;
#85477 = CARTESIAN_POINT ( 'NONE',  ( 197.3290507633359709, 70.40097505901294994, -11.81033421933028649 ) ) ;
#85478 = CARTESIAN_POINT ( 'NONE',  ( -105.8991785296611141, -288.5965288166284495, -303.9862092998071148 ) ) ;
#85479 = CARTESIAN_POINT ( 'NONE',  ( -103.7234390054959192, -285.7190485944348666, -302.7259751915948982 ) ) ;
#85480 = CARTESIAN_POINT ( 'NONE',  ( 29.25440886013337050, -285.3105775831259052, -233.6604594917863551 ) ) ;
#85481 = CARTESIAN_POINT ( 'NONE',  ( -110.0779476705021978, -285.8269609341642195, -281.8595101528047735 ) ) ;
#85482 = CARTESIAN_POINT ( 'NONE',  ( -109.3537821472749556, -285.5259432252710212, -257.3730876721704135 ) ) ;
#85483 = CARTESIAN_POINT ( 'NONE',  ( -53.07113772343158331, -293.8315063285199358, -196.6125193458454703 ) ) ;
#85484 = CARTESIAN_POINT ( 'NONE',  ( 32.83754504310024203, -273.9956657480891522, -298.5054196352234044 ) ) ;
#85485 = CARTESIAN_POINT ( 'NONE',  ( 39.35979346878447416, -275.9671065084103816, -276.8899135430260685 ) ) ;
#85486 = CARTESIAN_POINT ( 'NONE',  ( -112.9276973838095159, -288.6573999724478767, -268.3678348825804960 ) ) ;
#85487 = CARTESIAN_POINT ( 'NONE',  ( -84.86637858723672423, -277.6867629155370309, -331.0127353505313863 ) ) ;
#85488 = CARTESIAN_POINT ( 'NONE',  ( -110.3939595230142743, -298.7306801683519097, -254.9628638157828107 ) ) ;
#85489 = DIRECTION ( 'NONE',  ( 0.000000000000000000, 1.000000000000000000, 0.000000000000000000 ) ) ;
#85490 = FACE_OUTER_BOUND ( 'NONE', #92730, .T. ) ;
#85491 = CARTESIAN_POINT ( 'NONE',  ( -88.02255192507298887, -284.0097323557801019, -217.1380521336927529 ) ) ;
#85492 = CARTESIAN_POINT ( 'NONE',  ( -22.92500629182146454, -278.2362999985753049, -196.7069129976315196 ) ) ;
#85493 = DIRECTION ( 'NONE',  ( 0.000000000000000000, 1.000000000000000000, -0.000000000000000000 ) ) ;
#85494 = CARTESIAN_POINT ( 'NONE',  ( 23.93477325718336601, -273.4219383265481724, -224.8869322975220086 ) ) ;
#85495 = CARTESIAN_POINT ( 'NONE',  ( -74.07165735627216918, -276.9027617096418226, -333.5655712296564843 ) ) ;
#85496 = CARTESIAN_POINT ( 'NONE',  ( -50.57690759279955017, -296.7443813451467918, -342.8562008094031057 ) ) ;
#85497 = CARTESIAN_POINT ( 'NONE',  ( 37.56064306032777722, -280.6800082276840271, -286.8877868902635555 ) ) ;
#85498 = CARTESIAN_POINT ( 'NONE',  ( -31.57189788777413497, -295.9189228475019036, -343.4190485551495726 ) ) ;
#85499 = CARTESIAN_POINT ( 'NONE',  ( -61.42036995063765659, -296.6735375929934548, -343.0354728500914234 ) ) ;
#85500 = CARTESIAN_POINT ( 'NONE',  ( -109.6030553722883809, -272.3619811233771202, -259.5093225255930633 ) ) ;
#85501 = CARTESIAN_POINT ( 'NONE',  ( -85.12225379204525666, -293.3926104201368048, -212.5509170035166164 ) ) ;
#85502 = CARTESIAN_POINT ( 'NONE',  ( -113.8198857466201162, -284.8307530452827905, -261.4119767391071036 ) ) ;
#85503 = CARTESIAN_POINT ( 'NONE',  ( -43.91165069348464556, -272.1096668562589116, -194.8292561368286044 ) ) ;
#85504 = CARTESIAN_POINT ( 'NONE',  ( 37.37734162407514305, -287.1527367308601697, -251.7583008795115234 ) ) ;
#85505 = CARTESIAN_POINT ( 'NONE',  ( -43.92062934987458078, -281.9486143028269112, -195.9554349219983749 ) ) ;
#85506 = CARTESIAN_POINT ( 'NONE',  ( -19.74775943112968690, -285.3427172996281342, -199.2706003438800906 ) ) ;
#85507 = CARTESIAN_POINT ( 'NONE',  ( -41.67124161301421026, -287.1065093832526713, -345.2489305224974601 ) ) ;
#85508 = CARTESIAN_POINT ( 'NONE',  ( -106.3535322092011199, -272.9508360837029954, -295.9465859460973434 ) ) ;
#85509 = CARTESIAN_POINT ( 'NONE',  ( 25.00649936477236679, -286.5354849934403205, -232.2731873275983219 ) ) ;
#85510 = CARTESIAN_POINT ( 'NONE',  ( 28.11067463113290543, -283.0201968156267185, -310.5718127627725380 ) ) ;
#85511 = CARTESIAN_POINT ( 'NONE',  ( -113.7713662134438977, -289.7076530896669624, -262.6486439669167794 ) ) ;
#85512 = CARTESIAN_POINT ( 'NONE',  ( -99.60716562036697042, -280.7395715522028468, -226.4355875573334629 ) ) ;
#85513 = CARTESIAN_POINT ( 'NONE',  ( -86.50075231068633741, -280.7013072837039545, -211.6687999738819315 ) ) ;
#85514 = CARTESIAN_POINT ( 'NONE',  ( 31.07104722411070341, -281.0440341837937126, -244.7465731184199740 ) ) ;
#85515 = CARTESIAN_POINT ( 'NONE',  ( 36.33353319184841723, -277.3721129037020319, -256.3268511106654159 ) ) ;
#85516 = CARTESIAN_POINT ( 'NONE',  ( -4.502533278418947127, -294.6313252199440171, -340.0217587359314280 ) ) ;
#85517 = CARTESIAN_POINT ( 'NONE',  ( -87.86071224173032590, -287.7820920545598824, -325.3828414447040132 ) ) ;
#85518 = CIRCLE ( 'NONE', #35651, 1.000000000000000888 ) ;
#85519 = CARTESIAN_POINT ( 'NONE',  ( -96.34094964446404674, -296.0800069474249767, -226.8276945445428225 ) ) ;
#85520 = VERTEX_POINT ( 'NONE', #62104 ) ;
#85521 = CARTESIAN_POINT ( 'NONE',  ( 34.72362051837087904, -283.7143713935473102, -289.0641358370465923 ) ) ;
#85522 = CARTESIAN_POINT ( 'NONE',  ( -67.30776643810303028, -295.1229841594759478, -336.9640344876455060 ) ) ;
#85523 = CARTESIAN_POINT ( 'NONE',  ( 17.25982963123163216, -293.8885137752931769, -216.4331697621240380 ) ) ;
#85524 = CARTESIAN_POINT ( 'NONE',  ( -71.44909830719414856, -284.1666494155278428, -335.0185077991605453 ) ) ;
#85525 = CARTESIAN_POINT ( 'NONE',  ( -21.39194517359764092, -273.3106466430626824, -195.2716677969644365 ) ) ;
#85526 = CARTESIAN_POINT ( 'NONE',  ( -40.32648608736790408, -289.7401286725425393, -347.2143011431266473 ) ) ;
#85527 = CARTESIAN_POINT ( 'NONE',  ( -110.3083884012011282, -282.4319497071741694, -290.7613112288343018 ) ) ;
#85528 = CARTESIAN_POINT ( 'NONE',  ( 21.19297770640138268, -288.4980240389705841, -314.0372790511082144 ) ) ;
#85529 = CARTESIAN_POINT ( 'NONE',  ( 197.1396238179664806, 70.11630495483946390, 10.20652033329685793 ) ) ;
#85530 = LINE ( 'NONE', #55727, #79384 ) ;
#85531 = CARTESIAN_POINT ( 'NONE',  ( 179.3481683450128799, 251.2162237358350296, -164.2031354143598492 ) ) ;
#85532 = CARTESIAN_POINT ( 'NONE',  ( -37.30987171927208834, -283.5523547857346784, -195.3611179825600175 ) ) ;
#85533 = ORIENTED_EDGE ( 'NONE', *, *, #2712, .F. ) ;
#85534 = CARTESIAN_POINT ( 'NONE',  ( -98.24276597247360598, -278.0379758613937611, -229.4630841282810536 ) ) ;
#85535 = CARTESIAN_POINT ( 'NONE',  ( 39.11606743151551768, -275.3363193404978233, -279.7495316287636911 ) ) ;
#85536 = CARTESIAN_POINT ( 'NONE',  ( -109.9447275254303094, -280.3182582703445860, -288.5475079289647624 ) ) ;
#85537 = CARTESIAN_POINT ( 'NONE',  ( 27.23156886404066057, -24.64972949587738782, -342.7637830639515073 ) ) ;
#85538 = CARTESIAN_POINT ( 'NONE',  ( 22.42587235992054318, -279.4844028041153479, -222.7331297969963089 ) ) ;
#85539 = CARTESIAN_POINT ( 'NONE',  ( -100.4344906291615729, -282.0320756914086360, -310.3471119873251496 ) ) ;
#85540 = CARTESIAN_POINT ( 'NONE',  ( -100.7698843629572139, -297.7536358669563583, -312.2992698669916081 ) ) ;
#85541 = CARTESIAN_POINT ( 'NONE',  ( 30.88361845728635302, -293.6956813646223736, -244.2212184902696492 ) ) ;
#85542 = ORIENTED_EDGE ( 'NONE', *, *, #9353, .T. ) ;
#85543 = CARTESIAN_POINT ( 'NONE',  ( -108.9038523491274759, -289.4569924473643709, -253.5700453439344528 ) ) ;
#85544 = CARTESIAN_POINT ( 'NONE',  ( 26.05582569661106973, -275.6281620950620663, -226.8169079915260795 ) ) ;
#85545 = CARTESIAN_POINT ( 'NONE',  ( 8.926447763647503919, -298.8139247038343456, -197.3597661904372558 ) ) ;
#85546 = EDGE_LOOP ( 'NONE', ( #64362, #68160, #50638, #90523 ) ) ;
#85547 = CARTESIAN_POINT ( 'NONE',  ( 208.6208076322478746, 32.98517505407394168, 10.00000000000000000 ) ) ;
#85548 = CARTESIAN_POINT ( 'NONE',  ( 222.8344101925596306, -44.55766379199612004, -21.50000000000000000 ) ) ;
#85549 = ADVANCED_FACE ( 'NONE', ( #56418 ), #84323, .F. ) ;
#85550 = DIRECTION ( 'NONE',  ( -1.000000000000000000, 0.000000000000000000, 0.000000000000000000 ) ) ;
#85551 = CARTESIAN_POINT ( 'NONE',  ( -57.21013760975414897, -280.8693607649280466, -199.7957492467839131 ) ) ;
#85552 = CARTESIAN_POINT ( 'NONE',  ( -33.98279256658350533, -281.8539990600738179, -194.4487227149543855 ) ) ;
#85553 = CARTESIAN_POINT ( 'NONE',  ( 35.54251501220352338, -283.2288194300687110, -256.1961503749483313 ) ) ;
#85554 = CARTESIAN_POINT ( 'NONE',  ( 28.48924969137261698, -273.5867518456990410, -237.2402213100553467 ) ) ;
#85555 = DIRECTION ( 'NONE',  ( -1.000000000000000000, 0.000000000000000000, 0.000000000000000000 ) ) ;
#85556 = DIRECTION ( 'NONE',  ( -0.000000000000000000, -1.000000000000000000, -0.000000000000000000 ) ) ;
#85557 = CARTESIAN_POINT ( 'NONE',  ( -109.5814440185550040, -279.0218213547810251, -296.7002583133177041 ) ) ;
#85558 = VERTEX_POINT ( 'NONE', #26101 ) ;
#85559 = ORIENTED_EDGE ( 'NONE', *, *, #21626, .T. ) ;
#85560 = CARTESIAN_POINT ( 'NONE',  ( 209.5647629949351654, 27.95999215251566028, 12.09245862095555424 ) ) ;
#85561 = CARTESIAN_POINT ( 'NONE',  ( -55.28555507663003254, -285.2617727398736633, -343.5487184990271317 ) ) ;
#85562 = CARTESIAN_POINT ( 'NONE',  ( 30.73206060456390531, -293.1086534307085572, -297.3057385194401263 ) ) ;
#85563 = ADVANCED_FACE ( 'NONE', ( #90936 ), #18533, .T. ) ;
#85564 = CARTESIAN_POINT ( 'NONE',  ( 20.49075617362565538, -287.5875370793182810, -321.0634918141067828 ) ) ;
#85565 = CARTESIAN_POINT ( 'NONE',  ( -110.4181088180543640, -282.9457908777168313, -258.5416320282533889 ) ) ;
#85567 = CARTESIAN_POINT ( 'NONE',  ( -48.23192545448974045, -287.4323272021493949, -343.6206156817993929 ) ) ;
#85566 = CARTESIAN_POINT ( 'NONE',  ( -100.1024354129055638, -283.6532775940405031, -231.8392706211699590 ) ) ;
#85568 = CARTESIAN_POINT ( 'NONE',  ( -38.87808651764148493, -284.2768934544958483, -343.7546692422877754 ) ) ;
#85569 = CARTESIAN_POINT ( 'NONE',  ( -21.74517891133420733, -272.2519085594715875, -197.0007119613921418 ) ) ;
#85570 = CARTESIAN_POINT ( 'NONE',  ( -113.3522103628082363, -283.0287314509279781, -264.2914591081551521 ) ) ;
#85571 = CARTESIAN_POINT ( 'NONE',  ( -98.36594887961382483, -297.9583063311339970, -314.0494907112497458 ) ) ;
#85572 = CARTESIAN_POINT ( 'NONE',  ( -36.55832833323467668, -284.0618060758968682, -195.1858001347452785 ) ) ;
#85573 = CARTESIAN_POINT ( 'NONE',  ( -109.1202495476264431, -279.6853521515758416, -255.7637111016307756 ) ) ;
#85574 = CARTESIAN_POINT ( 'NONE',  ( 15.00377397118206524, -288.7885883970969871, -216.4168896881612341 ) ) ;
#85575 = CARTESIAN_POINT ( 'NONE',  ( 207.6662022560301182, 36.29800326561209545, 14.90057469441957316 ) ) ;
#85576 = CARTESIAN_POINT ( 'NONE',  ( 5.656338806266730579, -294.5498868644410777, -208.2283340149834601 ) ) ;
#85577 = CIRCLE ( 'NONE', #50853, 0.5000000000000004441 ) ;
#85578 = CARTESIAN_POINT ( 'NONE',  ( -111.2615091041748627, -276.3881652025733615, -283.1203342715262465 ) ) ;
#85579 = CARTESIAN_POINT ( 'NONE',  ( -96.44809116857096853, -290.4111250448988244, -221.2429945923644539 ) ) ;
#85580 = CARTESIAN_POINT ( 'NONE',  ( -41.10012181139206433, -293.5000739352133223, -344.0780607851497734 ) ) ;
#85581 = CARTESIAN_POINT ( 'NONE',  ( -5.328647024294761891, -279.1673293274318439, -204.2066932574586531 ) ) ;
#85582 = CARTESIAN_POINT ( 'NONE',  ( -94.87606294870063550, -271.2884047939998595, -223.1065532404639100 ) ) ;
#85583 = CARTESIAN_POINT ( 'NONE',  ( -72.88000697145282913, -292.8864205847268636, -205.9745207508094325 ) ) ;
#85584 = CARTESIAN_POINT ( 'NONE',  ( -4.829096099716510437, -282.9805209788416391, -202.7746430608542312 ) ) ;
#85585 = CARTESIAN_POINT ( 'NONE',  ( -82.54414621805294416, -295.9274207310341467, -208.8182747641742196 ) ) ;
#85586 = CARTESIAN_POINT ( 'NONE',  ( 14.66139311657559574, -289.9049298967311756, -322.7263612970771760 ) ) ;
#85587 = CARTESIAN_POINT ( 'NONE',  ( -30.76236949919573505, -290.3739616631476679, -194.6077566276133837 ) ) ;
#85588 = CARTESIAN_POINT ( 'NONE',  ( -90.25248934431769499, -292.7105322276314610, -219.2159979661156228 ) ) ;
#85589 = DIRECTION ( 'NONE',  ( 0.000000000000000000, 0.000000000000000000, -1.000000000000000000 ) ) ;
#85590 = CARTESIAN_POINT ( 'NONE',  ( -110.5296002037081848, -291.3799112639683244, -268.4677586668598224 ) ) ;
#85591 = CARTESIAN_POINT ( 'NONE',  ( 165.7865175155837676, 3.000000000000000000, -9.000000000000001776 ) ) ;
#85592 = CARTESIAN_POINT ( 'NONE',  ( -88.39632076739410138, -292.5601965001120561, -213.2521482057046001 ) ) ;
#85594 = CARTESIAN_POINT ( 'NONE',  ( -2.439435508157327792, -292.5275188815695060, -206.2311530372823540 ) ) ;
#85593 = CARTESIAN_POINT ( 'NONE',  ( 27.87594980850826687, -279.0706561490188164, -232.6110856996642724 ) ) ;
#85595 = CARTESIAN_POINT ( 'NONE',  ( 37.98466697166355743, -281.3516765318192938, -254.3312487121299341 ) ) ;
#85596 = CARTESIAN_POINT ( 'NONE',  ( 38.23473724657374362, -281.0358927337142063, -255.7342110862453239 ) ) ;
#85597 = CARTESIAN_POINT ( 'NONE',  ( 36.48606533473977720, -285.7215866681849548, -283.5695129448341731 ) ) ;
#85598 = CARTESIAN_POINT ( 'NONE',  ( 34.31195114662135381, -279.4390737884366445, -250.9057321558088631 ) ) ;
#85599 = CARTESIAN_POINT ( 'NONE',  ( -108.0821718506374367, -282.8746962257821451, -245.4455343434404995 ) ) ;
#85600 = PLANE ( 'NONE',  #19999 ) ;
#85601 = CARTESIAN_POINT ( 'NONE',  ( -42.36490753274321719, -278.4697658415672663, -194.2199652434757411 ) ) ;
#85602 = CARTESIAN_POINT ( 'NONE',  ( -10.09088630242400164, -285.3199135600573300, -198.6185194870605812 ) ) ;
#85603 = CARTESIAN_POINT ( 'NONE',  ( 11.64707871944216144, -275.5554826588801234, -215.9541481952816184 ) ) ;
#85604 = CARTESIAN_POINT ( 'NONE',  ( 196.8803347170859865, 42.36571313990104670, 12.49999999999999112 ) ) ;
#85605 = CARTESIAN_POINT ( 'NONE',  ( 34.55941910400228778, -295.3699824761300761, -287.0502434905782252 ) ) ;
#85606 = CARTESIAN_POINT ( 'NONE',  ( 39.11797753642464670, -276.9873318526389312, -271.1473252018745370 ) ) ;
#85607 = CARTESIAN_POINT ( 'NONE',  ( -21.65261428490309115, -276.5122992219743878, -341.7289018854619371 ) ) ;
#85608 = CARTESIAN_POINT ( 'NONE',  ( -114.0070502354968625, -290.8154066162862250, -262.6390699424250101 ) ) ;
#85609 =( BOUNDED_SURFACE ( )  B_SPLINE_SURFACE ( 3, 2, ( 
 ( #33636, #27010, #18978 ),
 ( #83342, #47353, #55897 ),
 ( #26057, #54013, #4290 ),
 ( #47830, #11859, #84751 ),
 ( #11395, #19899, #40247 ),
 ( #62059, #77677, #40708 ) ),
 .UNSPECIFIED., .F., .F., .F. ) 
 B_SPLINE_SURFACE_WITH_KNOTS ( ( 4, 2, 4 ),
 ( 3, 3 ),
 ( 0.000000000000000000, 0.2633701841259441512, 0.5267403682518883024 ),
 ( 0.000000000000000000, 1.000000000000000000 ),
 .UNSPECIFIED. ) 
 GEOMETRIC_REPRESENTATION_ITEM ( )  RATIONAL_B_SPLINE_SURFACE ( (
 ( 1.000000000000000000, 0.9475641245298920268, 1.000000000000000000),
 ( 1.000000000000000000, 0.9475641245298920268, 1.000000000000000000),
 ( 1.000000000000000000, 0.9451322790880677394, 1.000000000000000000),
 ( 1.000000000000000000, 0.9354614375526321135, 1.000000000000000000),
 ( 1.000000000000000000, 0.9282241625909624094, 1.000000000000000000),
 ( 1.000000000000000000, 0.9186651033962678348, 1.000000000000000000) ) ) 
 REPRESENTATION_ITEM ( '' )  SURFACE ( )  );
#85610 = CARTESIAN_POINT ( 'NONE',  ( 38.08990486678211340, -279.6985883279926952, -275.5861483506444074 ) ) ;
#85611 = CARTESIAN_POINT ( 'NONE',  ( -64.38681532129820084, -291.5422200893734725, -198.2108282642895460 ) ) ;
#85612 = CARTESIAN_POINT ( 'NONE',  ( -14.76250794572301750, -291.4107899595201729, -200.6934172302254069 ) ) ;
#85613 = CARTESIAN_POINT ( 'NONE',  ( -36.32772128997841321, -293.0393184440316077, -345.3670314085981659 ) ) ;
#85614 = ORIENTED_EDGE ( 'NONE', *, *, #37532, .T. ) ;
#85615 = DIRECTION ( 'NONE',  ( 0.000000000000000000, 1.000000000000000000, 0.000000000000000000 ) ) ;
#85616 = CARTESIAN_POINT ( 'NONE',  ( -62.81631593080187770, -291.2190038226141837, -201.8846082046662218 ) ) ;
#85617 = CARTESIAN_POINT ( 'NONE',  ( 175.2296996224750103, 275.0000000000000568, 0.000000000000000000 ) ) ;
#85618 = CARTESIAN_POINT ( 'NONE',  ( -37.37352853689063181, -274.5523547857346784, -340.3611179825599606 ) ) ;
#85619 = CARTESIAN_POINT ( 'NONE',  ( -101.3468667017618543, -296.1703763394959878, -227.9560730383263092 ) ) ;
#85620 = CARTESIAN_POINT ( 'NONE',  ( -113.8477035252685425, -285.8718581595813930, -270.0009574507120078 ) ) ;
#85621 = CARTESIAN_POINT ( 'NONE',  ( 15.03097391921307668, -286.6502169098480977, -219.5073765505128733 ) ) ;
#85622 = CARTESIAN_POINT ( 'NONE',  ( -8.449172227651917666, -278.1870730336481188, -338.1680766581016542 ) ) ;
#85623 = CARTESIAN_POINT ( 'NONE',  ( -101.5948613704433257, -294.0605653771070251, -308.4547664474541762 ) ) ;
#85624 = CARTESIAN_POINT ( 'NONE',  ( -99.57335025802424866, -297.7642799903013042, -310.5198579874615916 ) ) ;
#85625 = CARTESIAN_POINT ( 'NONE',  ( -9.853820414761541358, -275.4799099457689522, -338.4302259340467458 ) ) ;
#85626 = ORIENTED_EDGE ( 'NONE', *, *, #66952, .F. ) ;
#85627 = CARTESIAN_POINT ( 'NONE',  ( 195.1989865542159066, 41.04625909772627779, 13.32094405520072122 ) ) ;
#85628 = CARTESIAN_POINT ( 'NONE',  ( -74.59984961037540074, -295.2002672339990568, -337.7823373737829229 ) ) ;
#85629 = CARTESIAN_POINT ( 'NONE',  ( 35.10623275568143242, -289.2503028145857229, -253.2002213704480766 ) ) ;
#85630 = CARTESIAN_POINT ( 'NONE',  ( -66.71072642002270925, -295.6672788974004789, -201.3367497637570125 ) ) ;
#85631 = CARTESIAN_POINT ( 'NONE',  ( -56.08373206472055017, -289.9512813307704278, -341.0722842075379617 ) ) ;
#85632 = ORIENTED_EDGE ( 'NONE', *, *, #9353, .F. ) ;
#85633 = CARTESIAN_POINT ( 'NONE',  ( -31.08095794509638310, -279.1880403954928056, -193.7996129039383391 ) ) ;
#85634 = CARTESIAN_POINT ( 'NONE',  ( -111.1152470976926736, -296.9305095436812962, -292.1049314110994146 ) ) ;
#85635 = CARTESIAN_POINT ( 'NONE',  ( -104.8919272473247730, -289.1420248176779637, -235.9341082319315603 ) ) ;
#85636 = CARTESIAN_POINT ( 'NONE',  ( -72.06069974033017900, -295.8319812882730844, -339.0658147474513839 ) ) ;
#85637 = CARTESIAN_POINT ( 'NONE',  ( -1.249916577458247025, -292.8783556283502776, -206.8685273923465218 ) ) ;
#85638 = DIRECTION ( 'NONE',  ( -0.6056179655966479336, 0.7957555401921982963, 0.000000000000000000 ) ) ;
#85639 = DIRECTION ( 'NONE',  ( 0.000000000000000000, 1.000000000000000000, 0.000000000000000000 ) ) ;
#85640 = CARTESIAN_POINT ( 'NONE',  ( -70.32172481685874743, -290.9989759546916730, -339.1869951918496895 ) ) ;
#85641 = CARTESIAN_POINT ( 'NONE',  ( -88.47809603358389552, -294.9094976428775681, -206.1857440867352693 ) ) ;
#85642 = VERTEX_POINT ( 'NONE', #47872 ) ;
#85643 = CARTESIAN_POINT ( 'NONE',  ( 29.20253095018268752, -280.3989211745574721, -231.8231095163028499 ) ) ;
#85644 = CARTESIAN_POINT ( 'NONE',  ( -68.52569315994661281, -285.4630320055049424, -338.3874879343434827 ) ) ;
#85645 = CARTESIAN_POINT ( 'NONE',  ( -18.31109446836311960, -284.8673060323918662, -196.3034452094861422 ) ) ;
#85646 = CARTESIAN_POINT ( 'NONE',  ( -74.28035954010299236, -287.6270583448797424, -335.0043673302799903 ) ) ;
#85647 = CARTESIAN_POINT ( 'NONE',  ( 14.06280831804406795, -278.2005351252448691, -326.0911639105086692 ) ) ;
#85648 = ORIENTED_EDGE ( 'NONE', *, *, #90537, .F. ) ;
#85650 = CARTESIAN_POINT ( 'NONE',  ( 31.16873647268653258, -280.5593790851364702, -244.7165791536186816 ) ) ;
#85649 = CARTESIAN_POINT ( 'NONE',  ( -96.88569645718911261, -277.9621966968304037, -312.6144804368162227 ) ) ;
#85651 = CARTESIAN_POINT ( 'NONE',  ( 19.79633913834168979, -275.9345203025673072, -219.1290420161784596 ) ) ;
#85652 = CARTESIAN_POINT ( 'NONE',  ( -38.15024140828950294, -278.8371609032972742, -193.7624562362642280 ) ) ;
#85653 = CARTESIAN_POINT ( 'NONE',  ( 195.2250370176061267, 284.1914500304793023, -110.9006798413472836 ) ) ;
#85654 = CARTESIAN_POINT ( 'NONE',  ( -58.06964132618014673, -274.7320905147675489, -196.3925819611789905 ) ) ;
#85655 = CARTESIAN_POINT ( 'NONE',  ( -36.21360370459082390, -299.4912800419726295, -193.9500752164755681 ) ) ;
#85656 = ADVANCED_FACE ( 'NONE', ( #76311 ), #11902, .F. ) ;
#85657 = CARTESIAN_POINT ( 'NONE',  ( -37.30987171927208124, -285.5519495502701943, -345.3611179825600175 ) ) ;
#85658 = EDGE_LOOP ( 'NONE', ( #62010, #19258, #10078, #28573 ) ) ;
#85659 = CARTESIAN_POINT ( 'NONE',  ( 82.62832869962693394, -301.1699953031597943, -193.4454218763038114 ) ) ;
#85660 = CARTESIAN_POINT ( 'NONE',  ( 16.24627932075137338, -289.3489404375036997, -320.4609492190604101 ) ) ;
#85661 = CARTESIAN_POINT ( 'NONE',  ( -33.79731722162228635, -287.8563145932638463, -194.4571565249364937 ) ) ;
#85662 = CARTESIAN_POINT ( 'NONE',  ( 31.07292536875174704, -286.5558212225456032, -244.4629539084911869 ) ) ;
#85663 = CARTESIAN_POINT ( 'NONE',  ( -95.76571894798283324, -284.7365381984394048, -220.2196471121708896 ) ) ;
#85664 = CARTESIAN_POINT ( 'NONE',  ( -22.00851402745521312, -278.6516009200969961, -198.1191210953321047 ) ) ;
#85665 = CARTESIAN_POINT ( 'NONE',  ( 19.59412720405913788, -288.7474324378407005, -222.7054423590212195 ) ) ;
#85666 = CARTESIAN_POINT ( 'NONE',  ( 34.31986644239420059, -280.2572973485837338, -287.5998452620785315 ) ) ;
#85667 = CARTESIAN_POINT ( 'NONE',  ( -9.788035268694443403, -277.9997528014484374, -338.5072876270148754 ) ) ;
#85668 = CARTESIAN_POINT ( 'NONE',  ( -5.286711455162205198, -274.9780947195160365, -204.6931425802561932 ) ) ;
#85669 = CARTESIAN_POINT ( 'NONE',  ( -34.69598244527006159, -287.8145275857817182, -346.9183442744681543 ) ) ;
#85670 = CARTESIAN_POINT ( 'NONE',  ( -38.71937977508299156, -283.8718481715195594, -347.1872907360625504 ) ) ;
#85671 = CARTESIAN_POINT ( 'NONE',  ( -105.3806057996520593, -285.5099239001870046, -234.3271974006147786 ) ) ;
#85672 = CARTESIAN_POINT ( 'NONE',  ( 34.70390239981624347, -281.8740417792929520, -282.1267952221280666 ) ) ;
#85673 = ORIENTED_EDGE ( 'NONE', *, *, #11195, .T. ) ;
#85674 = ORIENTED_EDGE ( 'NONE', *, *, #63406, .T. ) ;
#85675 = CARTESIAN_POINT ( 'NONE',  ( 209.3191041914274706, 28.92934851230250715, 12.09245862095555424 ) ) ;
#85676 = CARTESIAN_POINT ( 'NONE',  ( -77.46190241506330665, -291.4443009915162293, -334.6926333359923547 ) ) ;
#85677 = CARTESIAN_POINT ( 'NONE',  ( -90.43159448846546411, -290.0045755535269336, -215.1989393131665338 ) ) ;
#85678 = CARTESIAN_POINT ( 'NONE',  ( -56.91300004569694693, -272.8523595307430014, -199.7364786031569395 ) ) ;
#85679 = EDGE_CURVE ( 'NONE', #48629, #6151, #17263, .T. ) ;
#85680 = CARTESIAN_POINT ( 'NONE',  ( 25.62641189995187574, -293.4854557767727670, -314.5239824245462046 ) ) ;
#85681 = CARTESIAN_POINT ( 'NONE',  ( -97.13237767597787808, -288.4352696932550089, -313.4399136002857063 ) ) ;
#85682 = CARTESIAN_POINT ( 'NONE',  ( 36.65409205586339425, -291.8335557867605417, -273.5547447701430315 ) ) ;
#85683 = CARTESIAN_POINT ( 'NONE',  ( 30.32190048286579298, -288.3761207082243345, -241.7907236443691659 ) ) ;
#85684 = CARTESIAN_POINT ( 'NONE',  ( -4.771743288812468897, -291.1233781216987495, -337.9199732462171255 ) ) ;
#85685 = CARTESIAN_POINT ( 'NONE',  ( -94.84091013533529235, -291.8867198572891084, -318.5353800385944965 ) ) ;
#85686 = CARTESIAN_POINT ( 'NONE',  ( -63.72096588275577744, -289.7090353403534664, -199.9204772003336359 ) ) ;
#85687 = CARTESIAN_POINT ( 'NONE',  ( -89.77392117723161391, -293.3129983394313172, -216.6623688720681571 ) ) ;
#85688 = CARTESIAN_POINT ( 'NONE',  ( -74.85088203869791812, -286.4806232702046032, -207.4606432583150024 ) ) ;
#85689 = CARTESIAN_POINT ( 'NONE',  ( 14.16296423689625605, -294.7731795263302388, -215.5420907042164345 ) ) ;
#85690 = CARTESIAN_POINT ( 'NONE',  ( -114.2601182895341481, -273.1888302692865977, -270.3692244198358026 ) ) ;
#85691 = FACE_OUTER_BOUND ( 'NONE', #18104, .T. ) ;
#85692 = CARTESIAN_POINT ( 'NONE',  ( 73.72085311440586963, -301.3523753661854130, -194.7650907356766083 ) ) ;
#85693 = CARTESIAN_POINT ( 'NONE',  ( -12.90104227253787172, -280.7345018630948061, -341.3221420630307534 ) ) ;
#85694 = CARTESIAN_POINT ( 'NONE',  ( -104.4668316174843454, -295.2622832809120723, -307.8647735153213034 ) ) ;
#85695 = CARTESIAN_POINT ( 'NONE',  ( -51.73690304907813697, -272.1054623281968929, -197.7086668234656770 ) ) ;
#85696 = CARTESIAN_POINT ( 'NONE',  ( -64.88832187261836282, -275.4944709412690145, -339.5714740457713674 ) ) ;
#85697 = CARTESIAN_POINT ( 'NONE',  ( -41.91565298661817707, -299.3084846687801246, -197.0104367736587108 ) ) ;
#85698 = CARTESIAN_POINT ( 'NONE',  ( 37.06532759786092868, -273.9071475562366800, -252.9202260240812166 ) ) ;
#85699 = ADVANCED_FACE ( 'NONE', ( #63065 ), #89829, .T. ) ;
#85700 = CARTESIAN_POINT ( 'NONE',  ( -93.52055971136928747, -297.3070798532343701, -317.9128395397153213 ) ) ;
#85701 = FACE_OUTER_BOUND ( 'NONE', #73212, .T. ) ;
#85702 = CARTESIAN_POINT ( 'NONE',  ( -108.1232084552512447, -297.1105650562094525, -288.9195344937976415 ) ) ;
#85703 = CARTESIAN_POINT ( 'NONE',  ( 151.9245405993102338, 130.8357700577111018, 11.49999999999999645 ) ) ;
#85705 = CARTESIAN_POINT ( 'NONE',  ( -35.14775944149625531, -298.0803702048956438, -197.3611180162293408 ) ) ;
#85704 = CARTESIAN_POINT ( 'NONE',  ( 8.823414105639065141, -284.7018156203092190, -210.8028353717432140 ) ) ;
#85706 = CARTESIAN_POINT ( 'NONE',  ( -67.18905943793892277, -285.6714749786099219, -199.3812959045337720 ) ) ;
#85707 = CARTESIAN_POINT ( 'NONE',  ( 16.66809589160853022, -287.9761739317270894, -325.2867296352273456 ) ) ;
#85708 = CARTESIAN_POINT ( 'NONE',  ( -110.6795407128679329, -298.7533848727259169, -253.0415352593796001 ) ) ;
#85709 = CARTESIAN_POINT ( 'NONE',  ( -12.42113940956891582, -292.7272644515553566, -340.9776930315268260 ) ) ;
#85710 = CARTESIAN_POINT ( 'NONE',  ( -86.69316799550755093, -278.5836415284378518, -211.3970264562993293 ) ) ;
#85711 = CARTESIAN_POINT ( 'NONE',  ( -85.33152481854862970, -293.1952119285919593, -330.4860931364851808 ) ) ;
#85712 = FACE_OUTER_BOUND ( 'NONE', #93247, .T. ) ;
#85713 = CARTESIAN_POINT ( 'NONE',  ( 23.06803662453980763, -286.9247910738117184, -312.0701241328527544 ) ) ;
#85714 = DIRECTION ( 'NONE',  ( -0.000000000000000000, -1.000000000000000000, -0.000000000000000000 ) ) ;
#85715 = CARTESIAN_POINT ( 'NONE',  ( -53.87350090601299968, -287.2642022878402486, -343.5164336381164389 ) ) ;
#85716 = CARTESIAN_POINT ( 'NONE',  ( -110.2717623132042490, -274.2150852030433725, -259.4328274767220819 ) ) ;
#85717 = CARTESIAN_POINT ( 'NONE',  ( 5.836234480685224213, -282.0503584991929529, -207.3192885790292053 ) ) ;
#85719 = CARTESIAN_POINT ( 'NONE',  ( 34.48544930250888285, -281.7250038463617443, -283.4642198079997684 ) ) ;
#85718 = CARTESIAN_POINT ( 'NONE',  ( -96.98833363688429188, -293.9441976605648961, -316.4120237049493198 ) ) ;
#85720 = CARTESIAN_POINT ( 'NONE',  ( -113.6523343058869671, -296.5853779519620730, -281.0319655623688959 ) ) ;
#85721 = CARTESIAN_POINT ( 'NONE',  ( -88.62198031439875479, -298.8372975569203049, -217.3649965788345071 ) ) ;
#85722 = CARTESIAN_POINT ( 'NONE',  ( 18.61897101117994069, -282.8570347894951738, -220.4078193683573090 ) ) ;
#85723 = CARTESIAN_POINT ( 'NONE',  ( -110.4464514635021999, -295.6683673989566614, -265.9903309002061178 ) ) ;
#85724 = VERTEX_POINT ( 'NONE', #68745 ) ;
#85725 = LINE ( 'NONE', #79575, #25657 ) ;
#85726 = CARTESIAN_POINT ( 'NONE',  ( -93.78673188038794706, -285.8511835702556709, -319.2252658153869334 ) ) ;
#85727 = LINE ( 'NONE', #71549, #3535 ) ;
#85728 = CARTESIAN_POINT ( 'NONE',  ( 31.98288692825983404, -290.6237833571634042, -237.0123917617631264 ) ) ;
#85729 = CARTESIAN_POINT ( 'NONE',  ( 32.86807142883216670, -275.1486438893880404, -301.5820532334019504 ) ) ;
#85730 = CARTESIAN_POINT ( 'NONE',  ( -12.25821258863840590, -292.2209570461576504, -201.7520162747607912 ) ) ;
#85731 = CARTESIAN_POINT ( 'NONE',  ( 18.47714651961067744, -282.3932482922413669, -222.2276796297211376 ) ) ;
#85732 = CARTESIAN_POINT ( 'NONE',  ( -8.406438897629112006, -278.2670665265890193, -338.2658343669842793 ) ) ;
#85733 = CARTESIAN_POINT ( 'NONE',  ( -111.3000326655414938, -285.7346250109096673, -289.6163627032206023 ) ) ;
#85734 = CARTESIAN_POINT ( 'NONE',  ( 33.50084658414023409, -280.0943080848075510, -251.1175769027694287 ) ) ;
#85735 = CARTESIAN_POINT ( 'NONE',  ( -96.00179778450207380, -279.9096711107787883, -317.1148411863597971 ) ) ;
#85736 = CARTESIAN_POINT ( 'NONE',  ( -85.80987657102753019, -273.5686025485974824, -210.5293883002286748 ) ) ;
#85737 = CARTESIAN_POINT ( 'NONE',  ( 38.49247849006026456, -275.2175914622532105, -256.9374563610105042 ) ) ;
#85738 = CARTESIAN_POINT ( 'NONE',  ( 36.64088209824904396, -295.5847777890091379, -279.0549050300811018 ) ) ;
#85739 = CARTESIAN_POINT ( 'NONE',  ( 236.4625231464875128, -138.0407542764614846, 22.50000000000000000 ) ) ;
#85740 = EDGE_CURVE ( 'NONE', #6120, #26691, #34626, .T. ) ;
#85741 = CARTESIAN_POINT ( 'NONE',  ( 170.4537599243631405, 275.0000000000000568, -23.51999999999999602 ) ) ;
#85742 = CARTESIAN_POINT ( 'NONE',  ( -111.4028354867733981, -294.4886743293645281, -286.3377795149082772 ) ) ;
#85743 = CARTESIAN_POINT ( 'NONE',  ( 15.63819010738987458, -275.7844356949537996, -320.6713522526613360 ) ) ;
#85744 = CARTESIAN_POINT ( 'NONE',  ( 10.77624762452223095, -295.9211792751279972, -329.6522842735044492 ) ) ;
#85745 = CARTESIAN_POINT ( 'NONE',  ( 22.86914366386307051, -295.3939904286159503, -317.7389313950892529 ) ) ;
#85746 = CARTESIAN_POINT ( 'NONE',  ( 34.85732033990312573, -289.8081786543672820, -290.2343563553295098 ) ) ;
#85747 = CARTESIAN_POINT ( 'NONE',  ( -67.56590383719320414, -275.4494358112877990, -338.8193237687033275 ) ) ;
#85748 = CARTESIAN_POINT ( 'NONE',  ( -5.641628879685472775, -278.5521394614029873, -337.7281092861886123 ) ) ;
#85749 = CARTESIAN_POINT ( 'NONE',  ( -110.1832310492710860, -294.8312661254718137, -254.9563429599116660 ) ) ;
#85750 = CARTESIAN_POINT ( 'NONE',  ( 21.57789524123696978, -284.0618348067586112, -318.0133791635034868 ) ) ;
#85751 = CARTESIAN_POINT ( 'NONE',  ( -87.89777669145703953, -284.2451970324794956, -217.2733680245724486 ) ) ;
#85752 = CARTESIAN_POINT ( 'NONE',  ( 104.9453854588719111, 114.9807708061526768, -282.1350155447395309 ) ) ;
#85753 = ORIENTED_EDGE ( 'NONE', *, *, #42570, .T. ) ;
#85754 = CARTESIAN_POINT ( 'NONE',  ( -103.0335413260907558, -283.7859501076784454, -302.3625121701737157 ) ) ;
#85755 = CARTESIAN_POINT ( 'NONE',  ( 33.28664616673696486, -283.0152322226035153, -300.3820624017549790 ) ) ;
#85756 = CARTESIAN_POINT ( 'NONE',  ( -113.7545427575485348, -283.4237204857101347, -264.2644808022508300 ) ) ;
#85757 = CARTESIAN_POINT ( 'NONE',  ( -101.7005176884557756, -280.0456748938203759, -228.4227924386562449 ) ) ;
#85758 = CARTESIAN_POINT ( 'NONE',  ( -99.07732452895298536, -279.4715437568043512, -315.2321911048433662 ) ) ;
#85759 = CARTESIAN_POINT ( 'NONE',  ( -102.0172624299487154, -270.4809262143062369, -239.1787733560258289 ) ) ;
#85760 = CARTESIAN_POINT ( 'NONE',  ( -94.53301180112747204, -240.7393305608231913, -341.8848713043685166 ) ) ;
#85761 = VERTEX_POINT ( 'NONE', #72942 ) ;
#85762 = CARTESIAN_POINT ( 'NONE',  ( -107.1351055028651444, -274.9058821298693260, -243.2197343025253815 ) ) ;
#85763 = CARTESIAN_POINT ( 'NONE',  ( -67.95838257802341786, -277.6683635073297864, -202.2702986123385642 ) ) ;
#85764 = CARTESIAN_POINT ( 'NONE',  ( -111.0176479060446866, -292.5486748608047947, -251.7121738408289389 ) ) ;
#85765 = CARTESIAN_POINT ( 'NONE',  ( 21.89216935441539036, -292.3020215004322040, -227.5001114091085697 ) ) ;
#85766 = CARTESIAN_POINT ( 'NONE',  ( -112.8088645201898288, -289.8715453812329201, -285.4023685039321663 ) ) ;
#85767 = FACE_OUTER_BOUND ( 'NONE', #5646, .T. ) ;
#85769 = CARTESIAN_POINT ( 'NONE',  ( -67.86012005591703655, -284.0446007464481681, -203.1668737180935409 ) ) ;
#85768 = CARTESIAN_POINT ( 'NONE',  ( 21.81881515393812521, -292.7812609300220856, -318.7411363038077070 ) ) ;
#85770 = CARTESIAN_POINT ( 'NONE',  ( -55.33428400204005726, -293.6786350541656816, -198.3393684687820553 ) ) ;
#85771 = CARTESIAN_POINT ( 'NONE',  ( -8.283950716791443014, -283.9786676134251593, -337.8658635795046621 ) ) ;
#85772 = ORIENTED_EDGE ( 'NONE', *, *, #17827, .F. ) ;
#85773 = CARTESIAN_POINT ( 'NONE',  ( -112.6962975145030725, -291.6779892833129679, -255.6466024279604881 ) ) ;
#85774 = CARTESIAN_POINT ( 'NONE',  ( -6.749370263548423843, -280.9572518169413797, -203.9991546187190750 ) ) ;
#85775 = CARTESIAN_POINT ( 'NONE',  ( 37.07060684332193290, -292.5764034922810310, -288.6043414482115850 ) ) ;
#85776 = CARTESIAN_POINT ( 'NONE',  ( 37.66954564181710197, -288.5644961872640692, -287.0787069798631705 ) ) ;
#85777 = CARTESIAN_POINT ( 'NONE',  ( -113.9461947854349262, -291.1410213015502677, -262.6493668697426074 ) ) ;
#85778 = CARTESIAN_POINT ( 'NONE',  ( 35.65519841913559418, -287.7277101066745217, -271.0340273153930752 ) ) ;
#85779 = ORIENTED_EDGE ( 'NONE', *, *, #43643, .F. ) ;
#85780 = DIRECTION ( 'NONE',  ( 0.000000000000000000, 1.000000000000000000, 0.000000000000000000 ) ) ;
#85781 = CARTESIAN_POINT ( 'NONE',  ( -33.47381399219635512, -296.8643924128447225, -346.0400358634137774 ) ) ;
#85782 = CARTESIAN_POINT ( 'NONE',  ( -65.34579475146988159, -296.3786194635000015, -199.1071049529226400 ) ) ;
#85783 = CARTESIAN_POINT ( 'NONE',  ( -85.26824692627361912, -276.7919171746917755, -325.8038811662642047 ) ) ;
#85784 = CARTESIAN_POINT ( 'NONE',  ( -26.99857988267562448, -273.6878153121984951, -194.0676702579505104 ) ) ;
#85785 = CARTESIAN_POINT ( 'NONE',  ( -100.7730316895313791, -294.5202615458483137, -307.9739570292107373 ) ) ;
#85786 = CARTESIAN_POINT ( 'NONE',  ( 35.62087088786995537, -277.1496272757230486, -257.8586944271748962 ) ) ;
#85787 = CARTESIAN_POINT ( 'NONE',  ( -52.82550546027108851, -296.0910042078525635, -197.9329270260638509 ) ) ;
#85788 = CARTESIAN_POINT ( 'NONE',  ( 12.63642499629979099, -295.5419929105079859, -324.1831632783031978 ) ) ;
#85789 = CARTESIAN_POINT ( 'NONE',  ( -80.32495229518906399, -296.7297519182717451, -329.7468579030024785 ) ) ;
#85790 = DIRECTION ( 'NONE',  ( 0.000000000000000000, 0.000000000000000000, 1.000000000000000000 ) ) ;
#85791 = CARTESIAN_POINT ( 'NONE',  ( -106.6936256947451938, -294.1727584114302658, -299.4845382643239873 ) ) ;
#85792 = CARTESIAN_POINT ( 'NONE',  ( -112.9113753381214735, -273.5328259274955371, -256.1706220193983086 ) ) ;
#85793 = CARTESIAN_POINT ( 'NONE',  ( -50.87751384109608921, -287.8030658880169881, -342.7468645324327667 ) ) ;
#85794 = CARTESIAN_POINT ( 'NONE',  ( -111.5657523610991149, -274.6950462632147492, -259.2447671250016015 ) ) ;
#85795 = CARTESIAN_POINT ( 'NONE',  ( -36.94634933104565988, -274.5493541400449544, -193.4106304115468902 ) ) ;
#85796 = CARTESIAN_POINT ( 'NONE',  ( -98.46759592877810974, -297.4399682125919639, -230.3232402885087708 ) ) ;
#85797 = CARTESIAN_POINT ( 'NONE',  ( -31.23279406911437306, -282.1087133302665961, -195.2023754378563183 ) ) ;
#85798 = CARTESIAN_POINT ( 'NONE',  ( 39.03569538216176937, -280.3034709773987743, -275.6436429937372168 ) ) ;
#85799 = EDGE_CURVE ( 'NONE', #55239, #54554, #70204, .T. ) ;
#85800 = CARTESIAN_POINT ( 'NONE',  ( -8.085360970329940500, -282.0275942556496602, -341.5328336744230455 ) ) ;
#85801 = CARTESIAN_POINT ( 'NONE',  ( 29.86249072600618248, -274.4143903612652480, -232.8763482313367490 ) ) ;
#85802 = CARTESIAN_POINT ( 'NONE',  ( 37.47315155673641840, -279.7692503375686215, -255.8981174442102144 ) ) ;
#85803 = CARTESIAN_POINT ( 'NONE',  ( -12.10041799479818181, -278.3795462083166399, -199.5045815458435072 ) ) ;
#85804 = EDGE_CURVE ( 'NONE', #85293, #19459, #87587, .T. ) ;
#85805 = CARTESIAN_POINT ( 'NONE',  ( -43.51359144666648149, -272.5475277165089665, -196.9800407331447332 ) ) ;
#85806 = CARTESIAN_POINT ( 'NONE',  ( -19.85633632169537321, -276.2769523627447938, -197.3750361555509585 ) ) ;
#85807 = DIRECTION ( 'NONE',  ( 0.000000000000000000, -0.8660254037844385966, 0.5000000000000000000 ) ) ;
#85808 = CARTESIAN_POINT ( 'NONE',  ( 200.7568414405312467, 39.78480925505071752, 10.50000000000000000 ) ) ;
#85809 = CARTESIAN_POINT ( 'NONE',  ( 19.16243952856850186, -290.8822657840449892, -220.4849307037962944 ) ) ;
#85810 = CARTESIAN_POINT ( 'NONE',  ( -47.74339216224365146, -291.9235117316364381, -194.0131243149929503 ) ) ;
#85811 = CARTESIAN_POINT ( 'NONE',  ( -12.44871337131436206, -278.7294596728138458, -341.3408056513137012 ) ) ;
#85812 = CARTESIAN_POINT ( 'NONE',  ( 22.28671310206897616, -272.9291108996798130, -224.8487290386991333 ) ) ;
#85813 = CARTESIAN_POINT ( 'NONE',  ( 60.30156426812553860, -249.1647034777049612, -22.50000000000000000 ) ) ;
#85814 = CARTESIAN_POINT ( 'NONE',  ( 208.6208076322478746, 32.98517505407394168, 14.69807322781335657 ) ) ;
#85815 = CARTESIAN_POINT ( 'NONE',  ( -102.4604238925557951, -283.0494305424492154, -233.0481712420753695 ) ) ;
#85816 = DIRECTION ( 'NONE',  ( -1.000000000000000000, 0.000000000000000000, 0.000000000000000000 ) ) ;
#85817 = CARTESIAN_POINT ( 'NONE',  ( 30.94940323027170592, -292.7064750406875078, -297.3972325438379585 ) ) ;
#85818 = CARTESIAN_POINT ( 'NONE',  ( 17.82413611787097452, -284.9921599658878222, -220.6672302870377109 ) ) ;
#85819 = CARTESIAN_POINT ( 'NONE',  ( 156.4851178187871312, 1.000000000000000000, 7.000000000000000000 ) ) ;
#85820 = DIRECTION ( 'NONE',  ( 0.000000000000000000, 1.000000000000000000, 0.000000000000000000 ) ) ;
#85821 = CARTESIAN_POINT ( 'NONE',  ( 2.614354125536130002, -292.5166364664996763, -333.8931922374497390 ) ) ;
#85822 = CARTESIAN_POINT ( 'NONE',  ( -44.37476865659339609, -281.6193288297670279, -346.3958598503389226 ) ) ;
#85823 = CARTESIAN_POINT ( 'NONE',  ( -105.1854217436183063, -280.5382327403985983, -241.3151225513428813 ) ) ;
#85824 = CARTESIAN_POINT ( 'NONE',  ( -103.7041802232159426, -286.2583951535875713, -231.9929530054473048 ) ) ;
#85825 = CARTESIAN_POINT ( 'NONE',  ( 24.27231187649644184, -280.3898207318718505, -314.8543957327372596 ) ) ;
#85826 = CARTESIAN_POINT ( 'NONE',  ( 2.447014477759043238, -286.6019865148135182, -209.1577014928330414 ) ) ;
#85827 = CARTESIAN_POINT ( 'NONE',  ( -40.51313852930374537, -278.5180517248779779, -343.8945433916259162 ) ) ;
#85828 = CARTESIAN_POINT ( 'NONE',  ( -80.90735955920331435, -278.4638174307096392, -329.1372614830498264 ) ) ;
#85829 = CARTESIAN_POINT ( 'NONE',  ( -82.31488457452613261, -287.4221278830089545, -209.8326594777478533 ) ) ;
#85830 = ORIENTED_EDGE ( 'NONE', *, *, #58734, .F. ) ;
#85831 = CARTESIAN_POINT ( 'NONE',  ( 30.79044743357041725, -298.7164300005194377, -193.3629520540350768 ) ) ;
#85832 = CARTESIAN_POINT ( 'NONE',  ( 13.28957391886754635, -290.3202489952476526, -325.2795396473097185 ) ) ;
#85833 = CARTESIAN_POINT ( 'NONE',  ( -57.23711263161519724, -282.8906705383787994, 57.50000000000000711 ) ) ;
#85834 = CARTESIAN_POINT ( 'NONE',  ( -88.52914483777347243, -275.9090924074130271, -206.2264541496106460 ) ) ;
#85835 = VERTEX_POINT ( 'NONE', #72484 ) ;
#85836 = CARTESIAN_POINT ( 'NONE',  ( 23.84961573162311055, -272.9594273835972444, -226.6853232383336945 ) ) ;
#85837 = CARTESIAN_POINT ( 'NONE',  ( 37.28265016409321930, -291.7564006316505925, -254.8812888575445754 ) ) ;
#85838 = CARTESIAN_POINT ( 'NONE',  ( -93.99423961548697548, -295.4071145937429037, -316.5162158226945053 ) ) ;
#85839 = CARTESIAN_POINT ( 'NONE',  ( 28.26667228697986900, -288.6192598304143075, -236.6890277552311659 ) ) ;
#85840 = CARTESIAN_POINT ( 'NONE',  ( -1.494647797404490053, -282.2945127053787928, -205.6080265215061331 ) ) ;
#85841 = CARTESIAN_POINT ( 'NONE',  ( -12.39878815453698024, -290.1593695883699411, -342.6416145997918079 ) ) ;
#85842 = CARTESIAN_POINT ( 'NONE',  ( -54.37541671862952342, -290.5815790275290169, -345.0020090174414804 ) ) ;
#85843 = CARTESIAN_POINT ( 'NONE',  ( -88.26870779457259175, -285.7650690485356790, -325.4906657391997555 ) ) ;
#85844 = CARTESIAN_POINT ( 'NONE',  ( -114.0789197055876656, -278.6316363909194820, -277.3331901124690262 ) ) ;
#85845 = CARTESIAN_POINT ( 'NONE',  ( 20.25385196770011476, -292.3038888789243970, -319.2698756806485676 ) ) ;
#85846 = CARTESIAN_POINT ( 'NONE',  ( 35.32839188608864589, -281.0625917986267837, -244.7448771800976886 ) ) ;
#85847 = CARTESIAN_POINT ( 'NONE',  ( -74.91874138816510253, -275.4069004883340313, -206.2794439007923017 ) ) ;
#85848 = CARTESIAN_POINT ( 'NONE',  ( -4.771743288812468897, -291.1233781216987495, -337.9199732462171255 ) ) ;
#85849 = CARTESIAN_POINT ( 'NONE',  ( 32.78710686273940667, -273.4134517781415070, -240.9689351963718025 ) ) ;
#85850 = CARTESIAN_POINT ( 'NONE',  ( -113.5000000000000568, -298.0521521680024080, -540.3336712212508246 ) ) ;
#85851 = CARTESIAN_POINT ( 'NONE',  ( 26.51566355916656192, -280.5748518290793072, -234.8614624291071493 ) ) ;
#85852 = CARTESIAN_POINT ( 'NONE',  ( -48.42130949917548577, -278.3951211357284592, -346.2121669165729259 ) ) ;
#85853 = CARTESIAN_POINT ( 'NONE',  ( -34.46908655563495927, -299.5140766823485023, -196.7711715412838203 ) ) ;
#85854 = CARTESIAN_POINT ( 'NONE',  ( -69.68275518038723249, -284.6954935745990269, -200.7272858806688021 ) ) ;
#85855 = CARTESIAN_POINT ( 'NONE',  ( -108.7351969225418884, -292.5666290335522604, -250.8433663041809609 ) ) ;
#85856 = CARTESIAN_POINT ( 'NONE',  ( -83.11596427144279176, -275.0376802593943921, -209.3757974498577141 ) ) ;
#85857 = ADVANCED_FACE ( 'NONE', ( #6698, #44040 ), #28464, .F. ) ;
#85858 = CARTESIAN_POINT ( 'NONE',  ( -49.65647411403506339, -275.2135604399873614, -194.7984205639671700 ) ) ;
#85859 = FACE_OUTER_BOUND ( 'NONE', #42579, .T. ) ;
#85860 = ADVANCED_FACE ( 'NONE', ( #78654 ), #28926, .T. ) ;
#85861 = CARTESIAN_POINT ( 'NONE',  ( -28.65858273116080568, -296.9420813793094567, -344.7412818163851398 ) ) ;
#85862 = CARTESIAN_POINT ( 'NONE',  ( -36.19024188133170838, -281.0375223410755439, -345.1855964259405027 ) ) ;
#85863 = CARTESIAN_POINT ( 'NONE',  ( -98.32890813025441901, -290.8460570862450254, -223.3684722317218814 ) ) ;
#85864 = CARTESIAN_POINT ( 'NONE',  ( 37.24410522536589241, -273.6247056781155038, -274.4268006788329330 ) ) ;
#85865 = CARTESIAN_POINT ( 'NONE',  ( -43.62087830060645643, -287.5743322721689310, -194.3675640441131520 ) ) ;
#85866 = CARTESIAN_POINT ( 'NONE',  ( -62.89565014937137732, -290.6317743444828920, -201.6499710564887096 ) ) ;
#85867 = ORIENTED_EDGE ( 'NONE', *, *, #43526, .T. ) ;
#85868 = CARTESIAN_POINT ( 'NONE',  ( -112.3430818000429099, -289.3118475998882104, -255.6848548715323659 ) ) ;
#85869 = CARTESIAN_POINT ( 'NONE',  ( -83.83923711355822661, -291.0595442950219649, -214.0577740235804072 ) ) ;
#85870 = ORIENTED_EDGE ( 'NONE', *, *, #74086, .T. ) ;
#85871 = CARTESIAN_POINT ( 'NONE',  ( 20.34948352732071797, -289.3183420156282750, -320.9103019499520428 ) ) ;
#85872 = CARTESIAN_POINT ( 'NONE',  ( 15.61613512433503459, -276.6099308755381116, -320.6359145724442783 ) ) ;
#85873 = CARTESIAN_POINT ( 'NONE',  ( -5.936905153447610495, -293.5692387928554581, -340.3270480010504002 ) ) ;
#85874 = CARTESIAN_POINT ( 'NONE',  ( -113.8016262650160115, -285.1009116203874214, -278.5582200044751744 ) ) ;
#85875 = CARTESIAN_POINT ( 'NONE',  ( -89.87491651513268209, -285.6682064388401727, -214.0213469282071230 ) ) ;
#85876 = CARTESIAN_POINT ( 'NONE',  ( 33.96197988333747020, -282.0930632603577806, -286.1050915504005729 ) ) ;
#85877 = CARTESIAN_POINT ( 'NONE',  ( -39.76822214190186600, -139.5689616928363250, -364.7666786286931710 ) ) ;
#85878 = CARTESIAN_POINT ( 'NONE',  ( 192.6862340675979794, 279.0923067692335167, -125.4747399153907423 ) ) ;
#85879 = CARTESIAN_POINT ( 'NONE',  ( -110.9460938673244925, -268.0485775136007760, -295.3054752808368448 ) ) ;
#85880 = CARTESIAN_POINT ( 'NONE',  ( -56.89495719884656211, -272.9907566640177379, -199.8081319336176023 ) ) ;
#85881 = CARTESIAN_POINT ( 'NONE',  ( 32.35998771573641619, -274.1704188865296032, -247.4842727566924623 ) ) ;
#85882 = CARTESIAN_POINT ( 'NONE',  ( -50.46320073889224034, -294.7229112231660224, -346.2263198580622543 ) ) ;
#85883 = CARTESIAN_POINT ( 'NONE',  ( -110.4703031237083479, -271.8150658180700816, -270.3517331077227368 ) ) ;
#85884 = CARTESIAN_POINT ( 'NONE',  ( -63.37345732133692167, -272.4047490413110495, -198.4191560288155642 ) ) ;
#85885 = CARTESIAN_POINT ( 'NONE',  ( -86.94290714680967369, -299.2133778354631772, -215.1290101081950183 ) ) ;
#85886 = CARTESIAN_POINT ( 'NONE',  ( -50.82562026649912212, -290.5430711862491648, -342.6587482699363250 ) ) ;
#85887 = CARTESIAN_POINT ( 'NONE',  ( -67.94270306975059270, -292.7204072126145888, -203.7304741619769572 ) ) ;
#85888 = VERTEX_POINT ( 'NONE', #43586 ) ;
#85889 = CARTESIAN_POINT ( 'NONE',  ( -101.3601039914526183, -298.0525766679422190, -227.9760602943774188 ) ) ;
#85890 = CARTESIAN_POINT ( 'NONE',  ( 19.56536138227702182, -288.6917730722765896, -316.1822352991061393 ) ) ;
#85891 = CARTESIAN_POINT ( 'NONE',  ( 15.37534463307258292, -295.1324017058364007, -326.2634615092802619 ) ) ;
#85892 = CARTESIAN_POINT ( 'NONE',  ( -70.77545756792481768, -295.9736512146345717, -339.6699936239069757 ) ) ;
#85893 = CARTESIAN_POINT ( 'NONE',  ( 23.34006628128329197, -293.1552800687647959, -229.7812802556142344 ) ) ;
#85894 = ORIENTED_EDGE ( 'NONE', *, *, #33593, .F. ) ;
#85895 = CARTESIAN_POINT ( 'NONE',  ( 33.36547123559886074, -277.1288044683890348, -243.7188561796357646 ) ) ;
#85896 = ORIENTED_EDGE ( 'NONE', *, *, #51587, .T. ) ;
#85897 = CARTESIAN_POINT ( 'NONE',  ( -88.88556909322818456, -278.8583153894616657, -213.2405746099364876 ) ) ;
#85898 = AXIS2_PLACEMENT_3D ( 'NONE', #19942, #49298, #48814 ) ;
#85899 = CARTESIAN_POINT ( 'NONE',  ( 36.38736679794425299, -273.8965842165549134, -266.1130124511934127 ) ) ;
#85900 = CARTESIAN_POINT ( 'NONE',  ( 21.66366780981341833, -275.8875566233835457, -226.9816873368371546 ) ) ;
#85901 = CARTESIAN_POINT ( 'NONE',  ( -13.40324992060266496, -276.1189731458235883, -198.2436817139098082 ) ) ;
#85902 = CARTESIAN_POINT ( 'NONE',  ( 37.73949906315206704, -273.6543057514366524, -276.7814239591461387 ) ) ;
#85903 = CARTESIAN_POINT ( 'NONE',  ( -39.17919470572959995, -298.6799372295545822, -197.2698558067367003 ) ) ;
#85904 = CARTESIAN_POINT ( 'NONE',  ( -110.9633506204263540, -295.1485881538445710, -268.7016428887591246 ) ) ;
#85905 = CARTESIAN_POINT ( 'NONE',  ( 175.2296996224750103, 21.00000000000000000, 0.000000000000000000 ) ) ;
#85906 = CARTESIAN_POINT ( 'NONE',  ( -79.88198220455588228, -279.9861425904303474, -206.1890838177548915 ) ) ;
#85907 = CARTESIAN_POINT ( 'NONE',  ( 16.53258862093414905, -276.4256463369239896, -319.6398988981445655 ) ) ;
#85908 = CARTESIAN_POINT ( 'NONE',  ( 0.05744414204401958324, -285.2239752474326906, -203.6033582223108169 ) ) ;
#85909 = CARTESIAN_POINT ( 'NONE',  ( -102.5048116201718926, -275.0486224183449622, -233.1250473379532480 ) ) ;
#85910 = CARTESIAN_POINT ( 'NONE',  ( 82.65035235331711760, -299.4402615872036790, -197.8644493715226531 ) ) ;
#85911 = CARTESIAN_POINT ( 'NONE',  ( 22.87701180632885922, -287.3269692967478477, -311.9320644950454380 ) ) ;
#85912 = CARTESIAN_POINT ( 'NONE',  ( -66.44783850786315327, -277.9055762000330105, -202.2972607502154858 ) ) ;
#85914 = EDGE_CURVE ( 'NONE', #15111, #90289, #91381, .T. ) ;
#85913 = CARTESIAN_POINT ( 'NONE',  ( -35.63105069429413874, -278.6487229050646306, -196.7792698591719613 ) ) ;
#85915 = CARTESIAN_POINT ( 'NONE',  ( -35.15257581845639834, -285.0248523139926533, -345.3418173332767651 ) ) ;
#85916 = CARTESIAN_POINT ( 'NONE',  ( -6.093714602630924126, -277.8371768665330706, -336.7880182516466334 ) ) ;
#85917 = DIRECTION ( 'NONE',  ( 0.000000000000000000, 0.000000000000000000, -1.000000000000000000 ) ) ;
#85918 = CARTESIAN_POINT ( 'NONE',  ( -17.64248802589491660, -275.0412929209162485, -343.7499117727878684 ) ) ;
#85919 = CARTESIAN_POINT ( 'NONE',  ( 31.21103360533861348, -275.8655311557355958, -244.9757803702410115 ) ) ;
#85920 = CARTESIAN_POINT ( 'NONE',  ( 37.58221360234861663, -283.4749831303787460, -264.3249291374853556 ) ) ;
#85921 = DIRECTION ( 'NONE',  ( 1.000000000000000000, 0.000000000000000000, -0.000000000000000000 ) ) ;
#85922 = CARTESIAN_POINT ( 'NONE',  ( 32.71655054365363924, -289.8400890457534729, -298.8052886702989213 ) ) ;
#85923 = CARTESIAN_POINT ( 'NONE',  ( 22.69887783722546004, -292.1662705975508061, -315.3280756122244384 ) ) ;
#85924 = EDGE_CURVE ( 'NONE', #10184, #20922, #86665, .T. ) ;
#85925 = FACE_OUTER_BOUND ( 'NONE', #53620, .T. ) ;
#85926 = CARTESIAN_POINT ( 'NONE',  ( -54.30924655656728817, -272.5144278092167838, -198.8534551430940382 ) ) ;
#85927 = CARTESIAN_POINT ( 'NONE',  ( -9.238263802550241266, -290.5629460370223569, -201.5964267825922036 ) ) ;
#85928 = CARTESIAN_POINT ( 'NONE',  ( 173.4479467868932829, 229.7134184023448142, -192.0138545908111496 ) ) ;
#85929 = DIRECTION ( 'NONE',  ( -0.000000000000000000, -0.000000000000000000, 1.000000000000000000 ) ) ;
#85930 = CARTESIAN_POINT ( 'NONE',  ( -94.94772175729167429, -288.3495179891542080, -320.4036401610202347 ) ) ;
#85931 = CARTESIAN_POINT ( 'NONE',  ( -66.86105440172073600, -285.0456632616154593, -338.0139378429362864 ) ) ;
#85932 = CARTESIAN_POINT ( 'NONE',  ( 34.89284013776482851, -285.4894424775635002, -246.6099580098289437 ) ) ;
#85933 = CARTESIAN_POINT ( 'NONE',  ( -37.52390010888706939, -284.4797863188920815, -343.9626527703907755 ) ) ;
#85934 = CARTESIAN_POINT ( 'NONE',  ( -66.61481316073835046, -284.2484963339716728, -337.4245992952517668 ) ) ;
#85935 = CARTESIAN_POINT ( 'NONE',  ( -40.58736291348640179, -293.9914421694584235, -195.0629435506246523 ) ) ;
#85936 = CARTESIAN_POINT ( 'NONE',  ( -9.760655200936342979, -274.7745141898054158, -340.7074054403451555 ) ) ;
#85937 = CARTESIAN_POINT ( 'NONE',  ( -78.83372969306191180, -273.8424907381246953, -205.5216564328746642 ) ) ;
#85938 = CARTESIAN_POINT ( 'NONE',  ( -97.03727617580648257, -288.0016320758110169, -316.6833847914109015 ) ) ;
#85939 = CARTESIAN_POINT ( 'NONE',  ( 5.871282177220538578, -276.4837123355122799, -334.0921007168759047 ) ) ;
#85940 = CARTESIAN_POINT ( 'NONE',  ( 15.49803347003856935, -296.2809052283840288, -323.1577176977123145 ) ) ;
#85941 = CARTESIAN_POINT ( 'NONE',  ( -48.18343439339133027, -254.6019642153539735, -455.9944935231090994 ) ) ;
#85942 = CARTESIAN_POINT ( 'NONE',  ( 209.6916979138304953, 36.36051277703914053, 13.48241519114203690 ) ) ;
#85943 = CARTESIAN_POINT ( 'NONE',  ( -110.0980856356287774, -283.3729883903341147, -259.9807593171267399 ) ) ;
#85944 = CARTESIAN_POINT ( 'NONE',  ( -5.762308662806248982, -278.4672254764807917, -202.3336037881050231 ) ) ;
#85945 = CARTESIAN_POINT ( 'NONE',  ( -57.91589512562487130, -272.2711127407536083, -196.8255166606715818 ) ) ;
#85946 = EDGE_CURVE ( 'NONE', #3443, #35022, #55112, .T. ) ;
#85947 = CARTESIAN_POINT ( 'NONE',  ( -68.08783551814624957, -276.8154440312503084, -336.6965851554475648 ) ) ;
#85948 = CARTESIAN_POINT ( 'NONE',  ( 9.272577327340115971, -294.2258041345485822, -213.2176548307470512 ) ) ;
#85949 = CARTESIAN_POINT ( 'NONE',  ( 35.94350546125161827, -294.4985136184255907, -270.7492459827872153 ) ) ;
#85950 = CARTESIAN_POINT ( 'NONE',  ( -39.07974089614672408, -296.3887040484181625, -346.8482246648846399 ) ) ;
#85951 = CARTESIAN_POINT ( 'NONE',  ( -110.3841501660415929, -296.3709617512534464, -271.4609986234810322 ) ) ;
#85952 = CARTESIAN_POINT ( 'NONE',  ( -20.66039113737006616, -290.8381335202012110, -343.4824867879971748 ) ) ;
#85953 = CARTESIAN_POINT ( 'NONE',  ( -10.70004235915474489, -282.8809172882288294, -342.6619485668637139 ) ) ;
#85954 = CARTESIAN_POINT ( 'NONE',  ( 0.5977476434719330989, -272.6917782151280676, -204.7647994963298572 ) ) ;
#85955 = CARTESIAN_POINT ( 'NONE',  ( -0.9676835456519505829, -286.3547910630731508, -202.4941088972821035 ) ) ;
#85956 = CARTESIAN_POINT ( 'NONE',  ( -74.81773544421018585, -279.5336424865202503, -334.9164708208372190 ) ) ;
#85957 = CARTESIAN_POINT ( 'NONE',  ( -74.83029263721171276, -284.5984229527799130, -207.4483698322567875 ) ) ;
#85958 = VECTOR ( 'NONE', #16116, 1000.000000000000000 ) ;
#85959 = CARTESIAN_POINT ( 'NONE',  ( -26.46055136010997799, -286.9135113292617802, -344.5675951129986174 ) ) ;
#85960 = CARTESIAN_POINT ( 'NONE',  ( 2.709286185474054420, -58.23210827017373248, -348.3322198635470954 ) ) ;
#85961 = CARTESIAN_POINT ( 'NONE',  ( 33.77165796281082777, -286.8381924516382355, -253.5475924985559573 ) ) ;
#85962 = CARTESIAN_POINT ( 'NONE',  ( 9.076082880525564889, -283.3735003560506129, -331.5020178193938705 ) ) ;
#85963 = CARTESIAN_POINT ( 'NONE',  ( -113.4312682712157851, -289.7432163818066329, -259.8137745753052741 ) ) ;
#85964 = CARTESIAN_POINT ( 'NONE',  ( -113.5841242182532227, -280.1364241277045153, -271.6157743956738386 ) ) ;
#85965 = ADVANCED_FACE ( 'NONE', ( #35573 ), #74779, .F. ) ;
#85966 = CARTESIAN_POINT ( 'NONE',  ( -98.19436196449558452, -280.4896675398520074, -223.9689636621413911 ) ) ;
#85967 = CARTESIAN_POINT ( 'NONE',  ( 4.924881791221928040, -280.4747136745269813, -210.8419105168581495 ) ) ;
#85968 = CARTESIAN_POINT ( 'NONE',  ( -8.217062978642150739, -276.4335520214409598, -201.1916585937143509 ) ) ;
#85969 = CARTESIAN_POINT ( 'NONE',  ( -37.68897832448769236, -295.0563522512570103, -347.3734132593388608 ) ) ;
#85970 = CARTESIAN_POINT ( 'NONE',  ( -89.83528364984188386, -287.8177202881306584, -323.4296631904845754 ) ) ;
#85971 = CARTESIAN_POINT ( 'NONE',  ( -16.86142019535844128, -293.9124984013223525, -196.9649426907715508 ) ) ;
#85972 = CARTESIAN_POINT ( 'NONE',  ( -99.00071117008862132, -294.9249251930083915, -310.1075418388273306 ) ) ;
#85973 = ORIENTED_EDGE ( 'NONE', *, *, #48633, .F. ) ;
#85974 = CARTESIAN_POINT ( 'NONE',  ( -53.98836308670775708, -285.1875367435472413, -342.9690516050077349 ) ) ;
#85975 = CARTESIAN_POINT ( 'NONE',  ( -102.5493050419904790, -296.6661474953726838, -237.3843446948425253 ) ) ;
#85976 = CARTESIAN_POINT ( 'NONE',  ( 35.98737601237200323, -294.3486912546890721, -247.9036225248621577 ) ) ;
#85977 = CARTESIAN_POINT ( 'NONE',  ( 21.40594965552208606, -281.5941909678725779, -226.8359576003650204 ) ) ;
#85978 = CARTESIAN_POINT ( 'NONE',  ( 23.45386207502789944, -273.9832646113330838, -223.4705401649432019 ) ) ;
#85979 = CARTESIAN_POINT ( 'NONE',  ( -36.08018398855008968, -289.6881677601465412, -347.2619300671955216 ) ) ;
#85980 = CARTESIAN_POINT ( 'NONE',  ( -2.227978823967796007, -280.7319879563972336, -337.4977850064483960 ) ) ;
#85981 = CARTESIAN_POINT ( 'NONE',  ( -111.6135164223091749, -291.1394980910995969, -250.0764264207907956 ) ) ;
#85982 = CARTESIAN_POINT ( 'NONE',  ( 10.13222925168583544, -288.7098445959157402, -325.9105300489302408 ) ) ;
#85983 = CARTESIAN_POINT ( 'NONE',  ( 140.6539576904058606, 276.0000000000000568, -12.00000000000000178 ) ) ;
#85984 = DIRECTION ( 'NONE',  ( -1.000000000000000000, 0.000000000000000000, 0.000000000000000000 ) ) ;
#85985 = CARTESIAN_POINT ( 'NONE',  ( -21.69536100719032845, -108.9780876184144347, -358.8618341835472734 ) ) ;
#85986 = CARTESIAN_POINT ( 'NONE',  ( -112.3381139276884824, -270.1608578419545097, -261.8788190812425114 ) ) ;
#85987 = CARTESIAN_POINT ( 'NONE',  ( -100.9471620744349849, -278.2433594110846116, -234.2093969009453645 ) ) ;
#85988 = EDGE_LOOP ( 'NONE', ( #64303, #64967, #74614, #29762 ) ) ;
#85989 = CARTESIAN_POINT ( 'NONE',  ( -38.34432427491105955, -278.9596227473332419, -197.0464084888813829 ) ) ;
#85990 = CARTESIAN_POINT ( 'NONE',  ( 31.23338553702003750, -274.7683186972061549, -235.3868143088527063 ) ) ;
#85991 = CARTESIAN_POINT ( 'NONE',  ( 66.61766131416349879, 45.94256429874008063, -316.6294464272367577 ) ) ;
#85992 = CARTESIAN_POINT ( 'NONE',  ( -64.51567692195030190, -278.2791486848208251, -198.8897714850879765 ) ) ;
#85993 = CARTESIAN_POINT ( 'NONE',  ( -15.67870750511635158, -280.7905655471012665, -341.7933344608741209 ) ) ;
#85994 = CARTESIAN_POINT ( 'NONE',  ( -106.2380411386437089, -297.8965983094840340, -302.4121430309786547 ) ) ;
#85995 = PRODUCT_DEFINITION_SHAPE ( 'NONE', 'NONE',  #93718 ) ;
#85996 = CARTESIAN_POINT ( 'NONE',  ( 27.53831140029111779, -293.5880281851692075, -236.7668841686492556 ) ) ;
#85997 = ORIENTED_EDGE ( 'NONE', *, *, #60203, .T. ) ;
#85998 = CARTESIAN_POINT ( 'NONE',  ( -110.1866357209424905, -289.3695290652068479, -260.2447464865329039 ) ) ;
#85999 = CARTESIAN_POINT ( 'NONE',  ( 39.21499083192103541, -276.1061511060821658, -262.5823958574994776 ) ) ;
#86000 = CARTESIAN_POINT ( 'NONE',  ( -59.47564202369844111, -273.7575572872853513, -200.7446383398520311 ) ) ;
#86001 = VERTEX_POINT ( 'NONE', #7599 ) ;
#86002 =( NAMED_UNIT ( * ) PLANE_ANGLE_UNIT ( ) SI_UNIT ( $, .RADIAN. ) );
#86003 = CARTESIAN_POINT ( 'NONE',  ( 219.8344101925596021, 35.72494958537217968, 7.000000000000000000 ) ) ;
#86004 = CARTESIAN_POINT ( 'NONE',  ( -48.18343439339133027, -291.0521521680024080, -430.6442049081568939 ) ) ;
#86005 = CARTESIAN_POINT ( 'NONE',  ( -69.88986283944664990, -280.6927530737937673, -204.6597464184988553 ) ) ;
#86006 = CARTESIAN_POINT ( 'NONE',  ( 7.924666833472360672, -282.4208943661107583, -209.2635198249893165 ) ) ;
#86007 = CARTESIAN_POINT ( 'NONE',  ( -80.77528869267112555, -282.7163288302032242, -329.3897332318655913 ) ) ;
#86008 = CARTESIAN_POINT ( 'NONE',  ( -35.65814349349031431, -281.9338796490721393, -196.1323940554310354 ) ) ;
#86009 = CARTESIAN_POINT ( 'NONE',  ( 14.20257346326613401, -274.7922469214290118, -323.0999522957188788 ) ) ;
#86010 = DIRECTION ( 'NONE',  ( -0.000000000000000000, -0.000000000000000000, 1.000000000000000000 ) ) ;
#86011 = PLANE ( 'NONE',  #20137 ) ;
#86012 = CARTESIAN_POINT ( 'NONE',  ( -107.4246183105436927, -278.9503056384033925, -301.9952054448382910 ) ) ;
#86013 = DIRECTION ( 'NONE',  ( 0.000000000000000000, 0.000000000000000000, 1.000000000000000000 ) ) ;
#86014 = EDGE_LOOP ( 'NONE', ( #87945, #7760, #45004, #22715, #2523 ) ) ;
#86015 = CARTESIAN_POINT ( 'NONE',  ( 185.4166944662832179, 215.0000000000000568, 22.87680765314684095 ) ) ;
#86016 = CARTESIAN_POINT ( 'NONE',  ( -89.28568953398718122, -285.7583477470764137, -325.0241125775010573 ) ) ;
#86017 = CARTESIAN_POINT ( 'NONE',  ( 34.99606262804381629, -292.8977476760435366, -281.6379359963180491 ) ) ;
#86018 = CARTESIAN_POINT ( 'NONE',  ( 37.72362617664776963, -287.1104858160874187, -287.1098099827382271 ) ) ;
#86019 = CARTESIAN_POINT ( 'NONE',  ( -96.56347389551022786, -283.4066579724055828, -225.9679256277046591 ) ) ;
#86021 = CARTESIAN_POINT ( 'NONE',  ( 6.426059300490751802, -286.6886229282208660, -330.1104613063091051 ) ) ;
#86020 = CARTESIAN_POINT ( 'NONE',  ( -110.4603487888587665, -283.0123786079946058, -279.1105376037121459 ) ) ;
#86022 = AXIS2_PLACEMENT_3D ( 'NONE', #52276, #23862, #16299 ) ;
#86023 = CARTESIAN_POINT ( 'NONE',  ( 19.67013053928295818, -283.4079134921353216, -316.6062690709638900 ) ) ;
#86024 = CARTESIAN_POINT ( 'NONE',  ( -41.06725506839342188, -272.0052366240666970, -195.4027992210114633 ) ) ;
#86025 = CARTESIAN_POINT ( 'NONE',  ( -106.2905221562944860, -282.5321262878493940, -302.8033798383515318 ) ) ;
#86026 = CARTESIAN_POINT ( 'NONE',  ( -110.3528192457910961, -298.3312968219668164, -287.5740104511055506 ) ) ;
#86027 = CARTESIAN_POINT ( 'NONE',  ( -0.5898072669017507819, -284.5390993879458392, -204.7771743594223040 ) ) ;
#86028 = CARTESIAN_POINT ( 'NONE',  ( -66.17333680887702485, -280.6065328909930940, -203.0262249094810727 ) ) ;
#86029 = CARTESIAN_POINT ( 'NONE',  ( 37.52379666896567301, -289.6384337980255168, -277.0831574094953567 ) ) ;
#86030 = CARTESIAN_POINT ( 'NONE',  ( 197.1711655576864644, 291.5339772727334662, -7.625735220792024371 ) ) ;
#86031 = DIRECTION ( 'NONE',  ( 0.000000000000000000, 0.000000000000000000, -1.000000000000000000 ) ) ;
#86032 = CARTESIAN_POINT ( 'NONE',  ( 32.10296191605898741, -295.8603212217515761, -300.2717559984726563 ) ) ;
#86033 = CARTESIAN_POINT ( 'NONE',  ( -71.38271542569091821, -275.5015684762772707, -337.1908264198191887 ) ) ;
#86034 = CARTESIAN_POINT ( 'NONE',  ( -97.33107391121868091, -290.3938534175048858, -222.3461843208778532 ) ) ;
#86035 = CARTESIAN_POINT ( 'NONE',  ( 23.58201381024364807, -292.5263730467446521, -312.1006772726630061 ) ) ;
#86036 = CARTESIAN_POINT ( 'NONE',  ( -46.50142708007193448, -278.6184389651788251, -197.3895586899560328 ) ) ;
#86037 = CARTESIAN_POINT ( 'NONE',  ( -33.71316256091402153, -296.2376274846301385, -196.1270752847585186 ) ) ;
#86038 = CARTESIAN_POINT ( 'NONE',  ( -102.8567301656565860, -292.3179145393797285, -236.9463972831280500 ) ) ;
#86039 = CARTESIAN_POINT ( 'NONE',  ( -69.91165696735023971, -276.1233781216988064, -202.8022627189028810 ) ) ;
#86040 = CARTESIAN_POINT ( 'NONE',  ( 6.202332008376906458, -292.9531029290223501, -333.0882781293727248 ) ) ;
#86041 = CARTESIAN_POINT ( 'NONE',  ( -97.19563393301493193, -291.5550159112387405, -313.5345707563162136 ) ) ;
#86042 = CARTESIAN_POINT ( 'NONE',  ( -47.58431480887909260, -290.1636540129537138, -195.0148536498188037 ) ) ;
#86043 = CARTESIAN_POINT ( 'NONE',  ( -37.24920246201178031, -290.4762459037178814, -343.9502908503229150 ) ) ;
#86044 = DIRECTION ( 'NONE',  ( 0.000000000000000000, 1.000000000000000000, -0.000000000000000000 ) ) ;
#86045 = CARTESIAN_POINT ( 'NONE',  ( -3.282106225573130587, -289.3934417777558679, -335.1671021484442008 ) ) ;
#86046 = DIRECTION ( 'NONE',  ( 0.000000000000000000, 0.000000000000000000, -1.000000000000000000 ) ) ;
#86047 = CARTESIAN_POINT ( 'NONE',  ( -95.14852368630150181, -291.0742752973205256, -320.6242244272600033 ) ) ;
#86049 = CARTESIAN_POINT ( 'NONE',  ( -107.7258078396471177, -290.2940394252267424, -289.9143129309625238 ) ) ;
#86048 = CARTESIAN_POINT ( 'NONE',  ( 37.04014140497751839, -279.7275698075816308, -282.5141891068121254 ) ) ;
#86050 = CARTESIAN_POINT ( 'NONE',  ( -71.22911091300672126, -279.9502438134891804, -201.2424686760486168 ) ) ;
#86051 = CARTESIAN_POINT ( 'NONE',  ( 39.68930748857101065, -281.2135362459235921, -269.9346225428723187 ) ) ;
#86052 = CARTESIAN_POINT ( 'NONE',  ( 37.10650904063178501, -285.6685888660213095, -279.4421311190098436 ) ) ;
#86053 = FACE_OUTER_BOUND ( 'NONE', #58330, .T. ) ;
#86054 = CARTESIAN_POINT ( 'NONE',  ( 33.40130573111337497, -279.9870673443629130, -293.0293091108346744 ) ) ;
#86055 = CARTESIAN_POINT ( 'NONE',  ( -29.64225779535219019, -284.1495032150146471, -195.7573698474652986 ) ) ;
#86056 = DIRECTION ( 'NONE',  ( -0.8043439146810398288, 0.5941640067486249066, 0.000000000000000000 ) ) ;
#86057 = CARTESIAN_POINT ( 'NONE',  ( -99.67137328458505863, -277.6198250861004340, -226.3415814388513070 ) ) ;
#86058 = CARTESIAN_POINT ( 'NONE',  ( -23.82681155051151123, -285.1411338649730283, -194.8164535336805159 ) ) ;
#86059 = CARTESIAN_POINT ( 'NONE',  ( -85.42396705455898598, -274.1704161940028257, -215.1510692774234315 ) ) ;
#86060 = CARTESIAN_POINT ( 'NONE',  ( -5.802570524182329770, -229.5268262511776527, 22.50000000000000000 ) ) ;
#86061 = CARTESIAN_POINT ( 'NONE',  ( -65.65249300661895404, -293.2757740169525960, -202.1936613908745244 ) ) ;
#86062 = CARTESIAN_POINT ( 'NONE',  ( 37.63703529265601588, -276.7918553247759519, -255.6371399502399981 ) ) ;
#86063 = CARTESIAN_POINT ( 'NONE',  ( -108.7863419446854465, -278.0198468780952794, -285.4525275443737655 ) ) ;
#86064 = CARTESIAN_POINT ( 'NONE',  ( -68.09256332694990022, -297.4560484384575716, -338.7812279068012913 ) ) ;
#86065 = CARTESIAN_POINT ( 'NONE',  ( -88.65106368238826917, -291.5219679919231908, -212.9472763053174162 ) ) ;
#86066 = CARTESIAN_POINT ( 'NONE',  ( 28.05278311732715579, -279.1303846559010822, -232.5077725953603931 ) ) ;
#86067 = CARTESIAN_POINT ( 'NONE',  ( 1.701931895804736472, -292.3921144411266937, -203.9330621178176273 ) ) ;
#86068 = ADVANCED_FACE ( 'NONE', ( #92844 ), #10097, .F. ) ;
#86069 = CARTESIAN_POINT ( 'NONE',  ( -86.07669835838689210, -290.4157470530197998, -215.6274482700807482 ) ) ;
#86070 = CARTESIAN_POINT ( 'NONE',  ( -87.29289316236092588, -293.7478560305256110, -326.3761031373976493 ) ) ;
#86071 = ORIENTED_EDGE ( 'NONE', *, *, #38265, .F. ) ;
#86072 = CARTESIAN_POINT ( 'NONE',  ( 153.2628468892467311, 20.37991841447510311, 11.93555113920849386 ) ) ;
#86073 = CARTESIAN_POINT ( 'NONE',  ( 19.39754396006932069, -292.4089328173803892, -224.3125701546319704 ) ) ;
#86074 = DIRECTION ( 'NONE',  ( 0.000000000000000000, 0.000000000000000000, -1.000000000000000000 ) ) ;
#86075 = CARTESIAN_POINT ( 'NONE',  ( -105.5795714935544112, -276.2666405000204009, -254.7536222014695397 ) ) ;
#86076 = CARTESIAN_POINT ( 'NONE',  ( -94.48446673430025555, -294.9131301214216592, -321.6400900069639874 ) ) ;
#86077 = CARTESIAN_POINT ( 'NONE',  ( -113.3317776220491169, -285.9790618700961318, -261.4838213963163298 ) ) ;
#86078 = CARTESIAN_POINT ( 'NONE',  ( 26.36841721611366296, -286.8967647944322152, -234.6203349706351275 ) ) ;
#86079 = CARTESIAN_POINT ( 'NONE',  ( 19.73073150001051701, -277.7263312491641614, -317.0012339431818873 ) ) ;
#86080 = CARTESIAN_POINT ( 'NONE',  ( -41.14774837607774316, -293.1203714731076957, -344.9216765362599517 ) ) ;
#86081 = CARTESIAN_POINT ( 'NONE',  ( -53.34696732310778344, -297.0202432051246433, -342.6758818495331411 ) ) ;
#86082 = CARTESIAN_POINT ( 'NONE',  ( 29.50964426273811725, -274.7532410796671911, -300.6600991005429364 ) ) ;
#86083 = ORIENTED_EDGE ( 'NONE', *, *, #65006, .T. ) ;
#86084 = CARTESIAN_POINT ( 'NONE',  ( 195.4394726684814145, 39.61210057291198439, 13.99041345891462207 ) ) ;
#86085 = CARTESIAN_POINT ( 'NONE',  ( -113.9226162255255588, -296.1210810376899758, -278.1782518018537189 ) ) ;
#86086 = CARTESIAN_POINT ( 'NONE',  ( 36.39000885337114255, -289.6060405823153587, -280.6986184847754089 ) ) ;
#86087 = CARTESIAN_POINT ( 'NONE',  ( -82.24831055652813916, -295.4397336948744055, -210.2272085308262035 ) ) ;
#86088 = CARTESIAN_POINT ( 'NONE',  ( -111.4381795210764636, -274.0040958469344332, -250.7229238802001134 ) ) ;
#86089 = ADVANCED_FACE ( 'NONE', ( #64487 ), #42172, .T. ) ;
#86090 = CARTESIAN_POINT ( 'NONE',  ( 34.11207735671815300, -288.4076269515787772, -285.8552187274494258 ) ) ;
#86091 = ORIENTED_EDGE ( 'NONE', *, *, #70625, .T. ) ;
#86092 = CARTESIAN_POINT ( 'NONE',  ( 20.89544887160410624, -279.9336132315721102, -220.3285809885624644 ) ) ;
#86093 = CARTESIAN_POINT ( 'NONE',  ( 13.33489418193412135, -295.0166845592861478, -328.2693917963862873 ) ) ;
#86094 = CARTESIAN_POINT ( 'NONE',  ( -45.90999735546880345, -287.2991386654720714, -345.6921402247899096 ) ) ;
#86095 = AXIS2_PLACEMENT_3D ( 'NONE', #5505, #91648, #62324 ) ;
#86096 = CARTESIAN_POINT ( 'NONE',  ( -110.7783481901860512, -296.5948012587943481, -293.4877565563230064 ) ) ;
#86097 = CARTESIAN_POINT ( 'NONE',  ( 24.44741286264731173, -294.4239320862337763, -309.3687407585708229 ) ) ;
#86098 = DIRECTION ( 'NONE',  ( -1.000000000000000000, 8.666672153582269122E-16, 0.000000000000000000 ) ) ;
#86099 = CARTESIAN_POINT ( 'NONE',  ( 196.2205576190423528, 72.73813141077837940, -11.64668355651677345 ) ) ;
#86100 = CIRCLE ( 'NONE', #15076, 1.000000000000000888 ) ;
#86101 = CARTESIAN_POINT ( 'NONE',  ( 17.83663475847049185, -288.3442335507815528, -217.5776389324969387 ) ) ;
#86102 = CARTESIAN_POINT ( 'NONE',  ( -115.3430155898818299, -287.8380690714489560, -288.1317622949166548 ) ) ;
#86103 = CARTESIAN_POINT ( 'NONE',  ( -96.73340544276445030, -278.5579604239187574, -221.4945787034614568 ) ) ;
#86104 = CARTESIAN_POINT ( 'NONE',  ( -103.3773380151498316, -286.0830144249798650, -305.6753559689226449 ) ) ;
#86105 = CARTESIAN_POINT ( 'NONE',  ( -112.4158320185101019, -283.3096379623122516, -255.8565894072962124 ) ) ;
#86106 = CARTESIAN_POINT ( 'NONE',  ( -66.92333195810844870, -287.5225718509133799, -338.7261009155925535 ) ) ;
#86107 = CARTESIAN_POINT ( 'NONE',  ( 34.04525718381081134, -277.7398830232373257, -295.8971462202514999 ) ) ;
#86108 = CARTESIAN_POINT ( 'NONE',  ( -38.08683333091465073, -274.3758427936994622, -197.3437757727656390 ) ) ;
#86109 = EDGE_LOOP ( 'NONE', ( #45445, #69432, #79147, #38355 ) ) ;
#86111 = CARTESIAN_POINT ( 'NONE',  ( -43.75177264073350614, -279.3177332950034497, -197.4904620580578296 ) ) ;
#86110 = CARTESIAN_POINT ( 'NONE',  ( -100.5828336845994926, -278.0509698189387677, -306.9257599442761943 ) ) ;
#86112 = CARTESIAN_POINT ( 'NONE',  ( 37.91276418562804196, -276.4463103103168464, -255.5875567493712879 ) ) ;
#86113 = CARTESIAN_POINT ( 'NONE',  ( -88.65403744635321459, -278.1457016105900379, -213.4835938050755146 ) ) ;
#86114 = CARTESIAN_POINT ( 'NONE',  ( -110.1644982457800950, -264.2653545926315815, -305.9146289097863587 ) ) ;
#86115 = CARTESIAN_POINT ( 'NONE',  ( -34.12508696023863308, -275.0329281710281180, -193.6638324167203677 ) ) ;
#86116 = CARTESIAN_POINT ( 'NONE',  ( -89.22166260746922717, -298.7647503922274836, -214.1906224796564686 ) ) ;
#86117 = CARTESIAN_POINT ( 'NONE',  ( -85.33152481854864391, -287.9090924074130839, -210.2361428286349110 ) ) ;
#86118 = ORIENTED_EDGE ( 'NONE', *, *, #80845, .F. ) ;
#86119 = CARTESIAN_POINT ( 'NONE',  ( 82.67040237643779221, -297.8655364536941192, -193.5104719492758534 ) ) ;
#86120 = CARTESIAN_POINT ( 'NONE',  ( -37.29442038879642496, -287.1323945636266330, -197.0395286248191269 ) ) ;
#86121 = CARTESIAN_POINT ( 'NONE',  ( -26.78436490224498456, -287.9446623775103831, -195.0586287482441037 ) ) ;
#86122 = CARTESIAN_POINT ( 'NONE',  ( -8.185453708454760502, -288.0086602811940111, -337.4510853134514150 ) ) ;
#86123 = CARTESIAN_POINT ( 'NONE',  ( -114.2791973961366381, -284.0646278548166492, -269.9758684761570180 ) ) ;
#86124 = CARTESIAN_POINT ( 'NONE',  ( 15.84997504353883180, -279.2207327176601552, -219.1306275434438646 ) ) ;
#86125 = CARTESIAN_POINT ( 'NONE',  ( 11.93659908474737641, -288.6056069137401323, -214.7716727209824796 ) ) ;
#86126 = CARTESIAN_POINT ( 'NONE',  ( 36.11848389631552436, -280.1165700371992102, -276.8310959455851048 ) ) ;
#86127 = CARTESIAN_POINT ( 'NONE',  ( -71.87116892264261026, -278.8337864708252027, -335.2518038767208282 ) ) ;
#86128 = CARTESIAN_POINT ( 'NONE',  ( 25.32538962088364087, -275.5271033796352071, -232.7021973823910344 ) ) ;
#86129 = CARTESIAN_POINT ( 'NONE',  ( -48.82470790767777657, -287.9900854451622081, -346.1521558340440379 ) ) ;
#86130 = CARTESIAN_POINT ( 'NONE',  ( -95.20638058971513829, -284.6697830466758887, -320.9164102463781774 ) ) ;
#86131 = CARTESIAN_POINT ( 'NONE',  ( -103.9902869537412187, -285.5457813836982837, -231.8169880328766794 ) ) ;
#86132 = CARTESIAN_POINT ( 'NONE',  ( -32.96513488466632680, -280.2755050470740343, -197.4924300488215181 ) ) ;
#86133 = VERTEX_POINT ( 'NONE', #7153 ) ;
#86134 = ORIENTED_EDGE ( 'NONE', *, *, #13000, .T. ) ;
#86135 = CARTESIAN_POINT ( 'NONE',  ( 175.2296996224750103, 154.6894116713782807, 0.000000000000000000 ) ) ;
#86136 = CARTESIAN_POINT ( 'NONE',  ( -20.74355520701342215, -290.7018384893760867, -344.3392457607394022 ) ) ;
#86137 = CARTESIAN_POINT ( 'NONE',  ( -109.4067231409171370, -288.9088678022301906, -296.2073931386224785 ) ) ;
#86138 = CARTESIAN_POINT ( 'NONE',  ( -35.80106934112821904, -297.2690894033805193, -197.1998569180037180 ) ) ;
#86139 = CARTESIAN_POINT ( 'NONE',  ( 38.50436707897962663, -293.0604840223909378, -283.1170848790582113 ) ) ;
#86140 = CARTESIAN_POINT ( 'NONE',  ( -100.9117533263498672, -288.5238210972671595, -307.7384181341246858 ) ) ;
#86141 = CARTESIAN_POINT ( 'NONE',  ( 15.61602450727186842, -291.0535285914015162, -218.5822398014605028 ) ) ;
#86142 = CARTESIAN_POINT ( 'NONE',  ( 22.30534611916144172, -288.1616042857082221, -227.5044311724007002 ) ) ;
#86143 = CARTESIAN_POINT ( 'NONE',  ( -106.6379572354042296, -298.6233781216988632, -303.7686719486574702 ) ) ;
#86144 = CARTESIAN_POINT ( 'NONE',  ( 17.20810894700035476, -290.2739087980491490, -321.8326535991022297 ) ) ;
#86145 = CARTESIAN_POINT ( 'NONE',  ( -112.5341989671727276, -288.5774064229840974, -268.3770677680075210 ) ) ;
#86146 = CARTESIAN_POINT ( 'NONE',  ( 25.64437005843412010, -295.0025391302986577, -229.5513966709449676 ) ) ;
#86147 = CARTESIAN_POINT ( 'NONE',  ( -66.64273944772145342, -284.3868933692981500, -337.4929671033554541 ) ) ;
#86148 = CARTESIAN_POINT ( 'NONE',  ( -36.42689401635930579, -294.0637537354376718, -195.1872923611722399 ) ) ;
#86149 = CARTESIAN_POINT ( 'NONE',  ( 200.9021118020844199, 65.55478020308605380, -5.267193185415704804 ) ) ;
#86150 = DIRECTION ( 'NONE',  ( 1.000000000000000000, 0.000000000000000000, -0.000000000000000000 ) ) ;
#86151 = CARTESIAN_POINT ( 'NONE',  ( -93.86968991500313564, -275.2214292982374673, -220.5314764505885989 ) ) ;
#86152 = CARTESIAN_POINT ( 'NONE',  ( -4.764424252452510444, -281.8088180449574338, -335.8693069671070361 ) ) ;
#86153 = CARTESIAN_POINT ( 'NONE',  ( -56.86336323362571932, -281.3037452274124917, -342.7759321814564260 ) ) ;
#86154 = CARTESIAN_POINT ( 'NONE',  ( -90.60752007190234281, -294.9807912191776609, -325.8140828105549076 ) ) ;
#86155 = CARTESIAN_POINT ( 'NONE',  ( 33.84071785070673144, -273.5254679055530573, -249.9037296140886042 ) ) ;
#86156 = CARTESIAN_POINT ( 'NONE',  ( -109.6834144956224435, -276.8590689206492925, -252.8114580486227680 ) ) ;
#86157 = CARTESIAN_POINT ( 'NONE',  ( -40.55619145982202411, -299.3260977906836615, -196.9256643758872940 ) ) ;
#86158 = CARTESIAN_POINT ( 'NONE',  ( -38.33216272160166938, -296.4900824633626826, -343.9436831916700044 ) ) ;
#86159 = CARTESIAN_POINT ( 'NONE',  ( -58.44506725044026041, -296.1349072988235775, -340.4128818623713073 ) ) ;
#86160 = AXIS2_PLACEMENT_3D ( 'NONE', #19926, #34611, #32 ) ;
#86161 = LINE ( 'NONE', #944, #35435 ) ;
#86163 = CARTESIAN_POINT ( 'NONE',  ( -103.2041632951744816, -272.8112449056056903, -238.8788062814458613 ) ) ;
#86162 = CARTESIAN_POINT ( 'NONE',  ( 35.19415275998125026, -285.8342903664088794, -290.8279026627391204 ) ) ;
#86164 = CARTESIAN_POINT ( 'NONE',  ( -57.75593441690234187, -285.7957310267324260, -196.0611770603912873 ) ) ;
#86165 = AXIS2_PLACEMENT_3D ( 'NONE', #80685, #73133, #89167 ) ;
#86166 = CARTESIAN_POINT ( 'NONE',  ( 35.92632655596987235, -287.5158921112999906, -293.9734147224672256 ) ) ;
#86167 = CARTESIAN_POINT ( 'NONE',  ( 20.12990833785845979, -296.2033045184735442, -319.0994091516115532 ) ) ;
#86168 = CARTESIAN_POINT ( 'NONE',  ( -16.90812760216920907, -290.3163318977087783, -198.3176333113612770 ) ) ;
#86169 = CARTESIAN_POINT ( 'NONE',  ( -104.6472122639550975, -278.2304726642655055, -233.2919008856500511 ) ) ;
#86170 = CARTESIAN_POINT ( 'NONE',  ( -106.6379572354042153, -294.4809262143061801, -236.9535640164627068 ) ) ;
#86171 = DIRECTION ( 'NONE',  ( 0.000000000000000000, 0.000000000000000000, -1.000000000000000000 ) ) ;
#86172 = CARTESIAN_POINT ( 'NONE',  ( -22.36389268175464906, -285.0430125300786699, -198.4563551109906427 ) ) ;
#86173 = DIRECTION ( 'NONE',  ( 0.000000000000000000, 0.000000000000000000, 1.000000000000000000 ) ) ;
#86174 = CARTESIAN_POINT ( 'NONE',  ( 17.45526775019607157, -286.2696054490617144, -321.6454079059366791 ) ) ;
#86175 = CARTESIAN_POINT ( 'NONE',  ( -109.9252799767938882, -297.9772494752605212, -283.7750955080324502 ) ) ;
#86176 = CARTESIAN_POINT ( 'NONE',  ( 19.67680657382954834, -282.2822394614445329, -219.4740122644367091 ) ) ;
#86178 = CARTESIAN_POINT ( 'NONE',  ( 15.82586250214500190, -282.2729679662205058, -320.4561446309208463 ) ) ;
#86177 = CARTESIAN_POINT ( 'NONE',  ( -111.5155592359047176, -294.7421101762478770, -257.0703155336096870 ) ) ;
#86179 = CARTESIAN_POINT ( 'NONE',  ( -93.66420143866248793, -297.4352792401255101, -217.7783341986134360 ) ) ;
#86180 = CARTESIAN_POINT ( 'NONE',  ( -58.11861974492182270, -299.2988921375849714, -199.6573177866117135 ) ) ;
#86181 = CARTESIAN_POINT ( 'NONE',  ( -24.01538492022355342, -284.3007864750705949, -195.9323548680586384 ) ) ;
#86182 = CARTESIAN_POINT ( 'NONE',  ( 22.96791733772884925, -282.9439607885518626, -225.7769201937584000 ) ) ;
#86183 = ADVANCED_FACE ( 'NONE', ( #65403 ), #29398, .T. ) ;
#86184 = CARTESIAN_POINT ( 'NONE',  ( -71.76503134961998853, -296.6442213188000210, -205.7060004631101435 ) ) ;
#86185 = PLANE ( 'NONE',  #86160 ) ;
#86186 = CARTESIAN_POINT ( 'NONE',  ( 10.99251291554320531, -284.3597662237326062, -327.3118916594960979 ) ) ;
#86187 = PLANE ( 'NONE',  #88211 ) ;
#86188 = CARTESIAN_POINT ( 'NONE',  ( -4.771743288812454686, -283.9809262143061233, -202.8022627189028810 ) ) ;
#86189 = CARTESIAN_POINT ( 'NONE',  ( -9.280330824044447979, -275.8916553472793680, -341.8923585232664664 ) ) ;
#86190 = CARTESIAN_POINT ( 'NONE',  ( 33.30873927388111611, -293.1429268588723858, -251.9895253233305255 ) ) ;
#86191 = CARTESIAN_POINT ( 'NONE',  ( 36.39683177973545725, -283.0845964549790210, -271.3034874255757813 ) ) ;
#86192 = CARTESIAN_POINT ( 'NONE',  ( 24.66752478077172839, -277.7013424890029683, -310.4715864164873551 ) ) ;
#86193 = CARTESIAN_POINT ( 'NONE',  ( 24.47041098687520133, -283.7495474760008278, -314.9445061380191078 ) ) ;
#86194 = CARTESIAN_POINT ( 'NONE',  ( 25.48407149801997917, -279.8263985856398222, -232.3145633146270086 ) ) ;
#86195 = CARTESIAN_POINT ( 'NONE',  ( -86.39459255855943809, -279.7328562797914060, -327.1644876568187783 ) ) ;
#86196 = CARTESIAN_POINT ( 'NONE',  ( -88.03796645749240213, -273.5327425011998912, -212.3343077688948597 ) ) ;
#86197 = CARTESIAN_POINT ( 'NONE',  ( 39.13732681666608215, -275.5028936208451569, -279.7500034866696978 ) ) ;
#86198 = CARTESIAN_POINT ( 'NONE',  ( 18.17042474618121872, -296.1681744956499642, -319.9758897439148768 ) ) ;
#86199 = DIRECTION ( 'NONE',  ( 1.000000000000000000, 0.000000000000000000, 0.000000000000000000 ) ) ;
#86200 = EDGE_CURVE ( 'NONE', #92063, #43035, #15182, .T. ) ;
#86201 = ADVANCED_FACE ( 'NONE', ( #32177, #24130 ), #17038, .F. ) ;
#86202 = FACE_OUTER_BOUND ( 'NONE', #57292, .T. ) ;
#86203 = CARTESIAN_POINT ( 'NONE',  ( -6.325381000752239302, -292.7886205270276605, -339.4863191114410483 ) ) ;
#86204 = CARTESIAN_POINT ( 'NONE',  ( -94.65708692226107246, -272.6986586816919385, -225.0517935722931497 ) ) ;
#86205 = CARTESIAN_POINT ( 'NONE',  ( 37.67920192702032267, -295.2491966612953433, -284.3807215967667616 ) ) ;
#86206 = CARTESIAN_POINT ( 'NONE',  ( -3.510615814643709864, -293.6938456423344519, -201.6191773866841572 ) ) ;
#86207 = CARTESIAN_POINT ( 'NONE',  ( 11.32643419548897690, -290.3764556524163254, -327.2754204920393022 ) ) ;
#86208 = CARTESIAN_POINT ( 'NONE',  ( -111.3079346288414797, -276.4058186468024587, -281.7200167399190036 ) ) ;
#86209 = CARTESIAN_POINT ( 'NONE',  ( -37.79445049122723077, -278.9779828916521183, -344.8124441003350853 ) ) ;
#86210 = CARTESIAN_POINT ( 'NONE',  ( 36.25802797991327253, -291.7806065219150469, -281.8489001126035305 ) ) ;
#86211 = CARTESIAN_POINT ( 'NONE',  ( 22.75287375769195819, -282.7867761770912125, -224.1994110275627747 ) ) ;
#86212 = CARTESIAN_POINT ( 'NONE',  ( -97.60222871350218554, -284.0519490281568551, -228.5909432129838592 ) ) ;
#86213 = ORIENTED_EDGE ( 'NONE', *, *, #6688, .T. ) ;
#86214 = CARTESIAN_POINT ( 'NONE',  ( -6.027726585028406525, -282.2956631670616048, -336.3409431835260079 ) ) ;
#86215 = CARTESIAN_POINT ( 'NONE',  ( -59.22713662753947972, -280.8549902806670957, -196.8592800582860605 ) ) ;
#86216 = CARTESIAN_POINT ( 'NONE',  ( -111.9694047518493818, -283.5643574802977582, -253.0777611559296645 ) ) ;
#86217 = CARTESIAN_POINT ( 'NONE',  ( -88.78268009777688974, -280.2916837429551720, -213.3817726710100260 ) ) ;
#86218 = SHAPE_REPRESENTATION_RELATIONSHIP ( 'NONE' , 'NONE' ,  #71246, #67884 ) ;
#86219 = CARTESIAN_POINT ( 'NONE',  ( -110.0004737996372484, -279.7745651005986360, -293.8422694156296302 ) ) ;
#86220 = VECTOR ( 'NONE', #51025, 1000.000000000000000 ) ;
#86221 = CARTESIAN_POINT ( 'NONE',  ( 30.91033621190086578, -272.8380690714490129, -254.8156830097664738 ) ) ;
#86222 = EDGE_LOOP ( 'NONE', ( #23080, #52889 ) ) ;
#86223 = ORIENTED_EDGE ( 'NONE', *, *, #16074, .F. ) ;
#86224 = CARTESIAN_POINT ( 'NONE',  ( -44.79244279979960908, -299.9581344513669592, -195.6803591188261748 ) ) ;
#86225 = CARTESIAN_POINT ( 'NONE',  ( -103.6046354759887294, -277.0306810199793404, -235.8819947378720769 ) ) ;
#86226 = CARTESIAN_POINT ( 'NONE',  ( -113.1002435367726093, -292.2295619153871371, -276.8891450780491255 ) ) ;
#86227 = CARTESIAN_POINT ( 'NONE',  ( 21.08025679689979626, -292.2845690747449225, -226.4206171030940595 ) ) ;
#86228 = CARTESIAN_POINT ( 'NONE',  ( -85.13136277130155349, -289.1992434005931614, -330.7256556792448237 ) ) ;
#86230 = CARTESIAN_POINT ( 'NONE',  ( -81.94607671668215687, -283.8324531741836267, -211.5657950205414863 ) ) ;
#86229 = CARTESIAN_POINT ( 'NONE',  ( 3.893926359213578881, -293.0836886467742488, -334.7524764141869582 ) ) ;
#86231 = CARTESIAN_POINT ( 'NONE',  ( 5.192298025046579113, -294.4942150562570191, -209.4563189778400840 ) ) ;
#86232 = CARTESIAN_POINT ( 'NONE',  ( -70.42199879455813516, -284.8128070399175726, -336.0024501790110776 ) ) ;
#86233 = CARTESIAN_POINT ( 'NONE',  ( -75.53617671055729943, -290.4900433667446578, -336.9494215471587495 ) ) ;
#86234 = CARTESIAN_POINT ( 'NONE',  ( 13.37331014679241470, -281.2771943455525161, -217.6980724941505798 ) ) ;
#86235 = CARTESIAN_POINT ( 'NONE',  ( -3.418501215188087361, -293.4092539862115814, -339.0577049524756603 ) ) ;
#86236 = CARTESIAN_POINT ( 'NONE',  ( -28.98455913964636110, -289.7517491222019430, -346.7972331871446272 ) ) ;
#86237 = CARTESIAN_POINT ( 'NONE',  ( -114.3284783354898480, -291.0335691076958256, -271.2343218690337494 ) ) ;
#86238 = CARTESIAN_POINT ( 'NONE',  ( -94.12338067925827545, -285.3678566380152688, -224.4627619973549599 ) ) ;
#86239 = VERTEX_POINT ( 'NONE', #2378 ) ;
#86240 = DIRECTION ( 'NONE',  ( 0.000000000000000000, 0.000000000000000000, 1.000000000000000000 ) ) ;
#86241 = CARTESIAN_POINT ( 'NONE',  ( 38.27119546791247018, -295.4832801221733121, -275.9244634561154612 ) ) ;
#86242 = CARTESIAN_POINT ( 'NONE',  ( -95.21947267962707429, -294.5567454004556680, -320.3957231897343831 ) ) ;
#86243 = CARTESIAN_POINT ( 'NONE',  ( -97.08456464264504859, -277.0210967274819041, -312.7408837310269405 ) ) ;
#86244 = CARTESIAN_POINT ( 'NONE',  ( -112.3818752669307770, -272.2724018801275747, -253.3758591171066428 ) ) ;
#86245 = CARTESIAN_POINT ( 'NONE',  ( -42.45699264858786393, -293.5977107771991541, -343.8767050057956567 ) ) ;
#86246 = CARTESIAN_POINT ( 'NONE',  ( 19.76663549657548202, -276.6541510874912433, -223.2802087053597120 ) ) ;
#86247 = CARTESIAN_POINT ( 'NONE',  ( -90.10370680157242873, -271.4361236336774255, -218.1400864786699572 ) ) ;
#86248 = CARTESIAN_POINT ( 'NONE',  ( 33.50398087846112816, -295.0098380923572563, -289.5927894746005791 ) ) ;
#86249 = CARTESIAN_POINT ( 'NONE',  ( -45.10987807316766407, -296.2323717831378076, -343.3081831533322656 ) ) ;
#86250 = DIRECTION ( 'NONE',  ( 0.000000000000000000, 0.000000000000000000, -1.000000000000000000 ) ) ;
#86251 = CARTESIAN_POINT ( 'NONE',  ( -111.3299248788238458, -294.7218451599225659, -257.1032513837006377 ) ) ;
#86252 = CARTESIAN_POINT ( 'NONE',  ( -29.08157330243599148, -298.8044349271120836, -193.4621639557767878 ) ) ;
#86253 = CARTESIAN_POINT ( 'NONE',  ( -5.554209228260244657, -287.2003123869359342, -336.7307672317078300 ) ) ;
#86254 = CARTESIAN_POINT ( 'NONE',  ( 185.8821869067168393, 215.0000000000000568, 23.16839473634431101 ) ) ;
#86255 = CARTESIAN_POINT ( 'NONE',  ( -108.6593436259732073, -291.7130528629631385, -253.6570019851597806 ) ) ;
#86256 = CARTESIAN_POINT ( 'NONE',  ( -76.40688607295069801, -274.0371025460335090, -204.0165398843044215 ) ) ;
#86257 = CARTESIAN_POINT ( 'NONE',  ( -103.7395839019881834, -297.2965861191769932, -239.8517604270988954 ) ) ;
#86258 = CARTESIAN_POINT ( 'NONE',  ( -112.7327660307813915, -280.5520720423783132, -268.7941583936683969 ) ) ;
#86259 = CARTESIAN_POINT ( 'NONE',  ( 38.69462698084842600, -280.1244932509795262, -261.4243086426562286 ) ) ;
#86260 = ORIENTED_EDGE ( 'NONE', *, *, #47247, .F. ) ;
#86261 = CARTESIAN_POINT ( 'NONE',  ( -44.41810874856214042, -282.4878974926833735, -346.9861833074120909 ) ) ;
#86262 = CARTESIAN_POINT ( 'NONE',  ( 39.52918617465833506, -274.8751380959097901, -268.3167047885119132 ) ) ;
#86263 = CARTESIAN_POINT ( 'NONE',  ( -28.29949838904284221, -278.5647978780119161, -194.6464405584155770 ) ) ;
#86264 = CARTESIAN_POINT ( 'NONE',  ( 9.696073623395134788, -278.6971356703135712, -211.6643909721984471 ) ) ;
#86265 = EDGE_CURVE ( 'NONE', #69489, #84890, #55180, .T. ) ;
#86266 = CARTESIAN_POINT ( 'NONE',  ( -47.32326030969229436, -296.6076257106947196, -197.4973938920623766 ) ) ;
#86267 = CARTESIAN_POINT ( 'NONE',  ( -5.529903706810583408, -276.4707196843591532, -202.4280579822565187 ) ) ;
#86268 = CARTESIAN_POINT ( 'NONE',  ( 153.9133111279456045, 20.47222690886501439, 13.06183683676589524 ) ) ;
#86269 = CARTESIAN_POINT ( 'NONE',  ( 21.83248970208357420, -290.9344367090293986, -223.6840633000784919 ) ) ;
#86270 = CARTESIAN_POINT ( 'NONE',  ( -27.84909171997326638, -292.1693790550638141, -193.8948112050751149 ) ) ;
#86271 = CARTESIAN_POINT ( 'NONE',  ( -8.562431834741454750, -278.6765642247831920, -339.8141182845718049 ) ) ;
#86272 = CARTESIAN_POINT ( 'NONE',  ( -88.68438310270911984, -271.3319616250649347, -215.6189326606946111 ) ) ;
#86273 = CARTESIAN_POINT ( 'NONE',  ( -102.3763532919609673, -284.2863313076109080, -229.4385971888172548 ) ) ;
#86274 = CARTESIAN_POINT ( 'NONE',  ( 208.4306832106270804, -125.2391364535880882, 0.000000000000000000 ) ) ;
#86275 = CARTESIAN_POINT ( 'NONE',  ( -69.46683268374196984, -283.6292408607051811, -202.5756833079415458 ) ) ;
#86276 = CARTESIAN_POINT ( 'NONE',  ( -47.80257052418233599, -229.5268262511776527, 22.50000000000000000 ) ) ;
#86277 = CARTESIAN_POINT ( 'NONE',  ( 35.59974763790477681, -292.4600517301558966, -278.9722793919557944 ) ) ;
#86278 = CARTESIAN_POINT ( 'NONE',  ( -74.14780475061962761, -283.6971267830212469, -205.8779670114303997 ) ) ;
#86279 = CARTESIAN_POINT ( 'NONE',  ( 151.4851178187871312, 21.00000000000000000, -3.492110388858667314 ) ) ;
#86280 = CARTESIAN_POINT ( 'NONE',  ( 41.08708295871279859, -293.9068999365417199, -465.6442049081569508 ) ) ;
#86281 = CARTESIAN_POINT ( 'NONE',  ( 18.55458807317983627, -292.2484930871154347, -320.3865286226737226 ) ) ;
#86282 = CARTESIAN_POINT ( 'NONE',  ( -58.31493850242988941, -281.7981763255211831, -343.7838999290952984 ) ) ;
#86283 = CARTESIAN_POINT ( 'NONE',  ( -24.75981994843965239, -281.8154854858634053, -197.6415421828658339 ) ) ;
#86284 = CARTESIAN_POINT ( 'NONE',  ( -36.58484883322544334, -287.2665229466274468, -193.7489566462684536 ) ) ;
#86285 = CARTESIAN_POINT ( 'NONE',  ( -5.349951678169219349, -278.7072058786992557, -201.4372320783726593 ) ) ;
#86286 = CARTESIAN_POINT ( 'NONE',  ( 30.48518437149699878, -287.9149222174347074, -297.4884461264064157 ) ) ;
#86287 = CARTESIAN_POINT ( 'NONE',  ( -29.63380325394025760, -278.3780643453470702, -343.5968823064588946 ) ) ;
#86288 = CARTESIAN_POINT ( 'NONE',  ( -109.7831764641131684, -279.4943893598568820, -259.7703939831317825 ) ) ;
#86289 = CARTESIAN_POINT ( 'NONE',  ( -24.10025114423919845, -288.2002050056193525, -196.1253768880712300 ) ) ;
#86290 = VERTEX_POINT ( 'NONE', #39248 ) ;
#86291 = CARTESIAN_POINT ( 'NONE',  ( -3.408379831611338062, -298.2993333195257151, -193.3620392314379899 ) ) ;
#86293 = CARTESIAN_POINT ( 'NONE',  ( 17.23031493683589233, -290.2490159857565004, -321.3655699858621801 ) ) ;
#86292 = VECTOR ( 'NONE', #86880, 1000.000000000000000 ) ;
#86294 = DIRECTION ( 'NONE',  ( -1.000000000000000000, 0.000000000000000000, 0.000000000000000000 ) ) ;
#86295 = CARTESIAN_POINT ( 'NONE',  ( -111.2869819898779866, -281.4805209788416960, -234.7871824221999191 ) ) ;
#86296 = ORIENTED_EDGE ( 'NONE', *, *, #53514, .T. ) ;
#86297 = CARTESIAN_POINT ( 'NONE',  ( 6.194383980543309853, -272.6409561392168257, -209.0221268541379800 ) ) ;
#86298 = CARTESIAN_POINT ( 'NONE',  ( 21.65418117016169575, -292.6064331404992913, -318.6094537536760072 ) ) ;
#86299 = CIRCLE ( 'NONE', #3168, 1.500000000000001332 ) ;
#86300 = CARTESIAN_POINT ( 'NONE',  ( -38.65651086554108673, -287.5555284709033117, -196.6669122604396023 ) ) ;
#86301 = CARTESIAN_POINT ( 'NONE',  ( 34.43284272088385478, -283.0765261195882090, -252.2434507622298270 ) ) ;
#86302 = CARTESIAN_POINT ( 'NONE',  ( -97.68304183769218696, -291.3465170397900010, -317.2389248408354092 ) ) ;
#86303 = CARTESIAN_POINT ( 'NONE',  ( 22.03309444367659253, -289.5189715471655632, -318.6303900393300523 ) ) ;
#86304 = CARTESIAN_POINT ( 'NONE',  ( -110.6702582425654668, -286.3493563864115004, -286.1675975811750163 ) ) ;
#86305 = CARTESIAN_POINT ( 'NONE',  ( -114.2109756558660507, -278.7749219013197717, -265.8762005561951582 ) ) ;
#86306 = VERTEX_POINT ( 'NONE', #53008 ) ;
#86307 = CARTESIAN_POINT ( 'NONE',  ( -55.74369649047332587, -293.3670965702268063, -343.6460463449091094 ) ) ;
#86308 = CARTESIAN_POINT ( 'NONE',  ( 24.59300617215263784, -280.7774705281651109, -224.6107938304154175 ) ) ;
#86309 = CARTESIAN_POINT ( 'NONE',  ( -101.8018897169095425, -274.9098867110279230, -233.4371889488425325 ) ) ;
#86310 = CARTESIAN_POINT ( 'NONE',  ( -69.85430415644619018, -285.9805209788416391, -337.9475929042657754 ) ) ;
#86311 = CARTESIAN_POINT ( 'NONE',  ( 24.51521640473169583, -273.1994078667647727, -226.2061425263158299 ) ) ;
#86312 = CARTESIAN_POINT ( 'NONE',  ( 201.2104617360081704, 0.000000000000000000, 9.000000000000001776 ) ) ;
#86313 = CARTESIAN_POINT ( 'NONE',  ( -41.04804162620252583, -279.5119002925964082, -197.3936493785935511 ) ) ;
#86314 = CARTESIAN_POINT ( 'NONE',  ( 37.82613986986537924, -276.5716943659761000, -255.6029151879837684 ) ) ;
#86315 = CARTESIAN_POINT ( 'NONE',  ( -80.08491918998299752, -298.8860161893255167, -210.4579282516843364 ) ) ;
#86316 = CARTESIAN_POINT ( 'NONE',  ( -69.10008882171740652, -282.5184739706987784, -340.2627195659547965 ) ) ;
#86317 = CARTESIAN_POINT ( 'NONE',  ( -92.44234038387999419, -293.0099567477064966, -220.9266363056455305 ) ) ;
#86318 = CARTESIAN_POINT ( 'NONE',  ( -34.15723516101967761, -275.6916980864387483, -194.2276851185533530 ) ) ;
#86319 = CARTESIAN_POINT ( 'NONE',  ( 52.98980219858057694, -300.3645473847345784, -193.7401250667022907 ) ) ;
#86320 = CARTESIAN_POINT ( 'NONE',  ( 36.65462921126223250, -295.7002883522731622, -281.8600899583505566 ) ) ;
#86321 = CARTESIAN_POINT ( 'NONE',  ( -7.793200285562991603, -280.6638689061517198, -339.1136785590359182 ) ) ;
#86322 = CARTESIAN_POINT ( 'NONE',  ( -110.4094861314438702, -290.5257626330152334, -245.9694937582152079 ) ) ;
#86323 = CARTESIAN_POINT ( 'NONE',  ( 35.44309492666847916, -273.3579617242340305, -253.7442815901229665 ) ) ;
#86324 = CARTESIAN_POINT ( 'NONE',  ( -7.673608376139617882, -288.0345627838862583, -200.1178468688961800 ) ) ;
#86325 = EDGE_CURVE ( 'NONE', #32648, #7995, #9448, .T. ) ;
#86326 = CARTESIAN_POINT ( 'NONE',  ( -86.12451577205871445, -290.2773499221862608, -215.5711167681582197 ) ) ;
#86327 = ORIENTED_EDGE ( 'NONE', *, *, #46324, .F. ) ;
#86328 = CARTESIAN_POINT ( 'NONE',  ( -111.3558588993663250, -288.8868463609599075, -289.4006274286459188 ) ) ;
#86329 = CARTESIAN_POINT ( 'NONE',  ( -90.61108782081988977, -289.4996938909972641, -320.3795307763307960 ) ) ;
#86330 = ORIENTED_EDGE ( 'NONE', *, *, #10314, .F. ) ;
#86331 = CARTESIAN_POINT ( 'NONE',  ( -43.65458900103428874, -287.0539592477167616, -193.8774504945046999 ) ) ;
#86332 = CARTESIAN_POINT ( 'NONE',  ( -32.41489383520142553, -277.3217483603212941, -343.2658450267799140 ) ) ;
#86333 = EDGE_CURVE ( 'NONE', #50317, #5104, #709, .T. ) ;
#86334 = CARTESIAN_POINT ( 'NONE',  ( 37.15643751955254004, -292.7017875338705721, -288.6237164834165014 ) ) ;
#86335 = CARTESIAN_POINT ( 'NONE',  ( -65.20750573733751310, -284.0583009951000690, -342.0468424071573850 ) ) ;
#86336 = CARTESIAN_POINT ( 'NONE',  ( -112.1975920834811120, -284.6601343182347250, -288.3707270804216023 ) ) ;
#86337 = CARTESIAN_POINT ( 'NONE',  ( -46.46330593507787654, -280.2666285908467785, -197.8608199629846069 ) ) ;
#86338 = CARTESIAN_POINT ( 'NONE',  ( 168.1323214751145940, 232.5674794396639982, -192.7479069522925101 ) ) ;
#86339 = CARTESIAN_POINT ( 'NONE',  ( -57.22704699613181845, -168.7833709488410818, -363.6107807818947890 ) ) ;
#86340 = CARTESIAN_POINT ( 'NONE',  ( 195.2719850531713348, 282.9461876494999046, -110.4261502798884464 ) ) ;
#86341 = B_SPLINE_CURVE_WITH_KNOTS ( 'NONE', 3,
 ( #15728, #14354, #13877, #43214, #79669, #57438, #599, #44589, #73493, #37033, #21432, #73022, #65947, #57892, #1058, #37481 ),
 .UNSPECIFIED., .F., .F.,
 ( 4, 2, 2, 2, 2, 2, 2, 4 ),
 ( 0.000000000000000000, 0.001221894770150660538, 0.001832842155225994276, 0.002443789540301328448, 0.003054736925376662620, 0.003665684310451996358, 0.004276631695527330530, 0.004887579080602664702 ),
 .UNSPECIFIED. ) ;
#86342 = CARTESIAN_POINT ( 'NONE',  ( -68.34171366185952934, -272.8314078624193826, -204.0782356775627875 ) ) ;
#86343 = CARTESIAN_POINT ( 'NONE',  ( -8.838001346521661361, -273.3542176192941042, -202.7661315929888985 ) ) ;
#86344 = CARTESIAN_POINT ( 'NONE',  ( -41.94814925529558280, -294.6162560650674322, -347.2139090605071488 ) ) ;
#86345 = CARTESIAN_POINT ( 'NONE',  ( -106.9338212944154947, -265.3205186674255742, -305.6309630459658706 ) ) ;
#86346 = CARTESIAN_POINT ( 'NONE',  ( -0.2696406066346856423, -273.2193269098884230, -203.4211815681448172 ) ) ;
#86347 = CARTESIAN_POINT ( 'NONE',  ( -55.62034105952465524, -299.6749630383118301, -198.3582352620938707 ) ) ;
#86348 = CARTESIAN_POINT ( 'NONE',  ( 28.67805875981774122, -289.3017653401319080, -302.6509757237433291 ) ) ;
#86349 = CARTESIAN_POINT ( 'NONE',  ( -110.2818165302840043, -291.7283280005871120, -263.0149970709849754 ) ) ;
#86350 = ORIENTED_EDGE ( 'NONE', *, *, #54587, .F. ) ;
#86351 = CARTESIAN_POINT ( 'NONE',  ( -114.0750813442570006, -297.5385987677553317, -266.7583135697273065 ) ) ;
#86352 = CARTESIAN_POINT ( 'NONE',  ( -54.77709676717442022, -286.3144186711474504, -199.3581203944634126 ) ) ;
#86353 = PRODUCT_RELATED_PRODUCT_CATEGORY ( 'part', '', ( #26218 ) ) ;
#86354 = CARTESIAN_POINT ( 'NONE',  ( 13.29710821630033912, -295.1680795559121862, -328.2232806372514915 ) ) ;
#86355 = CARTESIAN_POINT ( 'NONE',  ( 4.199353182774348880, -295.0009991585198463, -335.1839255148053098 ) ) ;
#86356 = CARTESIAN_POINT ( 'NONE',  ( 2.238717458760330459, -292.7649171054112571, -208.9629101380651264 ) ) ;
#86357 = ORIENTED_EDGE ( 'NONE', *, *, #19791, .T. ) ;
#86358 = CARTESIAN_POINT ( 'NONE',  ( -96.69736344339952439, -275.1095435563289584, -223.6040924685493678 ) ) ;
#86359 = VERTEX_POINT ( 'NONE', #74324 ) ;
#86360 = CARTESIAN_POINT ( 'NONE',  ( -112.0246671844481341, -278.2919511252330835, -251.8143463855297455 ) ) ;
#86361 = CARTESIAN_POINT ( 'NONE',  ( -8.641102257194029690, -272.8338447037182277, -202.3160487866714448 ) ) ;
#86362 = CARTESIAN_POINT ( 'NONE',  ( -36.49293769754876138, -299.2680872644565397, -196.9638634735345022 ) ) ;
#86363 = CARTESIAN_POINT ( 'NONE',  ( 19.17280495417879038, -275.8353943621228268, -223.7830205100620162 ) ) ;
#86364 = CARTESIAN_POINT ( 'NONE',  ( -63.23315966276098266, -275.4795684095734032, -198.9215887556935058 ) ) ;
#86365 = AXIS2_PLACEMENT_3D ( 'NONE', #37511, #1539, #49869 ) ;
#86366 = CARTESIAN_POINT ( 'NONE',  ( 34.17707270369782435, -273.2650368110044496, -246.4589025258769936 ) ) ;
#86367 = CARTESIAN_POINT ( 'NONE',  ( -67.32944891327855430, -296.1075192840649493, -337.0428826209879958 ) ) ;
#86368 = CARTESIAN_POINT ( 'NONE',  ( 36.12415627872974966, -292.0605603591563977, -265.2937047847997292 ) ) ;
#86369 = FACE_OUTER_BOUND ( 'NONE', #60535, .T. ) ;
#86370 = CARTESIAN_POINT ( 'NONE',  ( -103.3620152138814632, -279.5612256700283069, -230.7499842046176184 ) ) ;
#86371 = CARTESIAN_POINT ( 'NONE',  ( -41.85446398826587711, -277.2772441112639399, -343.2340943474476376 ) ) ;
#86372 = CARTESIAN_POINT ( 'NONE',  ( 39.08598663172784171, -286.1803768745480738, -265.8641857817764844 ) ) ;
#86373 = CARTESIAN_POINT ( 'NONE',  ( -96.79982564474194362, -299.1813920034890657, -224.3538183514303626 ) ) ;
#86374 = CARTESIAN_POINT ( 'NONE',  ( 82.67245219369620202, -297.7045441827060586, -197.0521791778547254 ) ) ;
#86375 = CARTESIAN_POINT ( 'NONE',  ( 12.25778047535527371, -287.5379722566917167, -324.2118537354415366 ) ) ;
#86376 = CARTESIAN_POINT ( 'NONE',  ( -110.6219054866518263, -276.9318290593772076, -259.6146442693682275 ) ) ;
#86377 = CARTESIAN_POINT ( 'NONE',  ( -110.9398785623254895, -277.1594664548957780, -267.8703577606798376 ) ) ;
#86378 = CARTESIAN_POINT ( 'NONE',  ( -47.52947603537365495, -285.1816843602759945, -344.7177447560963515 ) ) ;
#86379 = CARTESIAN_POINT ( 'NONE',  ( 1.092359196607876948, -277.7321291609044351, -332.9504661303678859 ) ) ;
#86380 = CYLINDRICAL_SURFACE ( 'NONE', #51810, 24.00000000000001066 ) ;
#86381 = CARTESIAN_POINT ( 'NONE',  ( 36.51491496731624409, -273.7149207095698102, -251.6090294515939547 ) ) ;
#86382 = CARTESIAN_POINT ( 'NONE',  ( 35.47896907995129823, -276.1119054076957013, -263.4028032306936211 ) ) ;
#86383 = CARTESIAN_POINT ( 'NONE',  ( 35.88554643735736960, -283.3343134552551987, -253.3400180548439096 ) ) ;
#86384 = DIRECTION ( 'NONE',  ( 0.5370370370370448621, 0.000000000000000000, -0.8435586647355782786 ) ) ;
#86385 = CARTESIAN_POINT ( 'NONE',  ( 36.87117127708231124, -289.2912718827186040, -256.1567553334548393 ) ) ;
#86386 = CARTESIAN_POINT ( 'NONE',  ( 37.60425367300548771, -291.6030440151465655, -274.3375138302612868 ) ) ;
#86387 = LINE ( 'NONE', #50889, #52698 ) ;
#86388 = CARTESIAN_POINT ( 'NONE',  ( -2.666285104127320338, -273.2056785842119098, -205.5625140479185973 ) ) ;
#86389 = CARTESIAN_POINT ( 'NONE',  ( 36.43171639948916862, -291.8048171604463050, -279.0787236017769146 ) ) ;
#86390 = CARTESIAN_POINT ( 'NONE',  ( -104.9628119525177112, -256.0684274861638983, -326.9234398911233939 ) ) ;
#86391 = CARTESIAN_POINT ( 'NONE',  ( 214.2238915819278589, 32.98517505407394168, 10.50000000000000000 ) ) ;
#86392 = CARTESIAN_POINT ( 'NONE',  ( -111.5925778843774054, -288.8093070963093965, -288.0101205340813522 ) ) ;
#86393 = CARTESIAN_POINT ( 'NONE',  ( -112.8986753436223154, -282.6897458480524961, -278.4306600278530937 ) ) ;
#86394 = CARTESIAN_POINT ( 'NONE',  ( -29.36287170192303009, -284.3745221686216951, -343.5674341898863418 ) ) ;
#86395 = CARTESIAN_POINT ( 'NONE',  ( -110.1561881557234415, -285.4552580112109581, -262.7433774483430966 ) ) ;
#86396 = CARTESIAN_POINT ( 'NONE',  ( -85.48205720473674774, -293.3706654641899263, -212.3199657634946504 ) ) ;
#86397 = CARTESIAN_POINT ( 'NONE',  ( -58.11999014631759053, -274.1242175615750511, -196.1841386552216022 ) ) ;
#86398 = CARTESIAN_POINT ( 'NONE',  ( -92.55755105358264245, -287.9145728610459400, -322.0168201580793834 ) ) ;
#86399 = CARTESIAN_POINT ( 'NONE',  ( -100.4655052535041477, -277.9692520710557915, -314.4563016933424819 ) ) ;
#86400 = CARTESIAN_POINT ( 'NONE',  ( 34.89369184675017266, -295.2891519789712902, -251.5490220913792996 ) ) ;
#86401 = DIRECTION ( 'NONE',  ( 0.000000000000000000, 1.000000000000000000, 0.000000000000000000 ) ) ;
#86402 = CARTESIAN_POINT ( 'NONE',  ( -4.829096099716510437, -294.9805209788416391, -202.7746430608542312 ) ) ;
#86403 = CARTESIAN_POINT ( 'NONE',  ( -98.50828509517155851, -283.7987756670174804, -229.6193413699363362 ) ) ;
#86404 = CARTESIAN_POINT ( 'NONE',  ( -67.83541210034404401, -277.6518030914849078, -201.8260592758372525 ) ) ;
#86405 = CARTESIAN_POINT ( 'NONE',  ( -9.454125105613082169, -296.7956549059167628, -194.1685552188437782 ) ) ;
#86406 = CARTESIAN_POINT ( 'NONE',  ( 15.66608948680234548, -275.6253953390411766, -320.7006343524209910 ) ) ;
#86407 = CARTESIAN_POINT ( 'NONE',  ( -37.57136222185162211, -293.5693853405915092, -196.6555783920228464 ) ) ;
#86408 = CARTESIAN_POINT ( 'NONE',  ( 26.43357943670293153, -294.0009509561417644, -234.2559053233001691 ) ) ;
#86409 = CARTESIAN_POINT ( 'NONE',  ( -94.27333152191833676, -297.1691917547461799, -321.4892180444213068 ) ) ;
#86410 = CARTESIAN_POINT ( 'NONE',  ( -108.7786907208520546, -296.5844559066172224, -255.2758315196167018 ) ) ;
#86411 = CARTESIAN_POINT ( 'NONE',  ( -81.56685075715807898, -291.6536940031137419, -330.9991267899555396 ) ) ;
#86412 = CARTESIAN_POINT ( 'NONE',  ( -112.5246317212487099, -284.5108614525953499, -286.9902130148536799 ) ) ;
#86413 = CARTESIAN_POINT ( 'NONE',  ( -60.47113307886002787, -271.8950508871518537, -198.1583805074809277 ) ) ;
#86414 = CARTESIAN_POINT ( 'NONE',  ( 5.181444829031425670, -286.4430669223614814, -206.1042915139386196 ) ) ;
#86415 = CARTESIAN_POINT ( 'NONE',  ( -106.7890561417611650, -280.1741229152506207, -297.7273662306832307 ) ) ;
#86416 = CARTESIAN_POINT ( 'NONE',  ( -35.91690906059066890, -285.1292035160333853, -197.1396838308364750 ) ) ;
#86417 = CARTESIAN_POINT ( 'NONE',  ( -90.20733976565934142, -287.7990660283465445, -323.6340576456236136 ) ) ;
#86419 = AXIS2_PLACEMENT_3D ( 'NONE', #59485, #39885, #31067 ) ;
#86418 = CARTESIAN_POINT ( 'NONE',  ( 197.9738562182569694, 296.4636489450776367, -54.00000000000000711 ) ) ;
#86420 = CARTESIAN_POINT ( 'NONE',  ( -101.0419038713099695, -284.5502215899518887, -234.4765566944677460 ) ) ;
#86421 = VECTOR ( 'NONE', #61435, 1000.000000000000000 ) ;
#86422 = CARTESIAN_POINT ( 'NONE',  ( 38.78635991060995281, -282.6443367673805369, -261.3811964523839606 ) ) ;
#86423 = CARTESIAN_POINT ( 'NONE',  ( -48.84560911062249033, -288.2538667065797426, -346.3127265943128350 ) ) ;
#86424 = CARTESIAN_POINT ( 'NONE',  ( -113.2799984448088395, -280.0648538424637763, -277.2789386874847537 ) ) ;
#86425 = CARTESIAN_POINT ( 'NONE',  ( -81.96488948143928610, -280.7730444168118424, -208.2155691195069949 ) ) ;
#86426 = CARTESIAN_POINT ( 'NONE',  ( -103.3689424359514248, -278.8075887693566415, -239.1070702138660522 ) ) ;
#86427 = CARTESIAN_POINT ( 'NONE',  ( 24.81445327686541447, -292.9487465539360187, -224.9121070593207037 ) ) ;
#86428 = CARTESIAN_POINT ( 'NONE',  ( -73.17000336490163193, -287.5497638199732364, -335.8453106671726687 ) ) ;
#86429 = CARTESIAN_POINT ( 'NONE',  ( -39.21268854037838736, -293.6291943665424924, -194.1711890109491776 ) ) ;
#86430 = CARTESIAN_POINT ( 'NONE',  ( -110.4085359659928400, -295.3864006520545900, -276.9136489945161657 ) ) ;
#86431 = CARTESIAN_POINT ( 'NONE',  ( -26.50953543951491298, -284.8335650735134550, -344.0610956785242251 ) ) ;
#86432 = CARTESIAN_POINT ( 'NONE',  ( -110.3953215218635791, -296.2404035640226425, -268.7281897585174306 ) ) ;
#86433 = CARTESIAN_POINT ( 'NONE',  ( 38.05589761626159628, -294.8088172825385982, -284.4569336261859576 ) ) ;
#86434 = CARTESIAN_POINT ( 'NONE',  ( 22.19169328058926283, -281.6117696140012185, -227.9386270418994513 ) ) ;
#86435 = CARTESIAN_POINT ( 'NONE',  ( -13.12531760410572979, -273.4180151941861823, -197.5161659955479934 ) ) ;
#86436 = CARTESIAN_POINT ( 'NONE',  ( -95.37591663605273595, -290.5207022480558976, -320.8125054870433814 ) ) ;
#86437 = CARTESIAN_POINT ( 'NONE',  ( -4.717521196529470551, -280.7666336285604984, -338.7564252752937932 ) ) ;
#86438 = CARTESIAN_POINT ( 'NONE',  ( -99.85061598318259257, -290.2895289752230497, -315.3100813557242077 ) ) ;
#86439 = CARTESIAN_POINT ( 'NONE',  ( 15.98700896951612371, -287.1678475215834396, -220.4614456096433059 ) ) ;
#86440 = PLANE ( 'NONE',  #71678 ) ;
#86441 = CARTESIAN_POINT ( 'NONE',  ( -14.32388138225487850, -91.12230094864965224, -358.1431036431999360 ) ) ;
#86442 = CARTESIAN_POINT ( 'NONE',  ( 184.1086675408331246, 260.7702122114448002, -150.9958300510270135 ) ) ;
#86443 = CARTESIAN_POINT ( 'NONE',  ( -110.5535585741978508, -277.7457955153106468, -270.6284629835059263 ) ) ;
#86444 = ORIENTED_EDGE ( 'NONE', *, *, #27400, .F. ) ;
#86445 = CARTESIAN_POINT ( 'NONE',  ( -99.72356926569732138, -278.0023733986776620, -231.7580913035668573 ) ) ;
#86446 = CARTESIAN_POINT ( 'NONE',  ( -41.18746612208742874, -273.6718466802412308, -193.4261411279136382 ) ) ;
#86447 = CARTESIAN_POINT ( 'NONE',  ( 140.3020133904481384, 178.1001207059538274, -239.2162932893931213 ) ) ;
#86448 = CARTESIAN_POINT ( 'NONE',  ( -96.35072180182093859, -277.7842267615357628, -221.7965532727406242 ) ) ;
#86449 = CARTESIAN_POINT ( 'NONE',  ( -36.19294861392245366, -281.0577873578358776, -344.9970823454893321 ) ) ;
#86450 = CARTESIAN_POINT ( 'NONE',  ( -99.92891985083171846, -298.8889914382539246, -227.2474786046880695 ) ) ;
#86451 = CARTESIAN_POINT ( 'NONE',  ( -96.81510487270033138, -291.6379222333050052, -227.8384916981444803 ) ) ;
#86452 = CARTESIAN_POINT ( 'NONE',  ( -87.07534179161483223, -288.4467032014727010, -324.5393974894498115 ) ) ;
#86453 = CARTESIAN_POINT ( 'NONE',  ( 18.01045344371307166, -275.4709783284677656, -216.9044312136182384 ) ) ;
#86454 = CARTESIAN_POINT ( 'NONE',  ( -85.31016335348181201, -273.3677128144092876, -215.2662378431653565 ) ) ;
#86455 = ORIENTED_EDGE ( 'NONE', *, *, #67723, .T. ) ;
#86456 = CARTESIAN_POINT ( 'NONE',  ( 222.8344101925596306, -0.9999999999999997780, -22.50000000000000000 ) ) ;
#86457 = DIRECTION ( 'NONE',  ( -0.000000000000000000, -0.000000000000000000, 1.000000000000000000 ) ) ;
#86458 = CARTESIAN_POINT ( 'NONE',  ( -74.32487172137903997, -281.4845176766745567, -204.4706086669636704 ) ) ;
#86459 = CARTESIAN_POINT ( 'NONE',  ( 156.3051094419640492, 18.69637893470003220, 10.18000837680918913 ) ) ;
#86460 = CARTESIAN_POINT ( 'NONE',  ( -14.22438418033115859, -281.4386618551232004, -200.7386715428041271 ) ) ;
#86461 = CARTESIAN_POINT ( 'NONE',  ( -74.53180612248333148, -281.3245306771157175, -204.0974776467722620 ) ) ;
#86462 = CARTESIAN_POINT ( 'NONE',  ( -67.89341848551360670, -282.5220954481408739, -336.9193703201563608 ) ) ;
#86463 = CARTESIAN_POINT ( 'NONE',  ( -106.4084820258049859, -280.0546659060465799, -297.5759138953037564 ) ) ;
#86464 = CARTESIAN_POINT ( 'NONE',  ( -83.61101852201565521, -271.8837667750156015, -213.0038348717735914 ) ) ;
#86465 = LINE ( 'NONE', #79851, #15544 ) ;
#86466 = DIRECTION ( 'NONE',  ( 0.000000000000000000, -1.000000000000000000, 0.000000000000000000 ) ) ;
#86467 = CARTESIAN_POINT ( 'NONE',  ( -74.01077179349272228, -278.3293864949231988, -337.9004387555592643 ) ) ;
#86468 = DIRECTION ( 'NONE',  ( -0.000000000000000000, -0.000000000000000000, 1.000000000000000000 ) ) ;
#86469 = CARTESIAN_POINT ( 'NONE',  ( -68.78958545139009573, -276.0322304367668949, -340.0147479401626356 ) ) ;
#86470 = ORIENTED_EDGE ( 'NONE', *, *, #21629, .F. ) ;
#86471 = CARTESIAN_POINT ( 'NONE',  ( 156.8041522122653930, 275.0000000000000568, 16.89672165344857646 ) ) ;
#86472 = CARTESIAN_POINT ( 'NONE',  ( -109.5250025719447962, -286.2541195697757530, -292.0386652255925242 ) ) ;
#86473 = CARTESIAN_POINT ( 'NONE',  ( 35.86951619082733345, -292.7547096577450816, -270.7710083561801753 ) ) ;
#86474 = CARTESIAN_POINT ( 'NONE',  ( 30.26910897973711201, -287.3765443098334913, -307.1070236309670918 ) ) ;
#86475 = CARTESIAN_POINT ( 'NONE',  ( -77.58145343362549795, -283.7442268206820017, -208.1815928474821078 ) ) ;
#86477 = CARTESIAN_POINT ( 'NONE',  ( 21.14459914411247965, -286.4223256483457476, -315.7393940265175161 ) ) ;
#86476 = CARTESIAN_POINT ( 'NONE',  ( -52.19023546006646086, -284.4330281352165457, -198.2854916311188163 ) ) ;
#86478 = CARTESIAN_POINT ( 'NONE',  ( 36.10033822424737338, -282.7696009153808063, -271.3036252528334558 ) ) ;
#86479 = CARTESIAN_POINT ( 'NONE',  ( -4.673614811919557965, -272.4822888465581059, -202.8355263023359214 ) ) ;
#86480 = AXIS2_PLACEMENT_3D ( 'NONE', #44682, #17215, #53179 ) ;
#86481 = CARTESIAN_POINT ( 'NONE',  ( -70.69746270699212687, -284.0194350772653706, -201.8495604063347741 ) ) ;
#86482 = CARTESIAN_POINT ( 'NONE',  ( -76.02818019034485530, -297.5686729813228339, -334.6738171867392566 ) ) ;
#86483 = CARTESIAN_POINT ( 'NONE',  ( -15.91117444578450701, -284.3283997306367610, -198.2601021308670113 ) ) ;
#86484 = AXIS2_PLACEMENT_3D ( 'NONE', #1972, #81492, #30864 ) ;
#86485 = CARTESIAN_POINT ( 'NONE',  ( -108.3974648963425409, -279.2595210641939047, -288.1465545297805306 ) ) ;
#86486 = CARTESIAN_POINT ( 'NONE',  ( 27.11304886739153375, -289.0344757503367532, -231.5876226921864145 ) ) ;
#86487 = CARTESIAN_POINT ( 'NONE',  ( 196.7737507933381949, 25.83989517275634995, 12.61380704606697023 ) ) ;
#86488 = EDGE_CURVE ( 'NONE', #19459, #38465, #34023, .T. ) ;
#86489 = EDGE_CURVE ( 'NONE', #17165, #90976, #32462, .T. ) ;
#86490 = DIRECTION ( 'NONE',  ( 0.000000000000000000, 1.000000000000000000, 0.000000000000000000 ) ) ;
#86491 = CARTESIAN_POINT ( 'NONE',  ( 29.63739180786915384, -295.9320848867512268, -305.3341853160931691 ) ) ;
#86492 = AXIS2_PLACEMENT_3D ( 'NONE', #20401, #90907, #4771 ) ;
#86493 = CARTESIAN_POINT ( 'NONE',  ( -112.1655873391877662, -276.4768869508372404, -276.2101703488430076 ) ) ;
#86494 = CARTESIAN_POINT ( 'NONE',  ( -77.07698722531993951, -290.7315014170773679, -204.5330060143311641 ) ) ;
#86495 = CARTESIAN_POINT ( 'NONE',  ( -45.19591361731023227, -293.5530039475170270, -343.7930159482908152 ) ) ;
#86496 = CARTESIAN_POINT ( 'NONE',  ( -96.79485038647871420, -277.8375835803828977, -227.1573403322192632 ) ) ;
#86497 = CARTESIAN_POINT ( 'NONE',  ( -84.07602035528144313, -271.4837990614615251, -212.4196172445070658 ) ) ;
#86498 = CARTESIAN_POINT ( 'NONE',  ( -107.8732668597164519, -292.1392591447767586, -249.6635139811467354 ) ) ;
#86499 = CARTESIAN_POINT ( 'NONE',  ( -106.6662871844225293, -281.4805209788416960, -237.0123917617630696 ) ) ;
#86500 = CARTESIAN_POINT ( 'NONE',  ( -30.67101903103514360, -293.4491396299216603, -346.3756545275087433 ) ) ;
#86501 = CARTESIAN_POINT ( 'NONE',  ( -2.975879951691980718, -290.1906082062209293, -335.7279916890816480 ) ) ;
#86502 = CARTESIAN_POINT ( 'NONE',  ( 36.44342055898492561, -291.5618305230439091, -252.2026493786897561 ) ) ;
#86503 = CARTESIAN_POINT ( 'NONE',  ( 24.01069576863294230, -289.5370241730160501, -311.0198220108498504 ) ) ;
#86504 = CARTESIAN_POINT ( 'NONE',  ( 152.4536156746142410, 250.0000000000000568, 14.50000000000000000 ) ) ;
#86505 = CARTESIAN_POINT ( 'NONE',  ( -42.66548026638007940, -289.9237254767711534, -343.3793545533471843 ) ) ;
#86506 = DIRECTION ( 'NONE',  ( 0.000000000000000000, 0.000000000000000000, 1.000000000000000000 ) ) ;
#86507 = CARTESIAN_POINT ( 'NONE',  ( -38.89665040372960902, -290.2763240455488472, -346.9482634420761542 ) ) ;
#86509 = CARTESIAN_POINT ( 'NONE',  ( -107.7518858057029973, -290.8067722654363934, -251.0892277576016625 ) ) ;
#86508 = CARTESIAN_POINT ( 'NONE',  ( 35.59334855745336768, -279.8145483121985535, -289.3053909708036713 ) ) ;
#86510 = CARTESIAN_POINT ( 'NONE',  ( -68.66780773178679453, -279.9848674493933345, -200.0301710753123245 ) ) ;
#86511 = CARTESIAN_POINT ( 'NONE',  ( 33.54479863300238662, -281.6025070688658616, -300.5113676481673224 ) ) ;
#86512 = CARTESIAN_POINT ( 'NONE',  ( 19.32022575039783874, -286.2343163765089002, -319.5756592770393922 ) ) ;
#86513 = FACE_OUTER_BOUND ( 'NONE', #10426, .T. ) ;
#86514 = CARTESIAN_POINT ( 'NONE',  ( 35.91878273937629018, -279.8472731178611070, -282.3514111939365989 ) ) ;
#86515 = CARTESIAN_POINT ( 'NONE',  ( -90.46785551010871984, -283.2996294836206630, -217.4214139592873209 ) ) ;
#86516 = CARTESIAN_POINT ( 'NONE',  ( -106.7800878583809805, -277.4415715107390383, -238.5951022652082258 ) ) ;
#86517 = CARTESIAN_POINT ( 'NONE',  ( -83.29993878155930531, -274.2063475022424086, -213.4362374268059455 ) ) ;
#86518 = CARTESIAN_POINT ( 'NONE',  ( 155.2961426000110805, 19.82592759221843792, -13.64628225442899456 ) ) ;
#86519 = CARTESIAN_POINT ( 'NONE',  ( -111.1367662434341810, -292.1411499515317587, -271.2147162723267684 ) ) ;
#86520 = CARTESIAN_POINT ( 'NONE',  ( 36.01501685001681352, -276.7050348262910688, -248.7894985191474859 ) ) ;
#86521 = CARTESIAN_POINT ( 'NONE',  ( 26.78329200377127606, -275.6968005483327602, -305.3963521520410040 ) ) ;
#86522 = CARTESIAN_POINT ( 'NONE',  ( -69.34833097464030516, -297.4733591768510905, -338.2027714645250853 ) ) ;
#86523 = CARTESIAN_POINT ( 'NONE',  ( -74.42545568204182871, -289.6979756053364099, -337.8579842583397976 ) ) ;
#86524 = CARTESIAN_POINT ( 'NONE',  ( 35.09112599277639077, -279.9091247010081815, -292.0536971579592205 ) ) ;
#86525 = CARTESIAN_POINT ( 'NONE',  ( 28.05348044369287663, -292.8525756553774499, -229.6097766613948750 ) ) ;
#86526 = CARTESIAN_POINT ( 'NONE',  ( -96.94589859175326296, -290.2045545953758392, -227.7224738577461096 ) ) ;
#86527 = CARTESIAN_POINT ( 'NONE',  ( -58.31705146053971589, -293.3229525034639664, -342.4224412595595481 ) ) ;
#86528 = VERTEX_POINT ( 'NONE', #17513 ) ;
#86529 = CARTESIAN_POINT ( 'NONE',  ( 197.2116943569230330, 250.5000000000000568, -12.92446933126074882 ) ) ;
#86530 = CARTESIAN_POINT ( 'NONE',  ( -49.69296328023995812, -291.3981534834759941, -198.2997868370860033 ) ) ;
#86531 = FACE_OUTER_BOUND ( 'NONE', #52447, .T. ) ;
#86532 = CARTESIAN_POINT ( 'NONE',  ( -21.39648532958014826, -280.3380690714490129, -340.3683826091709079 ) ) ;
#86533 = CARTESIAN_POINT ( 'NONE',  ( -68.14280511368195903, -294.5056135763352358, -340.6754987677576310 ) ) ;
#86534 = CARTESIAN_POINT ( 'NONE',  ( -68.96721297771652814, -284.7745350173466932, -340.0398135309175132 ) ) ;
#86535 = CARTESIAN_POINT ( 'NONE',  ( -98.10589027291987918, -284.9470843605537880, -229.9048057365434659 ) ) ;
#86536 = CARTESIAN_POINT ( 'NONE',  ( 27.38490336241590839, -277.5499053878468203, -305.6981520168409929 ) ) ;
#86537 = CARTESIAN_POINT ( 'NONE',  ( 37.06195170961772334, -291.6496001805000446, -276.3563989471903710 ) ) ;
#86538 = CARTESIAN_POINT ( 'NONE',  ( 35.90744663217885346, -295.1742726410018349, -259.7527951850630643 ) ) ;
#86539 = CARTESIAN_POINT ( 'NONE',  ( -6.121590218001384365, -275.4274155596753531, -336.8011235376149557 ) ) ;
#86540 = ORIENTED_EDGE ( 'NONE', *, *, #71165, .F. ) ;
#86541 = CARTESIAN_POINT ( 'NONE',  ( 195.0325088190295162, 41.78303943026349998, 13.56014590831882671 ) ) ;
#86542 = CARTESIAN_POINT ( 'NONE',  ( 22.26756620735826075, -293.8730753312837578, -319.0899163082253835 ) ) ;
#86543 = CARTESIAN_POINT ( 'NONE',  ( 36.88987362935750269, -289.5527328293007372, -276.5777220055502426 ) ) ;
#86544 = DIRECTION ( 'NONE',  ( -1.000000000000000000, 0.000000000000000000, 0.000000000000000000 ) ) ;
#86545 = CARTESIAN_POINT ( 'NONE',  ( -99.25523899230893221, -274.3599914758804061, -225.1652414003027616 ) ) ;
#86546 = CARTESIAN_POINT ( 'NONE',  ( -22.44716109393969816, -286.8992027657391191, -198.7406998100513533 ) ) ;
#86547 = VERTEX_POINT ( 'NONE', #2830 ) ;
#86548 = CARTESIAN_POINT ( 'NONE',  ( -74.88237176057604927, -278.6235736397393907, -203.4020395351702746 ) ) ;
#86549 = CARTESIAN_POINT ( 'NONE',  ( 24.80879777540378228, -294.8056175612099423, -315.6671661990956750 ) ) ;
#86550 = CARTESIAN_POINT ( 'NONE',  ( -15.33405060201770809, -286.9099416125969810, -342.9140302957284803 ) ) ;
#86551 = CARTESIAN_POINT ( 'NONE',  ( -41.94005412120833398, -295.4417511395780025, -347.2548885691115856 ) ) ;
#86553 = CARTESIAN_POINT ( 'NONE',  ( 16.75098663953888334, -293.1820872911092124, -221.2352683679915799 ) ) ;
#86552 = CIRCLE ( 'NONE', #38221, 4.000000000000003553 ) ;
#86554 = DIRECTION ( 'NONE',  ( 0.000000000000000000, 0.000000000000000000, 1.000000000000000000 ) ) ;
#86555 = AXIS2_PLACEMENT_3D ( 'NONE', #67098, #53813, #76054 ) ;
#86556 = LINE ( 'NONE', #74221, #44749 ) ;
#86557 = DIRECTION ( 'NONE',  ( -0.000000000000000000, -0.000000000000000000, 1.000000000000000000 ) ) ;
#86558 = CARTESIAN_POINT ( 'NONE',  ( -10.25831565879497198, -287.9192875929880415, -198.9662194095278664 ) ) ;
#86559 = CARTESIAN_POINT ( 'NONE',  ( -72.02372285203398405, -283.1237833571631768, -198.2697987213421698 ) ) ;
#86560 = ORIENTED_EDGE ( 'NONE', *, *, #79269, .F. ) ;
#86561 = AXIS2_PLACEMENT_3D ( 'NONE', #23037, #67078, #46204 ) ;
#86562 = CARTESIAN_POINT ( 'NONE',  ( -98.49025049259559239, -278.5233984067970709, -223.7117009529606264 ) ) ;
#86563 = CARTESIAN_POINT ( 'NONE',  ( -79.38615718651213626, -285.6214919280812978, -332.2666270668925108 ) ) ;
#86564 = CARTESIAN_POINT ( 'NONE',  ( -65.64212688874044943, -284.2639610381068564, -199.3703719930022942 ) ) ;
#86566 = CARTESIAN_POINT ( 'NONE',  ( 37.09489171929099172, -285.6412118374488500, -271.0738514758131714 ) ) ;
#86565 = CIRCLE ( 'NONE', #73000, 0.5000000000000004441 ) ;
#86567 = CARTESIAN_POINT ( 'NONE',  ( 30.75565881523614564, -277.8473004034264022, -303.6929674794075709 ) ) ;
#86568 = CARTESIAN_POINT ( 'NONE',  ( -31.34220272111978289, -274.4632590561496386, -197.5742006228605874 ) ) ;
#86569 = ORIENTED_EDGE ( 'NONE', *, *, #68922, .F. ) ;
#86570 = CARTESIAN_POINT ( 'NONE',  ( 32.81259321861030998, -292.5252439015642949, -292.2613144033559820 ) ) ;
#86572 = CARTESIAN_POINT ( 'NONE',  ( -66.10217463974014152, -279.0141250549779102, -203.1408555820492836 ) ) ;
#86571 = CARTESIAN_POINT ( 'NONE',  ( -92.72663762731934867, -277.8750943379425280, -317.9164404838900282 ) ) ;
#86573 = CARTESIAN_POINT ( 'NONE',  ( 2.246617366452872577, -275.6490935848023014, -204.6781093158861040 ) ) ;
#86574 = CARTESIAN_POINT ( 'NONE',  ( -112.6779380663107162, -277.1717738909307513, -284.3062580674422861 ) ) ;
#86575 = CARTESIAN_POINT ( 'NONE',  ( 119.8472243494001503, 149.1509795950258876, -261.3511535428332877 ) ) ;
#86576 = CARTESIAN_POINT ( 'NONE',  ( -71.79200863345266725, -296.9237957464192164, -338.5650954234693017 ) ) ;
#86577 = CARTESIAN_POINT ( 'NONE',  ( 157.3402357740650075, 250.0000000000000568, 16.90039380915369094 ) ) ;
#86578 = CARTESIAN_POINT ( 'NONE',  ( 82.62999361571313273, -301.0392330995247789, -193.3423597593975956 ) ) ;
#86579 = CARTESIAN_POINT ( 'NONE',  ( -104.8877006405983678, -286.0141680809398963, -241.7391104908703312 ) ) ;
#86580 = CARTESIAN_POINT ( 'NONE',  ( -7.758601965761246610, -288.1945497742897828, -200.3136864427681019 ) ) ;
#86581 = CARTESIAN_POINT ( 'NONE',  ( 19.58765224678785088, -287.5481978791106599, -316.2189581710816242 ) ) ;
#86582 = CARTESIAN_POINT ( 'NONE',  ( -107.8672083172448311, -284.4536648349308052, -239.4760275200687829 ) ) ;
#86583 = CARTESIAN_POINT ( 'NONE',  ( 13.90512840747237888, -279.1850558169803094, -217.1842997244860385 ) ) ;
#86584 = CARTESIAN_POINT ( 'NONE',  ( -109.9228230600453600, -286.2096344421236154, -286.0049239099858482 ) ) ;
#86585 = CARTESIAN_POINT ( 'NONE',  ( 19.38206654844255894, -279.3709616335137866, -223.2976951285214682 ) ) ;
#86586 = CARTESIAN_POINT ( 'NONE',  ( -43.23001584571776590, -278.4432410717428752, -343.6180030938161849 ) ) ;
#86587 = CARTESIAN_POINT ( 'NONE',  ( 33.56739263977607379, -275.8123980091436351, -252.7574534580762133 ) ) ;
#86588 = CARTESIAN_POINT ( 'NONE',  ( -8.397461088183382216, -287.4764934968380317, -341.2994923637252214 ) ) ;
#86589 = CARTESIAN_POINT ( 'NONE',  ( -55.65377196893206957, -284.0849025594745285, -344.9856906439463273 ) ) ;
#86590 = CIRCLE ( 'NONE', #12537, 6.154241149514405151 ) ;
#86591 = CARTESIAN_POINT ( 'NONE',  ( 32.33932048692548733, -282.4639266343517647, -303.1069315509960234 ) ) ;
#86592 = ORIENTED_EDGE ( 'NONE', *, *, #59069, .F. ) ;
#86593 = ORIENTED_EDGE ( 'NONE', *, *, #52524, .F. ) ;
#86594 = LINE ( 'NONE', #79055, #32229 ) ;
#86595 = CARTESIAN_POINT ( 'NONE',  ( -67.53944006126283739, -291.3045185465318241, -339.8478216424853144 ) ) ;
#86596 = CARTESIAN_POINT ( 'NONE',  ( -113.1750209137404397, -289.3693546684516491, -259.8444448273807552 ) ) ;
#86597 = CARTESIAN_POINT ( 'NONE',  ( -98.03147786611464198, -272.1798973711223653, -229.2809214978196053 ) ) ;
#86598 = EDGE_CURVE ( 'NONE', #23364, #85888, #79392, .T. ) ;
#86599 = CARTESIAN_POINT ( 'NONE',  ( 36.99589893742542301, -293.1474253915205850, -290.0393839646713445 ) ) ;
#86600 = CARTESIAN_POINT ( 'NONE',  ( -111.0608795363489776, -289.0573305001290692, -268.4244046645557091 ) ) ;
#86601 = CARTESIAN_POINT ( 'NONE',  ( 19.26589789839507461, -291.1238969545192958, -222.6793199731177140 ) ) ;
#86602 = CARTESIAN_POINT ( 'NONE',  ( 16.31165787213243235, -289.4743245370594309, -320.5199069232691613 ) ) ;
#86603 = CARTESIAN_POINT ( 'NONE',  ( -69.85430415644619018, -297.9805209788416391, -337.9475929042657754 ) ) ;
#86604 = CARTESIAN_POINT ( 'NONE',  ( 22.56059550323598373, -290.1692442202887605, -315.4911039126819219 ) ) ;
#86605 = CARTESIAN_POINT ( 'NONE',  ( -112.2867767625877207, -288.4698658295511677, -276.7712763467328045 ) ) ;
#86606 = CARTESIAN_POINT ( 'NONE',  ( -71.84811252851179120, -293.5962634241609521, -203.7563775444847352 ) ) ;
#86607 = CARTESIAN_POINT ( 'NONE',  ( -103.2190963056276729, -285.0602782140209683, -302.4709360955877742 ) ) ;
#86608 = CARTESIAN_POINT ( 'NONE',  ( 37.82176059342154417, -295.5154156594693973, -267.4808256001151108 ) ) ;
#86609 = CARTESIAN_POINT ( 'NONE',  ( -114.0438498160389287, -273.6021560138187851, -270.3744733279939965 ) ) ;
#86610 = EDGE_CURVE ( 'NONE', #46837, #71459, #65755, .T. ) ;
#86611 = CARTESIAN_POINT ( 'NONE',  ( 160.5350683151633291, 250.0000000000000568, 20.22542485937379908 ) ) ;
#86612 = CARTESIAN_POINT ( 'NONE',  ( -104.1623545849157608, -274.9924854991103871, -235.4142766501725816 ) ) ;
#86613 = CARTESIAN_POINT ( 'NONE',  ( 34.72791690778539930, -280.5835666836326823, -257.7685794157575856 ) ) ;
#86614 = CARTESIAN_POINT ( 'NONE',  ( -88.30606934901378224, -281.7653921865735924, -325.4561296543740241 ) ) ;
#86615 = CARTESIAN_POINT ( 'NONE',  ( -109.6953663863599360, -296.0765333812132099, -244.4940385337762905 ) ) ;
#86616 = CARTESIAN_POINT ( 'NONE',  ( -36.70514686350039568, -272.3001141793175748, -196.3379308233194251 ) ) ;
#86617 = CARTESIAN_POINT ( 'NONE',  ( -103.1409666945161376, -276.1670178666419702, -305.1716151698924477 ) ) ;
#86618 = CARTESIAN_POINT ( 'NONE',  ( -44.63457604021047587, -299.2732584249731076, -197.1799815692015443 ) ) ;
#86619 = CIRCLE ( 'NONE', #17080, 1.000000000000000888 ) ;
#86620 = CARTESIAN_POINT ( 'NONE',  ( -23.38947313059208710, -296.2956951785070032, -342.6676235240379924 ) ) ;
#86621 = CARTESIAN_POINT ( 'NONE',  ( -70.99599795410820491, -296.3109421953061542, -335.3365823052049564 ) ) ;
#86622 = CARTESIAN_POINT ( 'NONE',  ( 199.4392256788250677, 65.82574266882505754, 7.741079165001062634 ) ) ;
#86623 = VECTOR ( 'NONE', #73129, 1000.000000000000000 ) ;
#86625 = CARTESIAN_POINT ( 'NONE',  ( -109.0456709670273057, -296.7336842046639163, -256.5999975610927208 ) ) ;
#86624 = CARTESIAN_POINT ( 'NONE',  ( 37.95935206350324620, -285.6233772988311443, -274.3613093923165138 ) ) ;
#86626 = VECTOR ( 'NONE', #90075, 1000.000000000000000 ) ;
#86627 = CARTESIAN_POINT ( 'NONE',  ( -100.9964917951645447, -285.1245554816696881, -226.9417931976975638 ) ) ;
#86628 = CARTESIAN_POINT ( 'NONE',  ( 38.27021368908083332, -287.0382009155877086, -255.9187227345602764 ) ) ;
#86629 = CARTESIAN_POINT ( 'NONE',  ( -89.55385694715241129, -297.7630677471756826, -324.7679817973432250 ) ) ;
#86630 = CARTESIAN_POINT ( 'NONE',  ( 31.55332648678318108, -291.1678279917462078, -241.0136516255639663 ) ) ;
#86631 = AXIS2_PLACEMENT_3D ( 'NONE', #15729, #30870, #66844 ) ;
#86632 = CARTESIAN_POINT ( 'NONE',  ( -25.41056192972533623, -279.3977002205458575, -194.4545519860903937 ) ) ;
#86633 = CARTESIAN_POINT ( 'NONE',  ( 21.27581636871891391, -279.6952119285918457, -317.1477375740089997 ) ) ;
#86634 = CIRCLE ( 'NONE', #45803, 15.36528803885689420 ) ;
#86635 = CARTESIAN_POINT ( 'NONE',  ( 208.6208076322478746, 32.98517505407394168, 14.49999999999999822 ) ) ;
#86636 = CARTESIAN_POINT ( 'NONE',  ( -6.837553730355165449, -285.2566054092299055, -203.5893374466559465 ) ) ;
#86638 = CARTESIAN_POINT ( 'NONE',  ( 196.8803347170859865, 73.40565171261611965, -12.50000000000000355 ) ) ;
#86637 = CARTESIAN_POINT ( 'NONE',  ( -87.19397867757579945, -288.6479529970536078, -328.7081736748474441 ) ) ;
#86639 = CARTESIAN_POINT ( 'NONE',  ( 129.8483263487583201, -299.5541904835127980, -195.3611179825600175 ) ) ;
#86640 = CARTESIAN_POINT ( 'NONE',  ( -105.6952829210544991, -297.7835847718082505, -298.1860731998385745 ) ) ;
#86641 = CARTESIAN_POINT ( 'NONE',  ( -72.25390656051285987, -281.0247557833624796, -202.3778776701827269 ) ) ;
#86643 = CARTESIAN_POINT ( 'NONE',  ( 22.13317929003263984, -280.6272342822693986, -227.9957287477335512 ) ) ;
#86642 = CARTESIAN_POINT ( 'NONE',  ( -107.9063864159121806, -294.2288382810562553, -296.9476805277259928 ) ) ;
#86644 = CARTESIAN_POINT ( 'NONE',  ( -0.7043056518484719364, -294.7459482385098113, -338.1011932398528756 ) ) ;
#86645 = AXIS2_PLACEMENT_3D ( 'NONE', #89839, #25907, #9363 ) ;
#86646 = CARTESIAN_POINT ( 'NONE',  ( -110.8287231321905040, -280.3590449753974099, -285.4130816221634177 ) ) ;
#86647 = CARTESIAN_POINT ( 'NONE',  ( -79.85492834090354108, -296.5198728734865199, -210.7286278917784728 ) ) ;
#86648 = ORIENTED_EDGE ( 'NONE', *, *, #89784, .T. ) ;
#86649 = FACE_OUTER_BOUND ( 'NONE', #18238, .T. ) ;
#86650 = CIRCLE ( 'NONE', #57959, 7.500000000000012434 ) ;
#86651 = CARTESIAN_POINT ( 'NONE',  ( -0.4169210472922616484, -284.5385596007845947, -335.2333577570809666 ) ) ;
#86652 = CARTESIAN_POINT ( 'NONE',  ( 165.2494399300530290, 8.542400036368780647, 9.000000000000001776 ) ) ;
#86653 = CARTESIAN_POINT ( 'NONE',  ( -106.6662871844225293, -287.6237833571633473, -303.7098442033569086 ) ) ;
#86654 = CARTESIAN_POINT ( 'NONE',  ( -7.955868606643791807, -275.8740238432718570, -341.3727782244550895 ) ) ;
#86655 = CARTESIAN_POINT ( 'NONE',  ( 16.73960894791003184, -292.6822067836282031, -221.2542117713003620 ) ) ;
#86656 = CARTESIAN_POINT ( 'NONE',  ( 33.39472534701439344, -282.8014630031112233, -249.6955460279457384 ) ) ;
#86657 = CARTESIAN_POINT ( 'NONE',  ( -38.11092209400543851, -275.6424849317033932, -196.5651240865178409 ) ) ;
#86658 = VECTOR ( 'NONE', #16556, 1000.000000000000000 ) ;
#86659 = CARTESIAN_POINT ( 'NONE',  ( 4.127594721337612960, -284.1038895794540053, -334.3510906276478067 ) ) ;
#86660 = CARTESIAN_POINT ( 'NONE',  ( 21.65725855215440987, -279.7380021454428061, -226.6792975752978521 ) ) ;
#86661 = CARTESIAN_POINT ( 'NONE',  ( -107.1194733263091479, -280.1943879412970659, -297.8577180270788745 ) ) ;
#86662 = CARTESIAN_POINT ( 'NONE',  ( -81.25212869392009907, -273.6403449735436766, -207.0440409089503078 ) ) ;
#86663 = CARTESIAN_POINT ( 'NONE',  ( 29.94856527696839876, -274.8990454977193281, -232.8212673127507912 ) ) ;
#86664 = CARTESIAN_POINT ( 'NONE',  ( 19.07955243041028126, -296.1506179762771467, -318.9393553440310143 ) ) ;
#86665 = LINE ( 'NONE', #8067, #21868 ) ;
#86666 = DIRECTION ( 'NONE',  ( 1.124465274301078034E-16, 1.000000000000000000, 0.000000000000000000 ) ) ;
#86667 = CARTESIAN_POINT ( 'NONE',  ( 10.40128966923078302, -292.5411853387999486, -329.2582298398679086 ) ) ;
#86668 = CARTESIAN_POINT ( 'NONE',  ( -71.93133220182700427, -273.0898281975242412, -205.9499056625479341 ) ) ;
#86669 = CARTESIAN_POINT ( 'NONE',  ( 22.55171687390224022, -294.4338839230368876, -223.0593153689044073 ) ) ;
#86671 = CARTESIAN_POINT ( 'NONE',  ( -34.98806743517886275, -293.2861335694759077, -193.7812730045262981 ) ) ;
#86670 = CARTESIAN_POINT ( 'NONE',  ( -99.90806341382572953, -299.6948066931273047, -220.5068182859052968 ) ) ;
#86672 = CARTESIAN_POINT ( 'NONE',  ( 20.95738955222951105, -290.1993422388954400, -317.2785409040520790 ) ) ;
#86673 = CARTESIAN_POINT ( 'NONE',  ( -109.5969203092538322, -276.3010762879391677, -289.8344737676102341 ) ) ;
#86674 = CARTESIAN_POINT ( 'NONE',  ( -56.95651819445507869, -279.2271161602518532, -342.2239288787270652 ) ) ;
#86675 = CARTESIAN_POINT ( 'NONE',  ( 36.13926416016368393, -291.4768814131369368, -258.3706629114885800 ) ) ;
#86676 = CARTESIAN_POINT ( 'NONE',  ( 3.141622936810263500, -282.4497111881916567, -206.2569376537458936 ) ) ;
#86677 = ORIENTED_EDGE ( 'NONE', *, *, #90853, .F. ) ;
#86678 = CARTESIAN_POINT ( 'NONE',  ( 5.601101455435562926, -282.1188570139379976, -329.4204379824330431 ) ) ;
#86679 = CARTESIAN_POINT ( 'NONE',  ( -41.00743043545369915, -281.0867354221526284, -193.7447449540067339 ) ) ;
#86680 = AXIS2_PLACEMENT_3D ( 'NONE', #60436, #30606, #80798 ) ;
#86681 = CARTESIAN_POINT ( 'NONE',  ( -95.97633632999615827, -282.6796996051750739, -319.6763288866721382 ) ) ;
#86682 = CARTESIAN_POINT ( 'NONE',  ( -97.51993451947126346, -280.1330867536838127, -222.7019077526034323 ) ) ;
#86683 = DIRECTION ( 'NONE',  ( 0.000000000000000000, 0.000000000000000000, 1.000000000000000000 ) ) ;
#86684 = CARTESIAN_POINT ( 'NONE',  ( 38.23478642177757791, -276.9393692068623523, -259.8300955601204123 ) ) ;
#86685 = CARTESIAN_POINT ( 'NONE',  ( -92.05005921254146983, -286.4090924074130839, -314.0302885647153062 ) ) ;
#86686 = ORIENTED_EDGE ( 'NONE', *, *, #24497, .T. ) ;
#86687 = ORIENTED_EDGE ( 'NONE', *, *, #66535, .T. ) ;
#86688 = AXIS2_PLACEMENT_3D ( 'NONE', #76850, #11977, #62671 ) ;
#86689 = CARTESIAN_POINT ( 'NONE',  ( -66.36968767766522603, -299.6722401657189039, -201.2063886482227701 ) ) ;
#86690 = AXIS2_PLACEMENT_3D ( 'NONE', #86135, #35024, #56349 ) ;
#86691 = CARTESIAN_POINT ( 'NONE',  ( -59.71140343208254819, -275.3634594636380371, -341.5751838313061626 ) ) ;
#86692 = CARTESIAN_POINT ( 'NONE',  ( -110.6610301073443736, -292.5661275606721574, -250.3554912141422903 ) ) ;
#86693 = CARTESIAN_POINT ( 'NONE',  ( 34.81589721817466199, -292.7454174113557883, -258.5706659591877496 ) ) ;
#86694 = CARTESIAN_POINT ( 'NONE',  ( -112.5065677701033167, -289.8542303650173722, -286.7857816292012103 ) ) ;
#86695 = LINE ( 'NONE', #544, #92865 ) ;
#86697 = CARTESIAN_POINT ( 'NONE',  ( -98.76169625675011332, -283.5138672670969413, -229.4462736011043944 ) ) ;
#86696 = CARTESIAN_POINT ( 'NONE',  ( -53.18493490559410475, -293.8260492327401607, -345.1654854126097121 ) ) ;
#86698 = CARTESIAN_POINT ( 'NONE',  ( -97.78057896873443156, -293.0057700165469328, -227.1695229211751439 ) ) ;
#86699 = CARTESIAN_POINT ( 'NONE',  ( -9.210978061590564536, -284.9065961328348635, -202.2345573385242119 ) ) ;
#86700 = CARTESIAN_POINT ( 'NONE',  ( 1.375247953333307738, -283.8386693197529098, -332.8884730680869666 ) ) ;
#86701 = CARTESIAN_POINT ( 'NONE',  ( -112.8995707007084945, -291.3223842879201015, -283.9936348109647497 ) ) ;
#86702 = CARTESIAN_POINT ( 'NONE',  ( 34.62662783376197240, -281.8785372207613023, -257.7695250671700364 ) ) ;
#86703 = CARTESIAN_POINT ( 'NONE',  ( -0.9086171950829795563, -293.3744140845097377, -337.7601903255441584 ) ) ;
#86704 = CARTESIAN_POINT ( 'NONE',  ( 5.475836976171089887, -289.2911366344806083, -334.1640750962648099 ) ) ;
#86705 = CARTESIAN_POINT ( 'NONE',  ( 23.24288397586526500, -288.6790875584675291, -317.8063261126611110 ) ) ;
#86706 = CARTESIAN_POINT ( 'NONE',  ( -69.98433501684097280, -285.7764693340060376, -205.0520100612092733 ) ) ;
#86707 = ORIENTED_EDGE ( 'NONE', *, *, #91432, .T. ) ;
#86708 = DIRECTION ( 'NONE',  ( 1.000000000000000000, 0.000000000000000000, 0.000000000000000000 ) ) ;
#86709 = CARTESIAN_POINT ( 'NONE',  ( -3.754695127627726059, -296.4742495132108502, -338.2888061178431371 ) ) ;
#86710 = AXIS2_PLACEMENT_3D ( 'NONE', #34589, #54947, #70116 ) ;
#86711 = CARTESIAN_POINT ( 'NONE',  ( -108.9817021583558017, -294.8934493970625681, -297.3622740399097779 ) ) ;
#86712 = CARTESIAN_POINT ( 'NONE',  ( -110.6274337749806733, -277.6073983759084740, -270.6269837945009158 ) ) ;
#86713 = ADVANCED_FACE ( 'NONE', ( #8984 ), #52124, .T. ) ;
#86714 = CARTESIAN_POINT ( 'NONE',  ( -114.1191532768571619, -272.1316067803842316, -264.6245811096715101 ) ) ;
#86715 = CARTESIAN_POINT ( 'NONE',  ( -15.40472209019244154, -293.2429894010492717, -340.7673072040351485 ) ) ;
#86716 = CARTESIAN_POINT ( 'NONE',  ( 3.470279454689859655, -276.3689327198972592, -208.5555960561645463 ) ) ;
#86717 = CARTESIAN_POINT ( 'NONE',  ( -57.16910997214898060, -271.9333435231922067, -198.7691379592928627 ) ) ;
#86718 = CARTESIAN_POINT ( 'NONE',  ( 27.83212250028824997, -294.3006420160401149, -236.6045875376940444 ) ) ;
#86719 = CARTESIAN_POINT ( 'NONE',  ( -88.70867372903639136, -296.8732738897116974, -322.7359824693222663 ) ) ;
#86720 = CARTESIAN_POINT ( 'NONE',  ( -43.38975745197526379, -264.0880790402558773, -436.2305102663831349 ) ) ;
#86721 = AXIS2_PLACEMENT_3D ( 'NONE', #68714, #75800, #25602 ) ;
#86722 = CARTESIAN_POINT ( 'NONE',  ( -112.4759463231367675, -294.5976597225312048, -266.7962079353489457 ) ) ;
#86723 = CARTESIAN_POINT ( 'NONE',  ( -34.06070296774593942, -298.7436293451507368, -193.4626981786925342 ) ) ;
#86724 = CARTESIAN_POINT ( 'NONE',  ( -111.1012288709428191, -274.7303055157603353, -256.4985364200303479 ) ) ;
#86725 = CARTESIAN_POINT ( 'NONE',  ( -98.29989936894735081, -290.9314815426498626, -310.9734290032396302 ) ) ;
#86726 = CARTESIAN_POINT ( 'NONE',  ( 3.831806899958924539, -294.8139180827574251, -330.6672520463549176 ) ) ;
#86727 = CARTESIAN_POINT ( 'NONE',  ( -111.4434848272890264, -280.3562271081813151, -284.1188251430195919 ) ) ;
#86728 = CARTESIAN_POINT ( 'NONE',  ( -64.55117762688779237, -278.3892292071748784, -198.8004110773277091 ) ) ;
#86729 = AXIS2_PLACEMENT_3D ( 'NONE', #2709, #89316, #82236 ) ;
#86730 = CARTESIAN_POINT ( 'NONE',  ( -63.88462517043102906, -282.7379730644068445, -342.5330371526828230 ) ) ;
#86731 = CARTESIAN_POINT ( 'NONE',  ( 14.80795133416751952, -275.6891104146346834, -326.9466496730910876 ) ) ;
#86732 = CARTESIAN_POINT ( 'NONE',  ( -107.7654563252636848, -277.3258044046063446, -241.2589706949641197 ) ) ;
#86733 = CARTESIAN_POINT ( 'NONE',  ( -31.19759255770202699, -278.1293027332055203, -195.3945408290494754 ) ) ;
#86734 = ADVANCED_FACE ( 'NONE', ( #67248, #52544 ), #89441, .T. ) ;
#86735 = CARTESIAN_POINT ( 'NONE',  ( -50.02265937824991937, -296.5717627639884313, -197.9702570311816032 ) ) ;
#86736 = CARTESIAN_POINT ( 'NONE',  ( 37.70677765558541950, -277.5439293079206209, -269.7078477727451400 ) ) ;
#86737 = CARTESIAN_POINT ( 'NONE',  ( 175.2296996224750103, 20.99999999999998934, 0.000000000000000000 ) ) ;
#86738 = CARTESIAN_POINT ( 'NONE',  ( -66.35828801208229777, -289.6942219311950453, -200.8165680025540496 ) ) ;
#86739 = CARTESIAN_POINT ( 'NONE',  ( -112.3172705891065988, -290.7715247174101023, -252.8207692390531065 ) ) ;
#86740 = CARTESIAN_POINT ( 'NONE',  ( -75.52394515027168609, -275.5446726040855197, -205.5541919999960783 ) ) ;
#86741 = CARTESIAN_POINT ( 'NONE',  ( -71.27671329616893559, -295.6029625535011860, -203.6502075215037735 ) ) ;
#86742 = CARTESIAN_POINT ( 'NONE',  ( -40.79895115453716414, -285.2070089660477379, -193.5483263464104482 ) ) ;
#86743 = CARTESIAN_POINT ( 'NONE',  ( 209.4046159701566410, 38.09026110277402211, 12.05941621939746966 ) ) ;
#86744 = CARTESIAN_POINT ( 'NONE',  ( -99.86092609266262343, -281.9913932701669523, -311.8814526483932354 ) ) ;
#86745 = CARTESIAN_POINT ( 'NONE',  ( 197.2116943569230330, 250.5000000000000568, -11.92446933126074882 ) ) ;
#86746 = CARTESIAN_POINT ( 'NONE',  ( 6.927883640651658403, -291.4651308904388998, -211.8176772176007887 ) ) ;
#86747 = CARTESIAN_POINT ( 'NONE',  ( -94.18591574876103323, -283.3585247542855541, -222.6159545265933843 ) ) ;
#86748 = CARTESIAN_POINT ( 'NONE',  ( 199.6150009768959706, 250.5000000000000568, -2.367926910627514037 ) ) ;
#86749 = CARTESIAN_POINT ( 'NONE',  ( 157.4471379844592036, 15.78783268421870645, -9.037979834338015550 ) ) ;
#86750 = CARTESIAN_POINT ( 'NONE',  ( 3.346337345427247367, -290.5984256856759202, -207.2957419298513173 ) ) ;
#86751 = CARTESIAN_POINT ( 'NONE',  ( -110.4493271790812088, -282.7546704188016520, -292.2693443716538582 ) ) ;
#86752 = CARTESIAN_POINT ( 'NONE',  ( -21.46122829231144635, -278.4453977070242559, -342.4848360931924276 ) ) ;
#86753 = CARTESIAN_POINT ( 'NONE',  ( -43.64895670453570631, -287.1793433499586854, -193.9653060778406370 ) ) ;
#86754 = CARTESIAN_POINT ( 'NONE',  ( 33.08190655882897602, -287.8083413300794859, -289.7714889439299100 ) ) ;
#86755 = CARTESIAN_POINT ( 'NONE',  ( -56.73814154964617984, -278.7323140456948636, -341.4010271746753347 ) ) ;
#86756 = CARTESIAN_POINT ( 'NONE',  ( -97.01148390475290739, -278.7648996115511864, -312.7162937232749300 ) ) ;
#86757 = CARTESIAN_POINT ( 'NONE',  ( -77.47433449402109318, -287.5138048364202632, -207.0020436016884844 ) ) ;
#86758 = VERTEX_POINT ( 'NONE', #53488 ) ;
#86759 = CIRCLE ( 'NONE', #23230, 0.9999999999999954481 ) ;
#86760 = CARTESIAN_POINT ( 'NONE',  ( -110.8124856383814034, -296.6770208126011426, -247.1400003917706272 ) ) ;
#86761 = CARTESIAN_POINT ( 'NONE',  ( -0.1505256645194337772, -290.5351261920225738, -335.1405081192834245 ) ) ;
#86762 = CARTESIAN_POINT ( 'NONE',  ( 193.9153122143737562, 215.0000000000000568, 17.21343741151142126 ) ) ;
#86763 = CARTESIAN_POINT ( 'NONE',  ( -111.2869819898779866, -287.4805209788416391, -234.7871824221999191 ) ) ;
#86764 = ORIENTED_EDGE ( 'NONE', *, *, #34566, .T. ) ;
#86765 = CARTESIAN_POINT ( 'NONE',  ( 38.06331026441004894, -291.8088035336748476, -259.0280594007051604 ) ) ;
#86766 = AXIS2_PLACEMENT_3D ( 'NONE', #62546, #75789, #12329 ) ;
#86767 = CARTESIAN_POINT ( 'NONE',  ( 19.18121083802451565, -288.4071935035355523, -223.0564963105121592 ) ) ;
#86768 = PRODUCT_DEFINITION_SHAPE ( 'NONE', 'NONE',  #93716 ) ;
#86769 = CARTESIAN_POINT ( 'NONE',  ( 32.01209631713407333, -282.9705450988461166, -244.3680249718194943 ) ) ;
#86770 = CARTESIAN_POINT ( 'NONE',  ( 18.22885088892227046, -289.6991133662497191, -322.8065196151509895 ) ) ;
#86771 = CARTESIAN_POINT ( 'NONE',  ( 36.31421764920121831, -289.1288242860660489, -291.0998763137836818 ) ) ;
#86772 = CARTESIAN_POINT ( 'NONE',  ( -110.3669567502479509, -286.3321290563596904, -287.5142968913292520 ) ) ;
#86773 = CARTESIAN_POINT ( 'NONE',  ( -95.20938898244470749, -278.0314176480131323, -321.1580725288027907 ) ) ;
#86774 = ORIENTED_EDGE ( 'NONE', *, *, #73224, .F. ) ;
#86775 = CARTESIAN_POINT ( 'NONE',  ( -27.95149810235949772, -293.0138097048730970, -345.3876637607737621 ) ) ;
#86776 = CARTESIAN_POINT ( 'NONE',  ( 28.30389320523857322, -281.9124432975543755, -310.7071090440763328 ) ) ;
#86777 = TOROIDAL_SURFACE ( 'NONE', #38378, 27.00000000000000355, 3.000000000000000000 ) ;
#86778 = CARTESIAN_POINT ( 'NONE',  ( -98.88019599209147259, -274.9811132730073382, -228.7497480662936766 ) ) ;
#86779 = AXIS2_PLACEMENT_3D ( 'NONE', #33001, #17868, #90275 ) ;
#86780 = DIRECTION ( 'NONE',  ( -0.000000000000000000, -0.000000000000000000, -1.000000000000000000 ) ) ;
#86781 = CARTESIAN_POINT ( 'NONE',  ( 31.95455697924148097, -289.6233781216988064, -236.9535640164627637 ) ) ;
#86782 = CARTESIAN_POINT ( 'NONE',  ( -64.51647401274645688, -271.9421256445228323, -199.3858237804838609 ) ) ;
#86783 = DIRECTION ( 'NONE',  ( 0.6573509547581669610, 0.1665889405894028785, -0.7349407099568147084 ) ) ;
#86784 = CARTESIAN_POINT ( 'NONE',  ( -100.8622202828733663, -278.5537948022475803, -234.2621988743837278 ) ) ;
#86785 = CARTESIAN_POINT ( 'NONE',  ( 36.20029734389860465, -276.4848738137167743, -248.7379886606918262 ) ) ;
#86786 = CARTESIAN_POINT ( 'NONE',  ( -60.72015274471441160, -299.1682260567342269, -200.5302615611704766 ) ) ;
#86787 = CARTESIAN_POINT ( 'NONE',  ( -109.0873391921046078, -283.2625887709342010, -297.8110137020640877 ) ) ;
#86788 = CARTESIAN_POINT ( 'NONE',  ( -102.5251139082621847, -291.8394605150623420, -305.5281926994011314 ) ) ;
#86789 = CARTESIAN_POINT ( 'NONE',  ( 30.00702508275892200, -300.4010117140515490, -194.0373803870615461 ) ) ;
#86790 = CARTESIAN_POINT ( 'NONE',  ( -23.46477283104988132, -299.4273271954446045, -193.7554179349797892 ) ) ;
#86791 = CARTESIAN_POINT ( 'NONE',  ( 27.39099520683090461, -296.0547708562792195, -307.9071774166563955 ) ) ;
#86792 = CARTESIAN_POINT ( 'NONE',  ( -110.2163411749519497, -282.3324557182195917, -287.4264551373652239 ) ) ;
#86793 = CARTESIAN_POINT ( 'NONE',  ( -105.9833334332431605, -290.6689138343548393, -235.4000849822964199 ) ) ;
#86794 = CARTESIAN_POINT ( 'NONE',  ( -66.43140005271798998, -271.6894408729166912, -201.6178553100715192 ) ) ;
#86795 = CARTESIAN_POINT ( 'NONE',  ( -52.03915023367822812, -287.4673228406683165, -195.5381428955062404 ) ) ;
#86796 = VECTOR ( 'NONE', #89548, 1000.000000000000000 ) ;
#86797 = CARTESIAN_POINT ( 'NONE',  ( -109.7265047859118994, -289.3190001243189045, -282.0447395844415155 ) ) ;
#86798 = CARTESIAN_POINT ( 'NONE',  ( 26.75917060119040514, -23.72314211615959323, -344.9376292452095640 ) ) ;
#86799 = ORIENTED_EDGE ( 'NONE', *, *, #89695, .F. ) ;
#86800 = CARTESIAN_POINT ( 'NONE',  ( -95.20276076680376320, -289.8062189588819137, -220.4341717469561956 ) ) ;
#86801 = CARTESIAN_POINT ( 'NONE',  ( 24.25390665540478707, -287.7609755527370794, -309.5793371125305384 ) ) ;
#86802 = ORIENTED_EDGE ( 'NONE', *, *, #29222, .T. ) ;
#86803 = CARTESIAN_POINT ( 'NONE',  ( -30.92348114642763690, -287.2111067028664593, -193.9260277965745729 ) ) ;
#86804 = CARTESIAN_POINT ( 'NONE',  ( -5.052915407156727490, -276.9482994221830836, -335.8694542499625868 ) ) ;
#86805 = EDGE_CURVE ( 'NONE', #19844, #8997, #3740, .T. ) ;
#86806 = CARTESIAN_POINT ( 'NONE',  ( 39.34742160862095517, -292.4360794352614334, -267.4620593073188388 ) ) ;
#86807 = CARTESIAN_POINT ( 'NONE',  ( -101.3297067515148200, -284.6404051943337663, -313.1045985470062192 ) ) ;
#86808 = CARTESIAN_POINT ( 'NONE',  ( -93.87237594259970308, -285.3694564531878655, -321.6346665297212439 ) ) ;
#86809 = CARTESIAN_POINT ( 'NONE',  ( -95.31601251462487312, -284.2003075149974052, -321.0042161784878090 ) ) ;
#86810 = CARTESIAN_POINT ( 'NONE',  ( -4.341809925834303918, -280.8328234898870619, -205.2081816685068247 ) ) ;
#86811 = CARTESIAN_POINT ( 'NONE',  ( -110.0552246555809290, -267.0563155853889725, -307.0414417294254577 ) ) ;
#86812 = CARTESIAN_POINT ( 'NONE',  ( 200.7444845821497381, 293.5020097745142493, -83.02703438293134752 ) ) ;
#86813 = CARTESIAN_POINT ( 'NONE',  ( 197.5587112275084394, 287.0354810671433370, -96.43656103357294285 ) ) ;
#86814 = CARTESIAN_POINT ( 'NONE',  ( -46.18819073417365217, -273.1342200703788876, -197.7364573587971392 ) ) ;
#86815 = CARTESIAN_POINT ( 'NONE',  ( -36.28159082874546471, -294.5468877216721921, -347.3053693379038123 ) ) ;
#86816 = CARTESIAN_POINT ( 'NONE',  ( 168.4634583693828347, 229.6213362103191287, -190.1949568163676929 ) ) ;
#86817 = CARTESIAN_POINT ( 'NONE',  ( -34.10717456667234870, -272.7768668049313305, -193.9226713860331870 ) ) ;
#86818 = CARTESIAN_POINT ( 'NONE',  ( -109.0346373814171841, -298.6633112630831874, -251.0510198752967597 ) ) ;
#86819 = CARTESIAN_POINT ( 'NONE',  ( 35.05022486730094755, -288.6974927387190633, -257.3995368237181083 ) ) ;
#86820 = ORIENTED_EDGE ( 'NONE', *, *, #55554, .T. ) ;
#86821 = CARTESIAN_POINT ( 'NONE',  ( -96.32291540047100398, -296.8302833475544844, -319.5143980008072049 ) ) ;
#86822 = CARTESIAN_POINT ( 'NONE',  ( -87.74148201065924013, -285.8169624009063341, -217.4664072097358769 ) ) ;
#86823 = CARTESIAN_POINT ( 'NONE',  ( -38.33954403604099781, -272.9602524530000096, -193.6767204910124462 ) ) ;
#86824 = CARTESIAN_POINT ( 'NONE',  ( 21.25116090570250904, -295.0264352406897501, -320.0706287109910022 ) ) ;
#86825 = CARTESIAN_POINT ( 'NONE',  ( 13.35998917800109531, -294.8576441450132393, -328.3011454666491318 ) ) ;
#86826 = CARTESIAN_POINT ( 'NONE',  ( -109.6226499573746764, -290.5828212286703547, -280.6715567784370364 ) ) ;
#86827 = ORIENTED_EDGE ( 'NONE', *, *, #47505, .F. ) ;
#86828 = CARTESIAN_POINT ( 'NONE',  ( -89.19281939885948418, -275.2500978073297802, -215.3280607889855958 ) ) ;
#86829 = CARTESIAN_POINT ( 'NONE',  ( 30.90353918811203116, -273.8966644578293881, -235.5674974730983990 ) ) ;
#86830 = ORIENTED_EDGE ( 'NONE', *, *, #86610, .T. ) ;
#86831 = EDGE_CURVE ( 'NONE', #26085, #50388, #70271, .T. ) ;
#86832 = CARTESIAN_POINT ( 'NONE',  ( -74.97235823153418721, -279.0724059540298185, -203.2532907640478186 ) ) ;
#86833 = CARTESIAN_POINT ( 'NONE',  ( 33.66203403119889970, -274.2157071071154633, -290.5296971300207929 ) ) ;
#86834 = CARTESIAN_POINT ( 'NONE',  ( -85.52363296086240041, -274.4472104620744517, -215.0419560849965706 ) ) ;
#86835 = AXIS2_PLACEMENT_3D ( 'NONE', #68817, #25702, #76382 ) ;
#86836 = CARTESIAN_POINT ( 'NONE',  ( 13.65192824351587397, -275.7295579016390548, -217.7963168958090989 ) ) ;
#86837 = CARTESIAN_POINT ( 'NONE',  ( -97.03117657187479494, -274.9495566298397762, -223.3383530757225230 ) ) ;
#86838 = CARTESIAN_POINT ( 'NONE',  ( -15.09976078826316304, -274.7857549282261971, -342.4136820837916275 ) ) ;
#86839 = CARTESIAN_POINT ( 'NONE',  ( -70.97031699023901297, -296.1595473133397149, -335.2828156419582228 ) ) ;
#86840 = CARTESIAN_POINT ( 'NONE',  ( 17.50772934652921009, -292.8232884356419845, -319.4404309214895079 ) ) ;
#86841 = CARTESIAN_POINT ( 'NONE',  ( 0.000000000000000000, 0.000000000000000000, 9.000000000000001776 ) ) ;
#86842 = CARTESIAN_POINT ( 'NONE',  ( -96.09813322418342807, -278.3745439393069319, -320.0524527527244913 ) ) ;
#86843 = CARTESIAN_POINT ( 'NONE',  ( 34.37310310425249327, -275.5389288423594394, -256.7234128284012513 ) ) ;
#86844 = CIRCLE ( 'NONE', #46002, 0.4999999999999926170 ) ;
#86845 = CARTESIAN_POINT ( 'NONE',  ( -89.53748335026845950, -284.0200167005681919, -214.3525214772778043 ) ) ;
#86846 = CARTESIAN_POINT ( 'NONE',  ( -112.2948881186215857, -298.6331651874568820, -264.0503518517452903 ) ) ;
#86847 = CARTESIAN_POINT ( 'NONE',  ( 209.5381921119887636, 36.46041812331149856, 14.69807322781370118 ) ) ;
#86848 = CIRCLE ( 'NONE', #33939, 4.000000000000003553 ) ;
#86849 = CARTESIAN_POINT ( 'NONE',  ( -65.14513454525537384, -284.8766089075410264, -202.6346691717131137 ) ) ;
#86850 = AXIS2_PLACEMENT_3D ( 'NONE', #70195, #35601, #78683 ) ;
#86851 = ADVANCED_FACE ( 'NONE', ( #16115 ), #44966, .F. ) ;
#86852 = CARTESIAN_POINT ( 'NONE',  ( -109.5911086132750114, -277.0016840335301254, -254.2408968133752580 ) ) ;
#86853 = CARTESIAN_POINT ( 'NONE',  ( -108.7482153045041002, -276.8933796392527711, -288.2031294237057182 ) ) ;
#86854 = CARTESIAN_POINT ( 'NONE',  ( 9.529343247231585323, -284.4081899320830189, -328.9768874560066365 ) ) ;
#86855 = CARTESIAN_POINT ( 'NONE',  ( -66.94883841530983659, -278.6541538061674146, -337.5217304590391336 ) ) ;
#86856 = CARTESIAN_POINT ( 'NONE',  ( 155.4162060973606287, 20.04122387618983936, 15.25295451849726902 ) ) ;
#86858 = CARTESIAN_POINT ( 'NONE',  ( 36.45880250003939693, -274.1919467345923067, -289.3328398162641975 ) ) ;
#86857 = VECTOR ( 'NONE', #81338, 1000.000000000000000 ) ;
#86859 = CARTESIAN_POINT ( 'NONE',  ( 26.72186456130578236, -275.7220136629193803, -235.0455216226051789 ) ) ;
#86860 = CARTESIAN_POINT ( 'NONE',  ( 5.126948894184845784, -282.6251541114432939, -208.3414253479113256 ) ) ;
#86861 = DIRECTION ( 'NONE',  ( -0.000000000000000000, 1.000000000000000000, -0.000000000000000000 ) ) ;
#86862 = CARTESIAN_POINT ( 'NONE',  ( -31.90550056379007415, -290.9043498458780732, -345.7768859654386233 ) ) ;
#86863 = CARTESIAN_POINT ( 'NONE',  ( -12.74980523639072949, -290.3715224340365921, -199.4536722586505562 ) ) ;
#86864 = CONICAL_SURFACE ( 'NONE', #67285, 4.025000000000000355, 0.7853981633973095011 ) ;
#86865 = CARTESIAN_POINT ( 'NONE',  ( 82.17417184970206279, -297.5662997459467647, -195.6645840736872515 ) ) ;
#86866 = CARTESIAN_POINT ( 'NONE',  ( -94.14895943576473769, -271.8932868063695878, -223.7133553978839871 ) ) ;
#86867 = CARTESIAN_POINT ( 'NONE',  ( -109.3000413618258193, -288.9291320137709249, -252.0649630799227054 ) ) ;
#86868 = CARTESIAN_POINT ( 'NONE',  ( -43.41528170534920861, -158.9639970630164498, -364.8434004397808508 ) ) ;
#86869 = DIRECTION ( 'NONE',  ( 0.000000000000000000, -0.000000000000000000, -1.000000000000000000 ) ) ;
#86870 = CARTESIAN_POINT ( 'NONE',  ( -80.16764853839896432, -288.1000006434949796, -333.5806883127525566 ) ) ;
#86871 = CARTESIAN_POINT ( 'NONE',  ( -51.95614118675854343, -284.1075939969323940, -195.7394099293193221 ) ) ;
#86872 = CARTESIAN_POINT ( 'NONE',  ( -61.71287943140944776, -284.8002930487787694, -339.8512278002538096 ) ) ;
#86873 = EDGE_CURVE ( 'NONE', #8402, #39736, #36994, .T. ) ;
#86874 = CARTESIAN_POINT ( 'NONE',  ( -110.4797577696382689, -285.3116262416378390, -273.6555799307682264 ) ) ;
#86875 = CARTESIAN_POINT ( 'NONE',  ( -71.45080126392132058, -293.5838877526078932, -203.1532573858007709 ) ) ;
#86876 = CARTESIAN_POINT ( 'NONE',  ( -81.24181258839446684, -273.8069192882472862, -207.0626354033265386 ) ) ;
#86877 = CARTESIAN_POINT ( 'NONE',  ( -95.45538569605990631, -289.2939843182991808, -222.0491680851177989 ) ) ;
#86878 = CARTESIAN_POINT ( 'NONE',  ( -74.09684862173958209, -277.5266836087328102, -338.0374756844877879 ) ) ;
#86879 = CARTESIAN_POINT ( 'NONE',  ( 33.10045602775717555, -295.8551362106339866, -295.2091428151940136 ) ) ;
#86880 = DIRECTION ( 'NONE',  ( -1.000000000000000000, -0.000000000000000000, -0.000000000000000000 ) ) ;
#86881 = CARTESIAN_POINT ( 'NONE',  ( -95.99890600148557951, -299.6948066931273615, -223.6242672951989618 ) ) ;
#86882 = CARTESIAN_POINT ( 'NONE',  ( -4.622555397615084161, -281.2965595327100345, -336.1691801607071852 ) ) ;
#86883 = CARTESIAN_POINT ( 'NONE',  ( -111.0022715921551111, -276.3593710688597298, -285.3964256195409916 ) ) ;
#86884 = CARTESIAN_POINT ( 'NONE',  ( -67.24593133910560994, -272.1469644428377137, -200.1582354957006373 ) ) ;
#86885 = CARTESIAN_POINT ( 'NONE',  ( 28.11809138613718773, -275.3427318570775810, -303.0160785147780871 ) ) ;
#86886 = CARTESIAN_POINT ( 'NONE',  ( -38.93176445487830506, -293.5519694959696722, -196.6849383197764496 ) ) ;
#86887 = CARTESIAN_POINT ( 'NONE',  ( 28.94640993440842180, -294.0727705118734434, -239.1079720788806071 ) ) ;
#86888 = CARTESIAN_POINT ( 'NONE',  ( -30.76620544236652677, -293.5588613948452235, -194.1814413712471890 ) ) ;
#86889 = CARTESIAN_POINT ( 'NONE',  ( 36.60161389795175069, -294.6192887686886479, -250.6717627220464522 ) ) ;
#86890 = CARTESIAN_POINT ( 'NONE',  ( -93.94389333796340225, -295.7327289671717381, -316.4805664725033694 ) ) ;
#86891 = CARTESIAN_POINT ( 'NONE',  ( -48.32949609678158964, -291.1920234091790007, -344.6042970538138661 ) ) ;
#86892 = CARTESIAN_POINT ( 'NONE',  ( -113.9036362900988451, -284.6162565717947359, -278.5629431221065602 ) ) ;
#86893 = CARTESIAN_POINT ( 'NONE',  ( -3.094337321886710956, -272.6392355175495368, -202.7639322579063332 ) ) ;
#86894 = CARTESIAN_POINT ( 'NONE',  ( -9.991975442845525635, -286.2327576604603223, -198.3252044889055128 ) ) ;
#86895 = CARTESIAN_POINT ( 'NONE',  ( -110.3688160444902309, -280.3326459323677682, -285.8170924691579557 ) ) ;
#86896 = CARTESIAN_POINT ( 'NONE',  ( -49.47212374671008916, -284.6891096647627819, -197.9216119406484893 ) ) ;
#86897 = CARTESIAN_POINT ( 'NONE',  ( -18.25844294283939817, -286.8060514101995295, -342.8926969051153719 ) ) ;
#86898 = CARTESIAN_POINT ( 'NONE',  ( -79.20817858417055390, -277.6337584082548346, -207.1515144517583735 ) ) ;
#86899 = CARTESIAN_POINT ( 'NONE',  ( -117.0947446405890418, -269.4376451100752661, -283.8482964293340274 ) ) ;
#86900 = CARTESIAN_POINT ( 'NONE',  ( -93.29819437879417876, -284.7263722217711575, -223.3838980455866761 ) ) ;
#86901 = CARTESIAN_POINT ( 'NONE',  ( 39.01468303602170806, -282.6800264357202650, -264.2201516214257708 ) ) ;
#86902 = CARTESIAN_POINT ( 'NONE',  ( -99.68620203225715670, -289.0152016919855100, -315.1718484472781370 ) ) ;
#86903 = CARTESIAN_POINT ( 'NONE',  ( -105.4695610292144607, -280.5972650895556058, -236.1109301535063878 ) ) ;
#86904 = CARTESIAN_POINT ( 'NONE',  ( -62.22963551617960576, -278.6842322358107822, -342.7626824613544159 ) ) ;
#86905 = CARTESIAN_POINT ( 'NONE',  ( -87.52908431975247083, -279.1615861610893035, -217.2796927199434549 ) ) ;
#86906 = CARTESIAN_POINT ( 'NONE',  ( -95.06605684316079419, -275.1878189204332443, -223.0151754470984997 ) ) ;
#86907 = CARTESIAN_POINT ( 'NONE',  ( 34.45149188605564206, -293.9047819355489537, -298.1952262028938776 ) ) ;
#86908 = CARTESIAN_POINT ( 'NONE',  ( 22.47680562451330744, -286.1852246695798385, -315.0321769504552663 ) ) ;
#86909 = UNCERTAINTY_MEASURE_WITH_UNIT (LENGTH_MEASURE( 1.000000000000000082E-05 ), #60100, 'distance_accuracy_value', 'NONE');
#86910 = CARTESIAN_POINT ( 'NONE',  ( -96.85170157148975534, -292.7964252854051210, -222.7691002997040641 ) ) ;
#86911 = CARTESIAN_POINT ( 'NONE',  ( -84.68818116109137861, -294.6426447077963076, -326.3968497534781932 ) ) ;
#86912 = CARTESIAN_POINT ( 'NONE',  ( 35.66290118510109153, -293.2601861980901958, -273.4941095296464368 ) ) ;
#86913 = CARTESIAN_POINT ( 'NONE',  ( -108.0873074472835924, -292.0099057537805152, -240.7545046334842311 ) ) ;
#86914 = AXIS2_PLACEMENT_3D ( 'NONE', #61515, #61966, #45876 ) ;
#86915 = CARTESIAN_POINT ( 'NONE',  ( 34.80549816460538892, -282.3586966801141784, -282.1371294821126412 ) ) ;
#86916 = EDGE_CURVE ( 'NONE', #4348, #30831, #23207, .T. ) ;
#86917 = CARTESIAN_POINT ( 'NONE',  ( -35.46743192501943298, -296.9954357504116160, -193.6705618249556551 ) ) ;
#86918 = CARTESIAN_POINT ( 'NONE',  ( -6.952563875487595801, -289.3151389814750019, -341.0139497990180644 ) ) ;
#86919 = CARTESIAN_POINT ( 'NONE',  ( -101.8785350594359755, -282.1645585666854004, -310.0511975511534501 ) ) ;
#86920 = CARTESIAN_POINT ( 'NONE',  ( -105.1353412709446786, -290.4138256832785601, -306.8270817300644921 ) ) ;
#86921 = CARTESIAN_POINT ( 'NONE',  ( -37.28511670800484978, -286.3861252245957871, -197.3275536068215104 ) ) ;
#86922 = DIRECTION ( 'NONE',  ( 8.659560562354958743E-17, 0.7071067811865453523, -0.7071067811865496822 ) ) ;
#86923 = CARTESIAN_POINT ( 'NONE',  ( -57.41194557413744093, -168.5696832352114711, -362.2019297073620123 ) ) ;
#86924 = CARTESIAN_POINT ( 'NONE',  ( -102.3726955531243732, -253.9557218656232180, -324.0492224005949993 ) ) ;
#86925 = CARTESIAN_POINT ( 'NONE',  ( -110.3189945673971692, -277.8176032825532502, -265.1730332779121682 ) ) ;
#86926 = CARTESIAN_POINT ( 'NONE',  ( -16.82207620049340946, -279.2438286434855854, -199.9823491192897222 ) ) ;
#86927 = CARTESIAN_POINT ( 'NONE',  ( 25.31216207106841765, -274.6260374437338783, -225.6145479451469669 ) ) ;
#86928 = CARTESIAN_POINT ( 'NONE',  ( 195.1835355330036066, 276.0653920892696647, -124.6905694975844909 ) ) ;
#86929 = CARTESIAN_POINT ( 'NONE',  ( -38.14536149072925042, -278.6169999800464439, -193.9545709877129411 ) ) ;
#86930 = CARTESIAN_POINT ( 'NONE',  ( -18.34075180822417295, -280.8263642058910818, -342.6006431026112864 ) ) ;
#86931 = CARTESIAN_POINT ( 'NONE',  ( 8.315406922725703254, -296.1969989576587636, -331.1015706242496890 ) ) ;
#86932 = CIRCLE ( 'NONE', #80850, 1.895975569037589015 ) ;
#86933 = CARTESIAN_POINT ( 'NONE',  ( -65.35634990667689692, -292.1681717458145044, -202.8704265452473692 ) ) ;
#86934 = CARTESIAN_POINT ( 'NONE',  ( -5.594463263340846204, -287.3103928393369983, -336.6435170880935743 ) ) ;
#86935 = CARTESIAN_POINT ( 'NONE',  ( 35.63059290751954933, -275.8959179690296537, -245.9372457096550875 ) ) ;
#86936 = CARTESIAN_POINT ( 'NONE',  ( -100.1653902561143212, -296.2067918880113666, -307.6383807713285705 ) ) ;
#86937 = ORIENTED_EDGE ( 'NONE', *, *, #17248, .T. ) ;
#86938 = CARTESIAN_POINT ( 'NONE',  ( 9.339199855150265961, -212.1443419142231051, 25.50000000000000000 ) ) ;
#86939 = CARTESIAN_POINT ( 'NONE',  ( 197.1933712184921603, 24.89666632552609826, 12.64285714285713169 ) ) ;
#86940 = CARTESIAN_POINT ( 'NONE',  ( -73.10605034128096236, -281.5020973758564082, -203.7865058852713105 ) ) ;
#86941 = CARTESIAN_POINT ( 'NONE',  ( 22.35726285581571204, -282.0399586273710497, -227.8139689271587827 ) ) ;
#86942 = CARTESIAN_POINT ( 'NONE',  ( -83.96311874118413243, -281.1821475650824596, -210.2910391935556049 ) ) ;
#86943 = CARTESIAN_POINT ( 'NONE',  ( 35.92305283820380168, -280.5876029057382652, -268.5898071631148696 ) ) ;
#86944 = CARTESIAN_POINT ( 'NONE',  ( -31.26340798893588513, -272.6101549384391092, -196.9061115795442163 ) ) ;
#86945 = DIRECTION ( 'NONE',  ( 0.000000000000000000, 0.000000000000000000, -1.000000000000000000 ) ) ;
#86946 = DIRECTION ( 'NONE',  ( 0.5729786897769378884, 0.000000000000000000, -0.8195702660916291959 ) ) ;
#86947 = CARTESIAN_POINT ( 'NONE',  ( 39.46250208819142813, -276.4009146000140618, -274.0260451032287392 ) ) ;
#86948 = ORIENTED_EDGE ( 'NONE', *, *, #71792, .F. ) ;
#86949 = CARTESIAN_POINT ( 'NONE',  ( 34.65847069133043590, -277.2798301904471145, -249.1804188694425477 ) ) ;
#86950 = CARTESIAN_POINT ( 'NONE',  ( -99.18364715087494687, -276.5266253956545484, -315.2629889391303095 ) ) ;
#86951 = ORIENTED_EDGE ( 'NONE', *, *, #73573, .T. ) ;
#86952 = LINE ( 'NONE', #88345, #83717 ) ;
#86953 = CARTESIAN_POINT ( 'NONE',  ( -101.5040988635992960, -286.0042478258033043, -309.8781192586051816 ) ) ;
#86954 = CARTESIAN_POINT ( 'NONE',  ( 2.336642849746430883, -291.7955606787663783, -208.8337853208038553 ) ) ;
#86955 = CARTESIAN_POINT ( 'NONE',  ( -26.62709092398780797, -285.5334963370459036, -194.1597417034820126 ) ) ;
#86956 = CARTESIAN_POINT ( 'NONE',  ( -32.09594336733599107, -281.2249262236850313, -344.1883219797156244 ) ) ;
#86957 = CARTESIAN_POINT ( 'NONE',  ( -93.01672211941095725, -282.4465694361184092, -318.5016762859595474 ) ) ;
#86958 = CARTESIAN_POINT ( 'NONE',  ( -53.76366360659341126, -284.4725734779144091, -341.9498346190770235 ) ) ;
#86959 = CARTESIAN_POINT ( 'NONE',  ( -64.16049008565703105, -271.7021451119229027, -200.3062209477518252 ) ) ;
#86960 = CARTESIAN_POINT ( 'NONE',  ( -108.2762202343852493, -283.3101978162937939, -242.3836714580931186 ) ) ;
#86961 = CARTESIAN_POINT ( 'NONE',  ( -85.10161127984252971, -297.7116797439952620, -328.1883739475700281 ) ) ;
#86962 = CARTESIAN_POINT ( 'NONE',  ( -103.5877890818818940, -279.9153425415879042, -239.0190653664648153 ) ) ;
#86963 = CARTESIAN_POINT ( 'NONE',  ( -112.3250561810371124, -286.6284405422214263, -264.4191461670728245 ) ) ;
#86964 = CARTESIAN_POINT ( 'NONE',  ( 198.7945540180826072, 289.2625417210226146, -6.475712835924320565 ) ) ;
#86965 = CARTESIAN_POINT ( 'NONE',  ( 207.0546088034498666, 35.99211966507625959, 14.99999999999999822 ) ) ;
#86966 = CARTESIAN_POINT ( 'NONE',  ( 33.11112878676183868, -295.1180981235899594, -242.9088996363635147 ) ) ;
#86967 = CARTESIAN_POINT ( 'NONE',  ( -37.84814670879880794, -275.0583030136047000, -345.3722060482741085 ) ) ;
#86968 = CARTESIAN_POINT ( 'NONE',  ( 18.52038806274003946, -287.4713679625443206, -323.1208177864992876 ) ) ;
#86969 = CARTESIAN_POINT ( 'NONE',  ( 33.10444211210852217, -292.2403355145663113, -292.3561505787731676 ) ) ;
#86970 = CARTESIAN_POINT ( 'NONE',  ( -43.26340984704629022, -275.8133174678249588, -343.6153112563832792 ) ) ;
#86971 = CARTESIAN_POINT ( 'NONE',  ( -110.3613397655482800, -294.5172644084547642, -283.8106600007712927 ) ) ;
#86972 = CARTESIAN_POINT ( 'NONE',  ( -90.18245116389111615, -292.6004517020554090, -219.2817825534721123 ) ) ;
#86973 = CARTESIAN_POINT ( 'NONE',  ( -95.99890600148557951, -275.6948066931273615, -223.6242672951989618 ) ) ;
#86974 = CARTESIAN_POINT ( 'NONE',  ( -65.36703677767771126, -293.8917826647602851, -341.3490696980040866 ) ) ;
#86975 = CARTESIAN_POINT ( 'NONE',  ( -26.33567588664358894, -290.5100280659751206, -343.3874350281475358 ) ) ;
#86976 = CARTESIAN_POINT ( 'NONE',  ( -110.2534416265384465, -289.0639868653782969, -248.9636422866416581 ) ) ;
#86977 = CARTESIAN_POINT ( 'NONE',  ( 34.86582325785120418, -289.1640144951885532, -284.6195935761369356 ) ) ;
#86978 = ADVANCED_FACE ( 'NONE', ( #88530 ), #33562, .F. ) ;
#86979 = PLANE ( 'NONE',  #44114 ) ;
#86980 = CARTESIAN_POINT ( 'NONE',  ( -45.37003679551985869, -289.9593068960140840, -343.0807682649054300 ) ) ;
#86981 = CARTESIAN_POINT ( 'NONE',  ( 211.4629471475955427, 32.98517505407394168, 14.26380412667038655 ) ) ;
#86982 = CARTESIAN_POINT ( 'NONE',  ( -82.60560315862981895, -290.8605763411180192, -332.1606956507961286 ) ) ;
#86983 = CARTESIAN_POINT ( 'NONE',  ( -98.08669643901508550, -277.1776928089325338, -225.7472852597653343 ) ) ;
#86984 = CARTESIAN_POINT ( 'NONE',  ( -98.56212380429246878, -279.5079335254365560, -223.6726962794251676 ) ) ;
#86985 = CARTESIAN_POINT ( 'NONE',  ( -1.647712679428733340, -282.2588758213220217, -338.5643697497121138 ) ) ;
#86986 = CARTESIAN_POINT ( 'NONE',  ( 35.64158622496402273, -285.7738233004019435, -287.6365504340372468 ) ) ;
#86987 = DIRECTION ( 'NONE',  ( 0.000000000000000000, 0.000000000000000000, 1.000000000000000000 ) ) ;
#86988 = CARTESIAN_POINT ( 'NONE',  ( 36.26061997301022899, -279.5612842513538112, -260.3051696439986813 ) ) ;
#86989 = CARTESIAN_POINT ( 'NONE',  ( -62.50577743955250298, -283.7245651208776849, -199.7086597029409347 ) ) ;
#86990 = CARTESIAN_POINT ( 'NONE',  ( 193.8404911864852807, 275.6304217925664375, -124.1201752808129868 ) ) ;
#86991 = CARTESIAN_POINT ( 'NONE',  ( -112.3873194491561947, -276.8567785726466468, -284.2483146577494608 ) ) ;
#86992 = CIRCLE ( 'NONE', #82404, 2.000000000000001776 ) ;
#86993 = CARTESIAN_POINT ( 'NONE',  ( -112.2262514165583980, -283.2647117677900042, -286.9079149419546866 ) ) ;
#86994 = CARTESIAN_POINT ( 'NONE',  ( -94.74575753952395019, -273.9936287187117614, -225.0028120148074890 ) ) ;
#86995 = CARTESIAN_POINT ( 'NONE',  ( -57.89709525034378146, -293.3824679963095150, -199.4280681820043242 ) ) ;
#86996 = CARTESIAN_POINT ( 'NONE',  ( 7.611735474325791451, -299.9190521943205567, -193.8444490797695892 ) ) ;
#86997 = CARTESIAN_POINT ( 'NONE',  ( 35.37467869294165723, -275.3067595654924276, -277.0256313092192499 ) ) ;
#86998 = CARTESIAN_POINT ( 'NONE',  ( -66.81629585481445588, -297.4385148196970476, -339.3266808211263310 ) ) ;
#86999 = CARTESIAN_POINT ( 'NONE',  ( -51.68322501210588626, -289.3974450965746996, -346.0137495857400722 ) ) ;
#87000 = CARTESIAN_POINT ( 'NONE',  ( 23.92507970797107930, -280.2298337478353574, -314.6063225004766082 ) ) ;
#87001 = CARTESIAN_POINT ( 'NONE',  ( 6.497972222874298431, -292.4633888009562952, -207.0595924665827852 ) ) ;
#87002 = CARTESIAN_POINT ( 'NONE',  ( -102.6138556948706508, -290.0618516025776330, -237.0381423371707967 ) ) ;
#87003 = CARTESIAN_POINT ( 'NONE',  ( 24.83897527482761447, -292.1192734703168412, -312.2963568091732895 ) ) ;
#87004 = ORIENTED_EDGE ( 'NONE', *, *, #57049, .T. ) ;
#87005 = CARTESIAN_POINT ( 'NONE',  ( 195.2846006655043141, -165.1985023605670335, 22.50000000000000000 ) ) ;
#87006 = CARTESIAN_POINT ( 'NONE',  ( -104.7574332432651829, -290.4388306379360642, -242.0673282533112456 ) ) ;
#87007 = DIRECTION ( 'NONE',  ( -0.000000000000000000, -1.000000000000000000, -0.000000000000000000 ) ) ;
#87008 = CARTESIAN_POINT ( 'NONE',  ( -2.340916204399413392, -287.4450511932226391, -202.0253653276260479 ) ) ;
#87009 = CARTESIAN_POINT ( 'NONE',  ( -109.1418805571601069, -299.0519495502701943, -270.3937649182068412 ) ) ;
#87010 = CARTESIAN_POINT ( 'NONE',  ( 17.38536455716302598, -293.3529204309299416, -324.2676370243960378 ) ) ;
#87011 = CARTESIAN_POINT ( 'NONE',  ( -94.02246708635550476, -285.1645415923574092, -321.7672042702283761 ) ) ;
#87012 = CARTESIAN_POINT ( 'NONE',  ( -69.98052506961970209, -285.4431632047923699, -205.0501058414645001 ) ) ;
#87013 = CARTESIAN_POINT ( 'NONE',  ( 34.57409704039786646, -277.2832580352981040, -286.5066311276393662 ) ) ;
#87014 = CARTESIAN_POINT ( 'NONE',  ( -2.395542853222797142, -292.6074731187071620, -336.3202939689280129 ) ) ;
#87015 = CARTESIAN_POINT ( 'NONE',  ( 26.68028261265103396, -295.8147902596743961, -307.4981579518927788 ) ) ;
#87016 = CARTESIAN_POINT ( 'NONE',  ( 17.72301747027863783, -275.0365047420391988, -318.9084919940676741 ) ) ;
#87017 = EDGE_LOOP ( 'NONE', ( #86223, #47655, #32566, #1634 ) ) ;
#87018 = CARTESIAN_POINT ( 'NONE',  ( 196.8702642586142986, 40.96915988761479355, 12.42857142857142350 ) ) ;
#87019 = CARTESIAN_POINT ( 'NONE',  ( -47.63294801514003751, -294.8463092448595262, -346.6489578287052495 ) ) ;
#87020 = CARTESIAN_POINT ( 'NONE',  ( 22.34241534179654209, -290.0846403591799572, -314.8697723763079352 ) ) ;
#87021 = CARTESIAN_POINT ( 'NONE',  ( 201.1758259809593596, 294.8492306316788927, -54.00000000001604405 ) ) ;
#87022 = CARTESIAN_POINT ( 'NONE',  ( -110.5007710126116365, -297.3410710553436047, -293.4103266072941096 ) ) ;
#87023 = CARTESIAN_POINT ( 'NONE',  ( 31.93455021491516632, -287.8939574015018934, -247.0224417871119726 ) ) ;
#87024 = CARTESIAN_POINT ( 'NONE',  ( -111.5006029407103370, -277.8605462609007759, -250.4791783278814705 ) ) ;
#87025 = CARTESIAN_POINT ( 'NONE',  ( -41.93117385229657401, -295.7598318103241013, -347.1744318594986112 ) ) ;
#87026 = CARTESIAN_POINT ( 'NONE',  ( -84.41606186059408401, -287.8313947895858860, -329.7939702951457548 ) ) ;
#87027 = CARTESIAN_POINT ( 'NONE',  ( -108.3538937382227516, -296.5058244838007226, -300.2145888350063387 ) ) ;
#87028 = CARTESIAN_POINT ( 'NONE',  ( 209.6287663260175975, 29.00782453271232697, 12.09245862095555601 ) ) ;
#87029 = DIRECTION ( 'NONE',  ( 0.000000000000000000, 0.000000000000000000, 1.000000000000000000 ) ) ;
#87030 = CARTESIAN_POINT ( 'NONE',  ( 189.4028190526519779, 267.9912538632855785, -137.5853595571369965 ) ) ;
#87031 = CARTESIAN_POINT ( 'NONE',  ( -21.15012816928218697, -287.7763675391628908, -195.7920845411168216 ) ) ;
#87032 = CARTESIAN_POINT ( 'NONE',  ( 36.60358173371529489, -290.6237833571632905, -234.7871824221999191 ) ) ;
#87033 = ORIENTED_EDGE ( 'NONE', *, *, #87263, .F. ) ;
#87034 = ADVANCED_FACE ( 'NONE', ( #47284 ), #19780, .T. ) ;
#87035 = CARTESIAN_POINT ( 'NONE',  ( -112.8944733477863309, -278.0809647510012610, -255.9697284346143533 ) ) ;
#87036 = CARTESIAN_POINT ( 'NONE',  ( -95.69909136722677090, -285.9062825057794726, -317.2263788409240419 ) ) ;
#87037 = EDGE_CURVE ( 'NONE', #31343, #63802, #11303, .T. ) ;
#87038 = CARTESIAN_POINT ( 'NONE',  ( -97.10808725633442862, -283.7692305905869716, -222.7524500176436391 ) ) ;
#87039 = CARTESIAN_POINT ( 'NONE',  ( -73.07109516919334169, -287.6094922979007720, -335.6659763733678687 ) ) ;
#87040 = CARTESIAN_POINT ( 'NONE',  ( 23.39194428265797043, -278.0249123827697417, -315.6571434105271123 ) ) ;
#87041 = CARTESIAN_POINT ( 'NONE',  ( -108.9437786015251817, -296.8521621837246585, -284.9537369827323232 ) ) ;
#87042 = ORIENTED_EDGE ( 'NONE', *, *, #9842, .F. ) ;
#87043 = CARTESIAN_POINT ( 'NONE',  ( -67.51287524442672350, -294.1412501299630549, -337.3894218181170004 ) ) ;
#87044 = CARTESIAN_POINT ( 'NONE',  ( -22.59386719112204034, -280.8874469842747317, -194.8363170886761111 ) ) ;
#87046 = CARTESIAN_POINT ( 'NONE',  ( -79.10631899854433868, -278.8205096865286805, -210.3643740832142726 ) ) ;
#87045 = CARTESIAN_POINT ( 'NONE',  ( -110.3511811492682284, -278.5845093988793337, -267.9082630551762918 ) ) ;
#87047 = CARTESIAN_POINT ( 'NONE',  ( 11.57790059813620509, -275.7919959780149384, -211.2297373291249869 ) ) ;
#87048 = CARTESIAN_POINT ( 'NONE',  ( -28.64978108595942530, -275.8648454504322558, -346.6112166353418615 ) ) ;
#87049 = LINE ( 'NONE', #52461, #80920 ) ;
#87050 = CARTESIAN_POINT ( 'NONE',  ( -54.27093570039709647, -275.2692864570307734, -343.4781719471016004 ) ) ;
#87051 = CARTESIAN_POINT ( 'NONE',  ( -106.6244182717853448, -297.5617832728611916, -302.5870587432296475 ) ) ;
#87052 = CARTESIAN_POINT ( 'NONE',  ( 35.78497577281001440, -278.2662352645559167, -287.0191576251351080 ) ) ;
#87053 = CARTESIAN_POINT ( 'NONE',  ( -47.20788896421541381, -156.8319029772612225, -362.3615984655540387 ) ) ;
#87054 = CARTESIAN_POINT ( 'NONE',  ( -27.80991693150940591, -287.2557188261831698, -197.6743160014825946 ) ) ;
#87055 = CARTESIAN_POINT ( 'NONE',  ( -57.50885758819714511, -287.5555889590203265, -197.0449057537632598 ) ) ;
#87056 = CARTESIAN_POINT ( 'NONE',  ( 33.17803229305736323, -287.1570333691416295, -289.8066071122917720 ) ) ;
#87057 = CARTESIAN_POINT ( 'NONE',  ( -111.0802993045079319, -276.9127413090307641, -273.3710024826641529 ) ) ;
#87058 = CARTESIAN_POINT ( 'NONE',  ( -104.6146896406658016, -286.8307805137546893, -238.8511167778089828 ) ) ;
#87059 = CARTESIAN_POINT ( 'NONE',  ( -108.2805216480688415, -277.2939342212549718, -250.3546492497199552 ) ) ;
#87060 = CARTESIAN_POINT ( 'NONE',  ( -11.06216349228297879, -278.0174523273245200, -338.9951433077949332 ) ) ;
#87061 = CARTESIAN_POINT ( 'NONE',  ( 15.48695484835621272, -275.3164036159712964, -219.8188731429957556 ) ) ;
#87062 = CARTESIAN_POINT ( 'NONE',  ( 39.20672379671495378, -286.3980690455695708, -274.4172908513317566 ) ) ;
#87063 = MECHANICAL_DESIGN_GEOMETRIC_PRESENTATION_REPRESENTATION (  '', ( #26576 ), #70405 ) ;
#87064 = CARTESIAN_POINT ( 'NONE',  ( 31.87156146139217583, -281.9245724303455063, -236.8668499724868184 ) ) ;
#87065 = CARTESIAN_POINT ( 'NONE',  ( 37.48998451762362549, -282.2689636264242381, -288.2987734089523997 ) ) ;
#87066 = ORIENTED_EDGE ( 'NONE', *, *, #36488, .F. ) ;
#87067 = ORIENTED_EDGE ( 'NONE', *, *, #70399, .T. ) ;
#87068 = DIRECTION ( 'NONE',  ( 1.000000000000000000, 0.000000000000000000, -0.000000000000000000 ) ) ;
#87069 = CARTESIAN_POINT ( 'NONE',  ( -12.60427254789684604, -290.5944431088615261, -342.0287051547421697 ) ) ;
#87070 = CARTESIAN_POINT ( 'NONE',  ( -80.27779731921161499, -288.3049155917591975, -333.7480283163351373 ) ) ;
#87071 = CARTESIAN_POINT ( 'NONE',  ( -71.69494316103349263, -297.0986235452331243, -338.3779917053607846 ) ) ;
#87072 = CARTESIAN_POINT ( 'NONE',  ( -93.08511059206676919, -272.2845389004573917, -222.8435468249676887 ) ) ;
#87073 = CARTESIAN_POINT ( 'NONE',  ( -13.88963751095280408, -291.6971190372616434, -197.0705678946828243 ) ) ;
#87074 = CARTESIAN_POINT ( 'NONE',  ( 35.25378180290265817, -285.8626547997351963, -257.3998924987257055 ) ) ;
#87075 = CARTESIAN_POINT ( 'NONE',  ( -41.62943686792771558, -290.2374042891395902, -196.4215450113670443 ) ) ;
#87076 = CARTESIAN_POINT ( 'NONE',  ( 24.58153917179780024, -289.2990844575876963, -309.7647084178387900 ) ) ;
#87077 = CARTESIAN_POINT ( 'NONE',  ( -95.95921662488163406, -292.4090924074130839, -317.1477375740089997 ) ) ;
#87078 = CARTESIAN_POINT ( 'NONE',  ( 27.19604713815770225, -290.0633536425456214, -308.5694917326212590 ) ) ;
#87079 = CARTESIAN_POINT ( 'NONE',  ( -110.2108464810266071, -288.7889813426107253, -251.8671125422930004 ) ) ;
#87080 = CARTESIAN_POINT ( 'NONE',  ( 15.19916572695814949, -294.7935788443522824, -216.7692228310467328 ) ) ;
#87081 = CARTESIAN_POINT ( 'NONE',  ( -109.6553682008042472, -285.6467479481958094, -258.6996405168739557 ) ) ;
#87082 = CARTESIAN_POINT ( 'NONE',  ( 37.03396929114710190, -295.4085114556111193, -259.1366410626119432 ) ) ;
#87083 = CARTESIAN_POINT ( 'NONE',  ( -114.2951601902143608, -272.0832046287694652, -270.3551471570179956 ) ) ;
#87084 = DIRECTION ( 'NONE',  ( -0.5877852522924792433, 0.000000000000000000, -0.8090169943749430104 ) ) ;
#87085 = CARTESIAN_POINT ( 'NONE',  ( -26.49281569206767628, -300.1071026503124131, -194.7975931931764535 ) ) ;
#87086 = CARTESIAN_POINT ( 'NONE',  ( 31.50307961130697976, -281.0801043631039988, -295.2696458960037944 ) ) ;
#87087 = CARTESIAN_POINT ( 'NONE',  ( -45.89210104889916408, -281.1602700858851449, -344.9245251598084110 ) ) ;
#87088 = CARTESIAN_POINT ( 'NONE',  ( -114.0732210017862798, -295.6871888938720190, -275.3187444137123521 ) ) ;
#87089 = CARTESIAN_POINT ( 'NONE',  ( -4.843157671766616268, -272.7259712287394677, -203.8503419411900097 ) ) ;
#87090 = CARTESIAN_POINT ( 'NONE',  ( -62.29512720161778105, -275.4589498511286365, -340.5489471361688629 ) ) ;
#87091 = CARTESIAN_POINT ( 'NONE',  ( -95.69075116023063288, -298.4919283886091534, -225.6569217723902625 ) ) ;
#87092 = CARTESIAN_POINT ( 'NONE',  ( -43.97339029149914325, -272.5447403110272830, -194.1857708260686195 ) ) ;
#87093 = CARTESIAN_POINT ( 'NONE',  ( -113.3531685960080608, -294.7659223054623112, -272.4196762500802720 ) ) ;
#87094 = CARTESIAN_POINT ( 'NONE',  ( -31.53792181364288538, -296.4028650608722728, -343.7716455480905893 ) ) ;
#87095 = CARTESIAN_POINT ( 'NONE',  ( 222.4306832106270804, -147.4436952405746979, -21.50000000000000000 ) ) ;
#87096 = CARTESIAN_POINT ( 'NONE',  ( -73.37304601109943292, -296.3460879544666113, -334.0348475812049287 ) ) ;
#87097 = CARTESIAN_POINT ( 'NONE',  ( 200.4892204403996345, 64.44609543878858915, 7.254661561168179951 ) ) ;
#87099 = CARTESIAN_POINT ( 'NONE',  ( -88.12574357754172638, -297.3174204619543843, -217.8502831476394022 ) ) ;
#87098 = CARTESIAN_POINT ( 'NONE',  ( -96.27787509257909448, -283.2147005265668440, -223.4043922827694075 ) ) ;
#87100 = CARTESIAN_POINT ( 'NONE',  ( -111.8749650846900607, -284.3095831587860403, -289.7471031355258901 ) ) ;
#87101 = CARTESIAN_POINT ( 'NONE',  ( 23.11786949616666220, -284.0869466274041315, -315.6816943435726444 ) ) ;
#87102 = CARTESIAN_POINT ( 'NONE',  ( 31.40481746806630170, -286.7730608759853226, -235.7250008526249019 ) ) ;
#87103 = CARTESIAN_POINT ( 'NONE',  ( 30.40890565665472778, -291.1318313133708671, -238.4600631311398615 ) ) ;
#87104 = CARTESIAN_POINT ( 'NONE',  ( -111.1792401077926655, -278.0164947493470891, -249.0966755861460342 ) ) ;
#87105 = CARTESIAN_POINT ( 'NONE',  ( -69.85430415644619018, -271.1237833571632905, -202.7746430608542312 ) ) ;
#87106 = CARTESIAN_POINT ( 'NONE',  ( 120.8395553409046528, -299.5541904835127980, -195.3611179825600175 ) ) ;
#87107 = CARTESIAN_POINT ( 'NONE',  ( 33.77710695988081824, -286.1082654230667117, -252.1652155683320018 ) ) ;
#87109 = CARTESIAN_POINT ( 'NONE',  ( 196.8803347170859865, 73.40565171261611965, -12.50000000000000000 ) ) ;
#87108 = CARTESIAN_POINT ( 'NONE',  ( -113.9432164640101774, -289.4260050711258145, -274.0624966428848666 ) ) ;
#87110 = DIRECTION ( 'NONE',  ( 0.000000000000000000, 0.000000000000000000, -1.000000000000000000 ) ) ;
#87111 = CARTESIAN_POINT ( 'NONE',  ( -77.48974504741970293, -279.0045281773539045, -335.4359859423503849 ) ) ;
#87113 = CARTESIAN_POINT ( 'NONE',  ( 19.36577322110076338, -281.8698058694361634, -316.3846295146207694 ) ) ;
#87112 = CARTESIAN_POINT ( 'NONE',  ( -110.3807832951234644, -294.3346195551673645, -288.9524052189986492 ) ) ;
#87114 = CARTESIAN_POINT ( 'NONE',  ( -30.58883720292238451, -295.1356695334509368, -347.0644350348135845 ) ) ;
#87115 = CARTESIAN_POINT ( 'NONE',  ( -97.83034029730403347, -281.1571022390884309, -225.9984249545709076 ) ) ;
#87116 = CARTESIAN_POINT ( 'NONE',  ( -110.4772675662958505, -295.5606560976330570, -274.1817492113691515 ) ) ;
#87117 = VERTEX_POINT ( 'NONE', #5177 ) ;
#87118 = CARTESIAN_POINT ( 'NONE',  ( 170.2305261370685798, 275.0000000000000568, -24.90909090909090295 ) ) ;
#87119 = CARTESIAN_POINT ( 'NONE',  ( -5.304633972890733240, -284.6084617901147453, -337.7953044748188063 ) ) ;
#87120 = DIRECTION ( 'NONE',  ( 0.000000000000000000, 0.000000000000000000, 1.000000000000000000 ) ) ;
#87121 = CARTESIAN_POINT ( 'NONE',  ( -37.30987171927208834, -295.5523547857347353, -195.3611179825600175 ) ) ;
#87122 = CARTESIAN_POINT ( 'NONE',  ( -36.93030901808022293, -273.2543841515934560, -193.5106700426319435 ) ) ;
#87123 = CARTESIAN_POINT ( 'NONE',  ( -109.7897746165363912, -290.2672776954267420, -279.3208337936673615 ) ) ;
#87124 = CARTESIAN_POINT ( 'NONE',  ( 19.35726196656250764, -282.4107136871275543, -223.2678162970068456 ) ) ;
#87125 = CIRCLE ( 'NONE', #68962, 1.000000000000000888 ) ;
#87126 = CARTESIAN_POINT ( 'NONE',  ( 17.87065506638449364, -276.4593907467981353, -221.3156728368727215 ) ) ;
#87127 = CARTESIAN_POINT ( 'NONE',  ( -30.26865301048117729, -284.5642067740689072, -346.2321428832173069 ) ) ;
#87128 = CARTESIAN_POINT ( 'NONE',  ( 35.42854188223928702, -280.2165187571731053, -260.4106963311598406 ) ) ;
#87129 = CARTESIAN_POINT ( 'NONE',  ( -96.38059613480717758, -281.1872334106495828, -224.0866872121109736 ) ) ;
#87130 = CARTESIAN_POINT ( 'NONE',  ( -23.35982626625671088, -298.2226792870364989, -193.3611167184400017 ) ) ;
#87131 = CARTESIAN_POINT ( 'NONE',  ( 18.09107174954792185, -274.6530169926743952, -216.8410750332150201 ) ) ;
#87132 = CARTESIAN_POINT ( 'NONE',  ( -2.447522372816185676, -296.5068889811529971, -336.1160460021952758 ) ) ;
#87133 = CARTESIAN_POINT ( 'NONE',  ( 202.8019728163925492, 61.40723988820082013, -6.999999999999999112 ) ) ;
#87134 = LINE ( 'NONE', #93315, #60230 ) ;
#87135 = CARTESIAN_POINT ( 'NONE',  ( -50.28027257718496656, -293.3550626916551209, -345.0660504698409454 ) ) ;
#87136 = CARTESIAN_POINT ( 'NONE',  ( -87.37087880576848420, -272.8395320939962403, -217.0464830100559652 ) ) ;
#87137 = CARTESIAN_POINT ( 'NONE',  ( -47.66889549982923313, -293.4433888506345625, -194.7031979721988932 ) ) ;
#87139 = CARTESIAN_POINT ( 'NONE',  ( 23.64972068570362751, -294.1361410877461253, -223.9924203886815803 ) ) ;
#87138 = CARTESIAN_POINT ( 'NONE',  ( 10.64812456238590066, -278.9090924074130839, -330.4860931364851808 ) ) ;
#87140 = EDGE_CURVE ( 'NONE', #49115, #34721, #22756, .T. ) ;
#87141 = CARTESIAN_POINT ( 'NONE',  ( 23.46592035992629377, -290.1470718755962253, -313.9783361296704811 ) ) ;
#87142 = CARTESIAN_POINT ( 'NONE',  ( 35.67666471611626378, -273.7635456059043122, -286.8005948857149860 ) ) ;
#87143 = CARTESIAN_POINT ( 'NONE',  ( -54.25785754193617549, -279.1911149806169874, -342.9067508370486621 ) ) ;
#87144 = CARTESIAN_POINT ( 'NONE',  ( 31.91651186019259256, -291.9915118503744793, -297.7896536970665693 ) ) ;
#87145 = CARTESIAN_POINT ( 'NONE',  ( 25.70735001552274923, -283.9745544798616379, -312.3744820030636902 ) ) ;
#87146 = ORIENTED_EDGE ( 'NONE', *, *, #22273, .T. ) ;
#87147 = CARTESIAN_POINT ( 'NONE',  ( -45.64608678021451027, -282.8268807630514061, -342.9595229892038901 ) ) ;
#87148 = CARTESIAN_POINT ( 'NONE',  ( -35.35785991662786643, -281.1561399079281500, -193.6828076952699291 ) ) ;
#87149 = CARTESIAN_POINT ( 'NONE',  ( -78.95694937922455381, -282.3948665894953933, -334.6742562024286940 ) ) ;
#87150 = CARTESIAN_POINT ( 'NONE',  ( -9.286615870786235405, -277.6354584490172783, -341.8155262461882558 ) ) ;
#87151 = DIRECTION ( 'NONE',  ( 1.000000000000000000, 0.000000000000000000, 0.000000000000000000 ) ) ;
#87152 = CARTESIAN_POINT ( 'NONE',  ( 18.40998617398158288, -277.7892767476644735, -322.4615712163483749 ) ) ;
#87153 = EDGE_CURVE ( 'NONE', #28617, #56465, #77829, .T. ) ;
#87154 = CARTESIAN_POINT ( 'NONE',  ( 30.91033621190086578, -290.2662352645559167, -285.9065529553535612 ) ) ;
#87155 = ORIENTED_EDGE ( 'NONE', *, *, #64747, .F. ) ;
#87156 = CARTESIAN_POINT ( 'NONE',  ( -96.89220901608568681, -299.1768040567841354, -224.7470093052217521 ) ) ;
#87157 = CARTESIAN_POINT ( 'NONE',  ( -96.59368509299753214, -275.9476666652178096, -315.7598964236245251 ) ) ;
#87158 = CARTESIAN_POINT ( 'NONE',  ( -70.47635915819078889, -293.3814465750955947, -201.9793339401152252 ) ) ;
#87159 = CARTESIAN_POINT ( 'NONE',  ( 6.116887529115544453, -293.7935981579256577, -329.2055190867316128 ) ) ;
#87160 = CARTESIAN_POINT ( 'NONE',  ( 27.38962620700064576, -287.6069102190861031, -312.0451817811361366 ) ) ;
#87161 = CARTESIAN_POINT ( 'NONE',  ( 138.6539576904058606, 250.5000000000000568, -10.49999999999999822 ) ) ;
#87163 = CARTESIAN_POINT ( 'NONE',  ( -108.8736165782340208, -282.7149901221792447, -288.5167051683990849 ) ) ;
#87162 = CARTESIAN_POINT ( 'NONE',  ( -50.38493665318376458, -293.7901362928752746, -345.7039622598906590 ) ) ;
#87164 = CARTESIAN_POINT ( 'NONE',  ( -50.95511739685161245, -291.0882253555936927, -343.3899680524128826 ) ) ;
#87165 = CARTESIAN_POINT ( 'NONE',  ( -77.40995748873682203, -283.9842074098854710, -208.4520365991952247 ) ) ;
#87166 = CARTESIAN_POINT ( 'NONE',  ( -36.16897720810293038, -284.3523203412029261, -343.8449134781333214 ) ) ;
#87167 = CARTESIAN_POINT ( 'NONE',  ( -98.83344105714425609, -290.8799114488745090, -316.3348478844704346 ) ) ;
#87168 = CARTESIAN_POINT ( 'NONE',  ( 30.07586868192587204, -281.6670994347393275, -242.2033507195215520 ) ) ;
#87169 = CARTESIAN_POINT ( 'NONE',  ( -37.70258949093786782, -293.8514716091232231, -346.9762075267503860 ) ) ;
#87170 = CARTESIAN_POINT ( 'NONE',  ( 3.103851776506648896, -289.3268164014589274, -335.7558910395454745 ) ) ;
#87171 = CARTESIAN_POINT ( 'NONE',  ( 35.89110286209584189, -288.3413872990493587, -293.9510198350824908 ) ) ;
#87172 = CARTESIAN_POINT ( 'NONE',  ( -85.72773610322461479, -285.5270718311205087, -215.6328594001012959 ) ) ;
#87173 = ORIENTED_EDGE ( 'NONE', *, *, #37333, .T. ) ;
#87174 = CARTESIAN_POINT ( 'NONE',  ( 195.2948010944529926, 25.74157531710192259, 13.17633069842077909 ) ) ;
#87175 = CARTESIAN_POINT ( 'NONE',  ( 22.21565044364082553, -296.0492245353190697, -317.2138473581729272 ) ) ;
#87176 = CARTESIAN_POINT ( 'NONE',  ( -58.72962035045954821, -294.0078287156442229, -343.8728224411968881 ) ) ;
#87177 = CARTESIAN_POINT ( 'NONE',  ( -102.0704635766277022, -277.1457623696255155, -304.6189000161161857 ) ) ;
#87178 = CARTESIAN_POINT ( 'NONE',  ( -66.19831783440207573, -273.1920785887881493, -199.0249959068005126 ) ) ;
#87179 = CARTESIAN_POINT ( 'NONE',  ( 6.459642732922678654, -292.9250292024290161, -329.6880967489092882 ) ) ;
#87180 = CARTESIAN_POINT ( 'NONE',  ( 14.18629278656914749, -276.5483151905087880, -217.2307127665802113 ) ) ;
#87181 = CARTESIAN_POINT ( 'NONE',  ( -63.72391872432801563, -271.8441288913015796, -200.9583209718786350 ) ) ;
#87182 = CARTESIAN_POINT ( 'NONE',  ( 20.84734080478926188, -295.3835978332341483, -315.1160951734532318 ) ) ;
#87183 = CARTESIAN_POINT ( 'NONE',  ( 35.01683525324736479, -294.4762225124824795, -258.5154492406280156 ) ) ;
#87184 = CARTESIAN_POINT ( 'NONE',  ( -43.29223561230568151, -273.4430627291207543, -431.9941326777201880 ) ) ;
#87185 = CARTESIAN_POINT ( 'NONE',  ( -109.0561248548955149, -294.8438361494001470, -247.6705587521980192 ) ) ;
#87186 = CARTESIAN_POINT ( 'NONE',  ( -109.9526215170702983, -273.6725390570174454, -245.2252289925691002 ) ) ;
#87187 = CARTESIAN_POINT ( 'NONE',  ( -42.66910236538571866, -290.0621225498153422, -343.4531556601870648 ) ) ;
#87188 = CARTESIAN_POINT ( 'NONE',  ( -93.95624647803359153, -296.2326091545078839, -316.4988844709282034 ) ) ;
#87189 = CARTESIAN_POINT ( 'NONE',  ( -110.5706760458231486, -280.3042047991052073, -288.1893392489516827 ) ) ;
#87190 = CARTESIAN_POINT ( 'NONE',  ( -112.3137577669544243, -277.0442467264654169, -285.6735146127546159 ) ) ;
#87191 = CARTESIAN_POINT ( 'NONE',  ( 11.42154817797827704, -281.7452453484582406, -329.8897384340091321 ) ) ;
#87192 = CARTESIAN_POINT ( 'NONE',  ( 13.90273716865263864, -274.0970986852495912, -212.9547943688261569 ) ) ;
#87193 = CARTESIAN_POINT ( 'NONE',  ( -45.82743490355252902, -281.2402636095860089, -344.3678791785675344 ) ) ;
#87194 = CARTESIAN_POINT ( 'NONE',  ( -104.0829795028111135, -277.4333052205451509, -233.5909936821545330 ) ) ;
#87195 = CARTESIAN_POINT ( 'NONE',  ( 2.863406806513552727, -278.5897569061328909, -206.7891693712074925 ) ) ;
#87196 = CARTESIAN_POINT ( 'NONE',  ( -80.00078017821981291, -296.1460110460122905, -210.5159313249120601 ) ) ;
#87197 = CARTESIAN_POINT ( 'NONE',  ( -4.295077914976588751, -276.4878083470302386, -203.0201134692841833 ) ) ;
#87198 = CARTESIAN_POINT ( 'NONE',  ( 196.8803347170859865, 20.19615242270636557, -12.49999999999999289 ) ) ;
#87199 = CARTESIAN_POINT ( 'NONE',  ( -37.76004497004281291, -290.0670494313489485, -195.0070749915740009 ) ) ;
#87200 = CARTESIAN_POINT ( 'NONE',  ( -43.18229547018431447, -289.1239828260511331, -347.1392883570213144 ) ) ;
#87201 = CARTESIAN_POINT ( 'NONE',  ( 12.72392577116737655, -276.7482455560452195, -214.2250033927584241 ) ) ;
#87202 = CARTESIAN_POINT ( 'NONE',  ( -61.07376076949173438, -295.7433451161675180, -199.3357716021132262 ) ) ;
#87203 = CARTESIAN_POINT ( 'NONE',  ( -111.7212414572205716, -283.5068803817931666, -289.6965311120846422 ) ) ;
#87204 = FACE_BOUND ( 'NONE', #12043, .T. ) ;
#87205 = CARTESIAN_POINT ( 'NONE',  ( -74.34580869418557825, -283.5600276426087021, -205.1107906316208016 ) ) ;
#87206 = CARTESIAN_POINT ( 'NONE',  ( -114.0438498160389287, -273.6021560138187851, -270.3744733279939965 ) ) ;
#87207 = CARTESIAN_POINT ( 'NONE',  ( 0.1248664753035984842, -291.3579588099480588, -207.2470395860473218 ) ) ;
#87208 = CARTESIAN_POINT ( 'NONE',  ( -44.11386370735301909, -284.1051911836536306, -196.4354574813377781 ) ) ;
#87209 = DIRECTION ( 'NONE',  ( 0.000000000000000000, 0.000000000000000000, 1.000000000000000000 ) ) ;
#87210 = FACE_OUTER_BOUND ( 'NONE', #38262, .T. ) ;
#87211 = CARTESIAN_POINT ( 'NONE',  ( 20.91498251029369726, -290.9013635880187962, -223.1056449038877929 ) ) ;
#87212 = CARTESIAN_POINT ( 'NONE',  ( -68.91738896012196847, -281.9396976273079076, -339.8425449067846102 ) ) ;
#87213 = CARTESIAN_POINT ( 'NONE',  ( -10.94911688531545302, -278.3023607232528889, -339.2804328735938952 ) ) ;
#87214 = CARTESIAN_POINT ( 'NONE',  ( -73.43954003664197216, -286.7896081581682779, -202.7379149654411208 ) ) ;
#87215 = CARTESIAN_POINT ( 'NONE',  ( -108.6649057187028404, -284.7581362593735435, -254.7463981876746857 ) ) ;
#87216 = EDGE_CURVE ( 'NONE', #6380, #51697, #4227, .T. ) ;
#87217 = CARTESIAN_POINT ( 'NONE',  ( -43.23633775017284364, -278.5533215880736861, -343.7138831971363970 ) ) ;
#87218 = CARTESIAN_POINT ( 'NONE',  ( -92.33656088284212160, -280.0423235944534781, -222.0909738850105839 ) ) ;
#87219 = CARTESIAN_POINT ( 'NONE',  ( -97.74894308766454287, -287.1595758922238701, -225.8237952280231866 ) ) ;
#87220 = ORIENTED_EDGE ( 'NONE', *, *, #17969, .T. ) ;
#87221 = DIRECTION ( 'NONE',  ( 1.000000000000000000, -0.000000000000000000, 5.880589007913310608E-16 ) ) ;
#87222 = CARTESIAN_POINT ( 'NONE',  ( -113.7745233062622674, -296.5021401980130804, -261.0324768428683342 ) ) ;
#87223 = CARTESIAN_POINT ( 'NONE',  ( 32.02277743232583163, -289.8944956478781592, -298.0762873916737021 ) ) ;
#87224 = CARTESIAN_POINT ( 'NONE',  ( 197.2554367620029439, 24.42492926436516498, 11.92185234729253374 ) ) ;
#87225 = CARTESIAN_POINT ( 'NONE',  ( 25.22466315766300227, -284.6948066931273047, -320.2154176792147382 ) ) ;
#87226 = CARTESIAN_POINT ( 'NONE',  ( -111.8780292072525668, -277.2451370597510163, -288.4668726249474844 ) ) ;
#87227 = CARTESIAN_POINT ( 'NONE',  ( 18.83975353840251898, -291.2443608084994366, -218.8821448026533858 ) ) ;
#87228 = CARTESIAN_POINT ( 'NONE',  ( 35.68048966333870453, -288.9377479172994185, -260.0660241030690258 ) ) ;
#87229 = CARTESIAN_POINT ( 'NONE',  ( -109.6009009841024948, -280.5213961754714092, -254.2848444726273840 ) ) ;
#87230 = CARTESIAN_POINT ( 'NONE',  ( 19.83368846760263438, -288.2847123798981670, -219.5919977501857261 ) ) ;
#87231 = CARTESIAN_POINT ( 'NONE',  ( -111.5958314136155707, -286.6877879851134026, -259.8100689390566913 ) ) ;
#87232 = CARTESIAN_POINT ( 'NONE',  ( -91.32752230076842181, -277.9608483952919755, -325.3405278219412935 ) ) ;
#87233 = ORIENTED_EDGE ( 'NONE', *, *, #22107, .T. ) ;
#87234 = CARTESIAN_POINT ( 'NONE',  ( -111.3932513481078956, -270.6953707840982588, -259.2191041581176023 ) ) ;
#87235 = VECTOR ( 'NONE', #32658, 1000.000000000000000 ) ;
#87236 = CARTESIAN_POINT ( 'NONE',  ( 37.79695028007690638, -291.5243124805288062, -261.9116984636203824 ) ) ;
#87237 = CARTESIAN_POINT ( 'NONE',  ( -73.76376950850132630, -279.4156004762390353, -202.5049346635564120 ) ) ;
#87238 = CARTESIAN_POINT ( 'NONE',  ( -16.31307777119193148, -276.1871447150635390, -199.1129837178100388 ) ) ;
#87239 = CARTESIAN_POINT ( 'NONE',  ( 154.7156223832783724, 19.57420759269780319, 12.98093464719297074 ) ) ;
#87240 = ADVANCED_FACE ( 'NONE', ( #61993 ), #41595, .F. ) ;
#87241 = CARTESIAN_POINT ( 'NONE',  ( -106.6662871844225293, -293.4805209788415823, -237.0123917617630980 ) ) ;
#87242 = CARTESIAN_POINT ( 'NONE',  ( -95.24082199233411927, -271.4644771141079787, -221.1306688775227656 ) ) ;
#87243 = DIRECTION ( 'NONE',  ( -0.000000000000000000, -0.000000000000000000, 1.000000000000000000 ) ) ;
#87244 = CARTESIAN_POINT ( 'NONE',  ( -108.9463045563752530, -278.2519848656275485, -255.7804320126150230 ) ) ;
#87245 = CARTESIAN_POINT ( 'NONE',  ( -5.436094395339358343, -277.8467150533444965, -340.0033540384137609 ) ) ;
#87246 = CARTESIAN_POINT ( 'NONE',  ( -71.95809676584293868, -299.0103631228081440, -205.4077555996138358 ) ) ;
#87247 = CARTESIAN_POINT ( 'NONE',  ( -106.7978608999653147, -283.1908966454601000, -303.0515132556267872 ) ) ;
#87248 = CARTESIAN_POINT ( 'NONE',  ( -75.21544796164317859, -291.3244537175978621, -333.9649458097078991 ) ) ;
#87249 = CARTESIAN_POINT ( 'NONE',  ( -100.9822293102898811, -298.6313532685761061, -228.2351689511953623 ) ) ;
#87250 = CARTESIAN_POINT ( 'NONE',  ( -99.60779319749049421, -298.3515458704301295, -225.7411406964684204 ) ) ;
#87251 = CARTESIAN_POINT ( 'NONE',  ( 35.56725716330633702, -295.7699498231250459, -287.2792209464835764 ) ) ;
#87252 = CARTESIAN_POINT ( 'NONE',  ( -33.42512046158628181, -281.0025978067237702, -345.1047820624272049 ) ) ;
#87253 = CARTESIAN_POINT ( 'NONE',  ( -54.56716909451176889, -271.8498166174089761, -197.7310276724736866 ) ) ;
#87254 = CARTESIAN_POINT ( 'NONE',  ( -1.365439685353753152, -288.1213139819946605, -203.1885856401416675 ) ) ;
#87255 = CARTESIAN_POINT ( 'NONE',  ( 23.75956779660924667, -287.0324845419196436, -310.8915847506417549 ) ) ;
#87256 = CARTESIAN_POINT ( 'NONE',  ( -111.2738350685697242, -271.9824026107303325, -296.3714058503458659 ) ) ;
#87257 = ORIENTED_EDGE ( 'NONE', *, *, #30387, .F. ) ;
#87258 = CARTESIAN_POINT ( 'NONE',  ( -75.38617875257762080, -288.1239010411518962, -336.6274287234946314 ) ) ;
#87259 = CARTESIAN_POINT ( 'NONE',  ( 10.12578800294857473, -288.0433894995334754, -325.9160342701869695 ) ) ;
#87260 = VERTEX_POINT ( 'NONE', #25988 ) ;
#87261 = CARTESIAN_POINT ( 'NONE',  ( -75.96299195399845416, -286.6290074716606568, -204.0437260719109815 ) ) ;
#87262 = CARTESIAN_POINT ( 'NONE',  ( -61.79290780238834202, -277.7120218781069525, -339.2205844277083884 ) ) ;
#87263 = EDGE_CURVE ( 'NONE', #56563, #30942, #83807, .T. ) ;
#87264 = CARTESIAN_POINT ( 'NONE',  ( 6.331528368509314220, -291.5505444604578429, -207.3203246681044050 ) ) ;
#87265 = CARTESIAN_POINT ( 'NONE',  ( -110.1255247843209304, -284.8904710376473304, -295.1769930403011131 ) ) ;
#87266 = CARTESIAN_POINT ( 'NONE',  ( 8.117822137980358121, -282.1809137328357906, -209.0080948386793125 ) ) ;
#87267 = CARTESIAN_POINT ( 'NONE',  ( -16.14358460938926143, -283.1187657124955876, -344.4189854317366439 ) ) ;
#87268 = CARTESIAN_POINT ( 'NONE',  ( -22.19416355412491271, -280.5846993978017849, -198.8764832698838063 ) ) ;
#87269 = CARTESIAN_POINT ( 'NONE',  ( 197.8073114025361292, 285.2187192818669246, -111.8627074968393202 ) ) ;
#87270 = CARTESIAN_POINT ( 'NONE',  ( -92.29731272663953234, -279.8399450608151824, -321.2292675588906832 ) ) ;
#87271 = CARTESIAN_POINT ( 'NONE',  ( 43.96814812851462051, 12.86298614219447245, -331.2283216785375544 ) ) ;
#87272 = CARTESIAN_POINT ( 'NONE',  ( 137.3404605090900930, 179.3035625165208273, -238.6278596830658785 ) ) ;
#87273 = CARTESIAN_POINT ( 'NONE',  ( -67.11387441388059472, -272.8487596632852501, -203.5176167432603904 ) ) ;
#87274 = CARTESIAN_POINT ( 'NONE',  ( -81.84122124445936208, -295.1478143521354127, -333.1901907159369784 ) ) ;
#87275 = CARTESIAN_POINT ( 'NONE',  ( -46.67462993100657087, -155.6783835708859556, -361.6360932913781312 ) ) ;
#87276 = CARTESIAN_POINT ( 'NONE',  ( -105.1639677063337217, -271.6979495732385885, -234.8427339630296444 ) ) ;
#87277 = CARTESIAN_POINT ( 'NONE',  ( -23.26172385449286395, -296.7307687885535756, -343.3013181649975536 ) ) ;
#87278 = CARTESIAN_POINT ( 'NONE',  ( 35.45113976354100060, -289.0011581321349468, -280.5744514599383592 ) ) ;
#87279 = EDGE_LOOP ( 'NONE', ( #67578, #2974, #12853, #66853 ) ) ;
#87280 = CARTESIAN_POINT ( 'NONE',  ( -2.064903851216415287, -295.5378146961030552, -338.5400579722356156 ) ) ;
#87281 = CARTESIAN_POINT ( 'NONE',  ( 19.55917037978895934, -287.3968706103750037, -224.5124927996667168 ) ) ;
#87282 = CARTESIAN_POINT ( 'NONE',  ( -102.4493285647804015, -272.0048365429831847, -229.8334826128313466 ) ) ;
#87283 = CARTESIAN_POINT ( 'NONE',  ( 17.45358104984482850, -295.0967238557605583, -324.3036423813090323 ) ) ;
#87284 = CARTESIAN_POINT ( 'NONE',  ( 38.01158975573933674, -294.2389679511756526, -285.8984474558842521 ) ) ;
#87285 = EDGE_CURVE ( 'NONE', #93421, #44526, #49096, .T. ) ;
#87286 = CARTESIAN_POINT ( 'NONE',  ( -96.76259796540551861, -291.3123076784474961, -227.8709322712328742 ) ) ;
#87287 = EDGE_LOOP ( 'NONE', ( #70638, #4592, #27685, #89484 ) ) ;
#87288 = CARTESIAN_POINT ( 'NONE',  ( -104.3435756380947339, -274.9327569839260264, -235.3185650403014222 ) ) ;
#87289 = CARTESIAN_POINT ( 'NONE',  ( 2.226106963450188214, -273.3647149346820697, -204.7684555858694466 ) ) ;
#87290 = VERTEX_POINT ( 'NONE', #20317 ) ;
#87291 = CARTESIAN_POINT ( 'NONE',  ( -82.19789247943079147, -278.9658142037412745, -207.8515274319058221 ) ) ;
#87292 = CARTESIAN_POINT ( 'NONE',  ( 21.32980628138984258, -273.3290783019095898, -225.5731929472714228 ) ) ;
#87293 = CARTESIAN_POINT ( 'NONE',  ( -36.74731744702084768, -275.1394666428234927, -197.0419471297055054 ) ) ;
#87294 = CARTESIAN_POINT ( 'NONE',  ( 34.60240978813735069, -276.3133755742737776, -256.6697521988016319 ) ) ;
#87295 = CARTESIAN_POINT ( 'NONE',  ( -105.9381947329436571, -274.7369086618808183, -237.6732771360743470 ) ) ;
#87296 = CARTESIAN_POINT ( 'NONE',  ( 35.63934254584228967, -273.8122443555967038, -289.1274233249697545 ) ) ;
#87297 = CARTESIAN_POINT ( 'NONE',  ( -88.56736834861571595, -296.4450846996291489, -322.5841760501292015 ) ) ;
#87298 = CARTESIAN_POINT ( 'NONE',  ( 27.67018288197493092, -292.5941174617131537, -304.9493720598764526 ) ) ;
#87299 = CARTESIAN_POINT ( 'NONE',  ( -23.68628624284178130, -55.96374926131388605, 22.50000000000000000 ) ) ;
#87300 = CARTESIAN_POINT ( 'NONE',  ( -59.64117956998753556, -277.8258070894528942, -343.9971154274811624 ) ) ;
#87301 = CARTESIAN_POINT ( 'NONE',  ( -21.93609811957808731, -274.4217895716409430, -199.0051971964152813 ) ) ;
#87302 = CARTESIAN_POINT ( 'NONE',  ( -70.83513091964725561, -284.3043433101905748, -201.5753028104321629 ) ) ;
#87303 = CARTESIAN_POINT ( 'NONE',  ( -111.9580283749157701, -298.6686313515486404, -261.2819118079733585 ) ) ;
#87304 = DIRECTION ( 'NONE',  ( 0.000000000000000000, 0.000000000000000000, 1.000000000000000000 ) ) ;
#87305 = CARTESIAN_POINT ( 'NONE',  ( -19.76718857806303120, -285.4811144340898181, -199.3418370075646635 ) ) ;
#87306 = CARTESIAN_POINT ( 'NONE',  ( -103.0452667296297591, -277.2503966162068991, -236.1759650251008793 ) ) ;
#87307 = CARTESIAN_POINT ( 'NONE',  ( -101.1023658560115877, -276.6259270113345110, -307.2052025868670171 ) ) ;
#87308 = CARTESIAN_POINT ( 'NONE',  ( -111.6093470310158580, -286.4134885082714845, -281.1731576528224537 ) ) ;
#87309 = CARTESIAN_POINT ( 'NONE',  ( 35.23197956886108528, -276.6122843233832214, -259.3134808580199433 ) ) ;
#87310 = CYLINDRICAL_SURFACE ( 'NONE', #23165, 0.5000000000000004441 ) ;
#87311 = CARTESIAN_POINT ( 'NONE',  ( 29.25833729346708978, -273.4658279134842473, -233.2272293124265730 ) ) ;
#87312 = CARTESIAN_POINT ( 'NONE',  ( -93.60680092389856100, -281.2440130133224443, -220.5186976893350845 ) ) ;
#87313 = CARTESIAN_POINT ( 'NONE',  ( 157.4851178187871312, 15.00000000000000000, -7.000000000000000888 ) ) ;
#87314 = CARTESIAN_POINT ( 'NONE',  ( -15.84695292629675833, -288.2480831434349398, -197.8685868777397161 ) ) ;
#87315 = DIRECTION ( 'NONE',  ( -0.000000000000000000, -0.000000000000000000, -1.000000000000000000 ) ) ;
#87316 = CARTESIAN_POINT ( 'NONE',  ( 24.12504669051080342, -290.9676885813409513, -227.2984240255767361 ) ) ;
#87317 = CARTESIAN_POINT ( 'NONE',  ( 82.16537594709545544, -298.2571283212178059, -196.8956743398162246 ) ) ;
#87318 = CARTESIAN_POINT ( 'NONE',  ( -36.46212291700452823, -296.8583261757528362, -196.9642272592394363 ) ) ;
#87319 = CARTESIAN_POINT ( 'NONE',  ( -82.46132286242755072, -289.5685795514277743, -211.3462335369621314 ) ) ;
#87320 = CARTESIAN_POINT ( 'NONE',  ( -65.60899210820664962, -198.9355752380678553, -358.8784014864789924 ) ) ;
#87321 = CARTESIAN_POINT ( 'NONE',  ( -73.79734911780855100, -295.5678831107678661, -204.8173440081091883 ) ) ;
#87322 = CARTESIAN_POINT ( 'NONE',  ( -107.1054198436791154, -288.6324708229527687, -301.4060540099637819 ) ) ;
#87323 = CARTESIAN_POINT ( 'NONE',  ( -18.51206549728809136, -284.4058086775550009, -341.7715478998489402 ) ) ;
#87324 = CARTESIAN_POINT ( 'NONE',  ( -105.7568951107252104, -283.2219364173413396, -237.2954997853219936 ) ) ;
#87325 = CARTESIAN_POINT ( 'NONE',  ( -23.94052758841320383, -284.3028772952277450, -342.7198319716271726 ) ) ;
#87326 = CARTESIAN_POINT ( 'NONE',  ( -65.36811900831199296, -284.2309443499473218, -337.9552278606435607 ) ) ;
#87327 = CARTESIAN_POINT ( 'NONE',  ( -48.59786250117770834, -291.1745405237812179, -344.9236762516080148 ) ) ;
#87328 = CARTESIAN_POINT ( 'NONE',  ( 23.61349818541550150, -275.2575915701593772, -223.3268135047993326 ) ) ;
#87329 = ORIENTED_EDGE ( 'NONE', *, *, #49529, .T. ) ;
#87330 = CARTESIAN_POINT ( 'NONE',  ( -41.70236007198370487, -287.1865028781521119, -345.8081623466974861 ) ) ;
#87331 = CARTESIAN_POINT ( 'NONE',  ( 38.72760953650423232, -275.4018172793528834, -258.3404622175017948 ) ) ;
#87332 = CARTESIAN_POINT ( 'NONE',  ( -6.053003555348501763, -296.6187749441894539, -338.1317921208016060 ) ) ;
#87333 = CARTESIAN_POINT ( 'NONE',  ( 82.64890176555634582, -299.5541904835127980, -189.2068768330456123 ) ) ;
#87334 = CARTESIAN_POINT ( 'NONE',  ( 208.9735924857420741, 36.55662354001872671, 13.48907645363297547 ) ) ;
#87335 = CARTESIAN_POINT ( 'NONE',  ( -56.46323529527972340, -281.9886214271139124, -341.3231526880317688 ) ) ;
#87336 = CARTESIAN_POINT ( 'NONE',  ( -68.28451945632860998, -275.4574352414505825, -338.8775205843881508 ) ) ;
#87337 = CARTESIAN_POINT ( 'NONE',  ( 74.93979048022610812, -297.8354839955923126, -194.1910459442052286 ) ) ;
#87338 = CARTESIAN_POINT ( 'NONE',  ( 33.99090781893561086, -275.1120745045000149, -286.4039950356229838 ) ) ;
#87339 = CARTESIAN_POINT ( 'NONE',  ( 25.42838062180426917, -294.5439060555598871, -231.6556734052198010 ) ) ;
#87340 = CARTESIAN_POINT ( 'NONE',  ( 29.71028046796762823, -294.8883569293827236, -299.8134582218693822 ) ) ;
#87341 = CARTESIAN_POINT ( 'NONE',  ( -94.92436863411488446, -286.9610598456816888, -223.8414499721200457 ) ) ;
#87342 = CARTESIAN_POINT ( 'NONE',  ( 15.02106687614145741, -294.1983839140704617, -214.6400628544085976 ) ) ;
#87343 = CARTESIAN_POINT ( 'NONE',  ( 33.99773281531482638, -295.2197441220977225, -298.0013708590839769 ) ) ;
#87344 = CARTESIAN_POINT ( 'NONE',  ( -108.1744287244692515, -296.6190727759282595, -252.6542251949486797 ) ) ;
#87345 = CARTESIAN_POINT ( 'NONE',  ( -112.3040877319867690, -292.5051888308561843, -274.0315578631796143 ) ) ;
#87346 = CARTESIAN_POINT ( 'NONE',  ( -5.453581932983436076, -282.8107860758286165, -340.4478351442622852 ) ) ;
#87347 = CARTESIAN_POINT ( 'NONE',  ( -95.96500942038261428, -271.3468808658288935, -222.3449104624316135 ) ) ;
#87348 = CARTESIAN_POINT ( 'NONE',  ( 24.70452958863816662, -286.7797811988014587, -224.7621554673708317 ) ) ;
#87349 = CARTESIAN_POINT ( 'NONE',  ( -86.16238213979377747, -279.7125912528277922, -326.8953769566107894 ) ) ;
#87350 = EDGE_CURVE ( 'NONE', #83883, #5562, #91446, .T. ) ;
#87351 = CARTESIAN_POINT ( 'NONE',  ( -65.22995255942416293, -284.4744307031965604, -202.4146387939862279 ) ) ;
#87352 = CARTESIAN_POINT ( 'NONE',  ( 24.19572886757650565, -286.1347439309681704, -313.3238464601024020 ) ) ;
#87353 = CARTESIAN_POINT ( 'NONE',  ( -98.41786475236470721, -277.2971497485578425, -225.5061226893401169 ) ) ;
#87354 = CARTESIAN_POINT ( 'NONE',  ( -104.9628119525177112, -256.0684274861638983, -326.9234398911233939 ) ) ;
#87355 = CARTESIAN_POINT ( 'NONE',  ( -102.2902356206279819, -284.5143087649622657, -236.8995552749194928 ) ) ;
#87356 = CARTESIAN_POINT ( 'NONE',  ( 21.31590875015975683, -283.4240054882389472, -319.6286898785173776 ) ) ;
#87357 = CARTESIAN_POINT ( 'NONE',  ( -102.1092041658163225, -289.0680171929629410, -311.6656420689378706 ) ) ;
#87358 = CARTESIAN_POINT ( 'NONE',  ( -68.66767518564732597, -279.0571418358229607, -339.8384812578836431 ) ) ;
#87359 = CARTESIAN_POINT ( 'NONE',  ( -6.756365149318233065, -277.9741672813127593, -340.5025656116278014 ) ) ;
#87360 = CARTESIAN_POINT ( 'NONE',  ( -107.6177356582538209, -278.6471574995300671, -250.5593167686149343 ) ) ;
#87361 = CARTESIAN_POINT ( 'NONE',  ( -40.87753351654002643, -275.9874786500002415, -195.7492853401443256 ) ) ;
#87362 = CARTESIAN_POINT ( 'NONE',  ( 15.43816516568050723, -292.7733411504802916, -214.2228942956865581 ) ) ;
#87363 = CARTESIAN_POINT ( 'NONE',  ( -75.57965824074560146, -287.5850235820369676, -334.4831221231992231 ) ) ;
#87364 = CARTESIAN_POINT ( 'NONE',  ( -6.232385340799044826, -294.0541992570694561, -200.7865678907699305 ) ) ;
#87365 = CARTESIAN_POINT ( 'NONE',  ( 33.04311923035042753, -292.7430299370837474, -290.9050678882197758 ) ) ;
#87366 = CARTESIAN_POINT ( 'NONE',  ( -0.7510309649830725354, -294.2188064752875789, -333.6106804635929848 ) ) ;
#87367 = CARTESIAN_POINT ( 'NONE',  ( -50.52678245010447711, -292.9672198073618006, -194.8121529789007980 ) ) ;
#87368 = CARTESIAN_POINT ( 'NONE',  ( 35.80492689081132340, -282.2160274776437632, -271.3068100294576084 ) ) ;
#87369 = EDGE_CURVE ( 'NONE', #32191, #86290, #13224, .T. ) ;
#87370 = ADVANCED_FACE ( 'NONE', ( #78543 ), #61204, .F. ) ;
#87371 = CARTESIAN_POINT ( 'NONE',  ( -40.41404922764577634, -296.9348465727555322, -193.6798768933045949 ) ) ;
#87372 = CARTESIAN_POINT ( 'NONE',  ( -70.58748147724664079, -290.1304078894370946, -339.7155494786653662 ) ) ;
#87373 = CARTESIAN_POINT ( 'NONE',  ( -30.35280132281144105, -281.1042205922930179, -345.8028887301368854 ) ) ;
#87374 = CARTESIAN_POINT ( 'NONE',  ( 24.12788664585239573, -288.5026344928243134, -316.6993764031540195 ) ) ;
#87376 = CARTESIAN_POINT ( 'NONE',  ( -42.67990905482616881, -286.3162642173693371, -197.5227308216707911 ) ) ;
#87375 = VECTOR ( 'NONE', #48341, 1000.000000000000000 ) ;
#87377 = DIRECTION ( 'NONE',  ( -1.000000000000000000, -0.000000000000000000, -0.000000000000000000 ) ) ;
#87378 = CARTESIAN_POINT ( 'NONE',  ( 159.3374055019249909, 220.0097216543477430, -203.8079738436954642 ) ) ;
#87379 = CARTESIAN_POINT ( 'NONE',  ( 198.4972914423243822, 285.9627626194107961, -96.27642562114702685 ) ) ;
#87380 = CARTESIAN_POINT ( 'NONE',  ( -54.52080894794085708, -279.0230250053349437, -199.1928460675015060 ) ) ;
#87381 = CARTESIAN_POINT ( 'NONE',  ( -95.85018299386948115, -278.0905842776803638, -226.1703470308495696 ) ) ;
#87382 = CARTESIAN_POINT ( 'NONE',  ( -49.71165681030664985, -273.5653706364552704, -194.3288540074505590 ) ) ;
#87383 = CARTESIAN_POINT ( 'NONE',  ( 27.10728642065183891, -24.65249435300752978, -342.5275202601461046 ) ) ;
#87384 = CARTESIAN_POINT ( 'NONE',  ( -40.96217823716339979, -278.5821964103578239, -194.0230704717859851 ) ) ;
#87385 = CARTESIAN_POINT ( 'NONE',  ( -13.01666320200853022, -280.7547668883113943, -340.9860258191369553 ) ) ;
#87386 = CARTESIAN_POINT ( 'NONE',  ( -53.05748494590894637, -297.0109501695598624, -344.7586558807576580 ) ) ;
#87387 = CARTESIAN_POINT ( 'NONE',  ( -28.10477759675800513, -292.6647679518334826, -197.8350368730701518 ) ) ;
#87388 = CARTESIAN_POINT ( 'NONE',  ( -42.71658813141468869, -287.8060606753376192, -343.7084080248773716 ) ) ;
#87389 = CARTESIAN_POINT ( 'NONE',  ( -96.86245927666115563, -273.8583029697116444, -221.6518418534377304 ) ) ;
#87390 = CARTESIAN_POINT ( 'NONE',  ( -101.2155899136548527, -297.2018741531614978, -235.0181383664189525 ) ) ;
#87391 = ORIENTED_EDGE ( 'NONE', *, *, #76250, .T. ) ;
#87392 = CARTESIAN_POINT ( 'NONE',  ( 195.2846006655043709, -165.1985023605670335, 21.50000000000000000 ) ) ;
#87393 = CARTESIAN_POINT ( 'NONE',  ( -42.35931087744771872, -281.9094864688591997, -194.9678969269052402 ) ) ;
#87394 = CARTESIAN_POINT ( 'NONE',  ( -19.47246110956689336, -281.3669857476694460, -199.2106742646069222 ) ) ;
#87395 = CARTESIAN_POINT ( 'NONE',  ( -112.7576276996449565, -280.1892171748334590, -280.0725231107722948 ) ) ;
#87396 = CARTESIAN_POINT ( 'NONE',  ( 35.80031659018471402, -280.6594826537344147, -274.0562279770529699 ) ) ;
#87397 = CARTESIAN_POINT ( 'NONE',  ( -36.71087157183738015, -272.5400945535506594, -196.6579488219028349 ) ) ;
#87398 = CARTESIAN_POINT ( 'NONE',  ( 209.5654368701818271, 27.96016292911928502, 12.08763307006249832 ) ) ;
#87399 = LINE ( 'NONE', #59955, #54717 ) ;
#87400 = CARTESIAN_POINT ( 'NONE',  ( 37.47533411851565432, -276.1348917514042114, -252.7947693400713263 ) ) ;
#87401 = CARTESIAN_POINT ( 'NONE',  ( 31.85812037710185862, -277.1731482225920900, -241.3067646063770724 ) ) ;
#87402 = CARTESIAN_POINT ( 'NONE',  ( -94.77994920763046593, -276.4397225151909083, -320.7541119048909763 ) ) ;
#87403 = EDGE_LOOP ( 'NONE', ( #60728, #57463, #70538, #75289 ) ) ;
#87404 = CARTESIAN_POINT ( 'NONE',  ( 200.7568414405312751, 39.78480925505072463, 8.999999999999998224 ) ) ;
#87405 = CARTESIAN_POINT ( 'NONE',  ( 0.07405726863351481948, -284.5366465922003272, -335.7860257773597255 ) ) ;
#87406 = CARTESIAN_POINT ( 'NONE',  ( -98.42874208005309811, -290.3075701170967591, -230.0077797776543491 ) ) ;
#87407 = CARTESIAN_POINT ( 'NONE',  ( 28.61539165901615789, -286.3833291750647732, -230.7239276617104906 ) ) ;
#87408 = CARTESIAN_POINT ( 'NONE',  ( -78.96475283924839061, -281.8617958153433847, -331.5615713691366864 ) ) ;
#87410 = CARTESIAN_POINT ( 'NONE',  ( -3.926670217352778991, -284.5762952634519820, -203.8423238163472035 ) ) ;
#87409 = CARTESIAN_POINT ( 'NONE',  ( -74.10678701983255223, -282.1252905895308913, -334.1663762892271166 ) ) ;
#87411 = CARTESIAN_POINT ( 'NONE',  ( 11.55901319616538814, -281.9539609382625258, -215.6267527243214488 ) ) ;
#87412 = CARTESIAN_POINT ( 'NONE',  ( 23.71396947211090733, -272.9594273849806427, -226.7822114662816944 ) ) ;
#87413 = CARTESIAN_POINT ( 'NONE',  ( -95.67122081008454870, -282.2847108426046816, -319.4130120510674260 ) ) ;
#87414 = CARTESIAN_POINT ( 'NONE',  ( -104.1639009116272234, -298.1007224043335100, -304.5311948212975608 ) ) ;
#87415 = CARTESIAN_POINT ( 'NONE',  ( -110.1365219269036686, -279.3820639169513811, -278.8288874517366480 ) ) ;
#87416 = CARTESIAN_POINT ( 'NONE',  ( -90.62187097233132249, -287.2993055969275247, -217.3398786502342261 ) ) ;
#87417 = CARTESIAN_POINT ( 'NONE',  ( 210.6911063078042901, 0.9999999999999991118, -7.166232077703399206 ) ) ;
#87418 = CARTESIAN_POINT ( 'NONE',  ( 38.06686676313274376, -295.5430086314377718, -275.9086037637108006 ) ) ;
#87419 = CARTESIAN_POINT ( 'NONE',  ( -70.14865211115889565, -275.4841491608034403, -337.8194206447396937 ) ) ;
#87420 = CARTESIAN_POINT ( 'NONE',  ( 16.56536935926178344, -287.5066981879070340, -325.1907959610214789 ) ) ;
#87421 = CARTESIAN_POINT ( 'NONE',  ( 36.44089357137963958, -291.9935428719738297, -273.5435715600183357 ) ) ;
#87422 = CARTESIAN_POINT ( 'NONE',  ( -64.53106175149169133, -276.0993533517874994, -338.6938779878001924 ) ) ;
#87423 = CARTESIAN_POINT ( 'NONE',  ( -107.8730478718130428, -294.9958608276012910, -247.0424411260378861 ) ) ;
#87424 = CARTESIAN_POINT ( 'NONE',  ( -64.26777787912008932, -293.0085004557493562, -201.9645277027552481 ) ) ;
#87425 = CARTESIAN_POINT ( 'NONE',  ( -110.4683760289727132, -281.2662352645559167, -253.7030783399848985 ) ) ;
#87426 = DIRECTION ( 'NONE',  ( -0.000000000000000000, -0.000000000000000000, -1.000000000000000000 ) ) ;
#87427 = CARTESIAN_POINT ( 'NONE',  ( -50.36837877540950359, -293.6953018904815735, -345.6011029765929266 ) ) ;
#87428 = CARTESIAN_POINT ( 'NONE',  ( 31.71605933782575804, -288.8070002019125582, -244.1887855995624648 ) ) ;
#87429 = CARTESIAN_POINT ( 'NONE',  ( -98.37708703366595842, -289.4020300999017081, -225.0772527550459188 ) ) ;
#87430 = EDGE_CURVE ( 'NONE', #81416, #92001, #49936, .T. ) ;
#87431 = CARTESIAN_POINT ( 'NONE',  ( -75.00198021850144414, -290.9896388054556837, -333.5983716431630342 ) ) ;
#87432 = FACE_OUTER_BOUND ( 'NONE', #42339, .T. ) ;
#87433 = CARTESIAN_POINT ( 'NONE',  ( -109.3360016495561240, -291.1836609239832114, -283.3773492239082543 ) ) ;
#87434 = CYLINDRICAL_SURFACE ( 'NONE', #56479, 3.000000000000000000 ) ;
#87435 = CIRCLE ( 'NONE', #34545, 2.000000000000010658 ) ;
#87436 = CARTESIAN_POINT ( 'NONE',  ( -69.17820966355287737, -290.6667542940334101, -340.0493156626847053 ) ) ;
#87437 = CARTESIAN_POINT ( 'NONE',  ( -70.48788889747339681, -277.6374449138581326, -202.6873640045662057 ) ) ;
#87438 = CARTESIAN_POINT ( 'NONE',  ( -112.6977213941364937, -279.0829151822152880, -254.5744817359279466 ) ) ;
#87439 = CARTESIAN_POINT ( 'NONE',  ( 36.96571459157146933, -280.9664776829865218, -250.2075776547380599 ) ) ;
#87440 = CARTESIAN_POINT ( 'NONE',  ( 25.16257708171830743, -286.1121439427332120, -311.8359330059347485 ) ) ;
#87441 = CARTESIAN_POINT ( 'NONE',  ( 207.4724402404594343, 29.73442829110639352, 14.90057469441957672 ) ) ;
#87442 = CARTESIAN_POINT ( 'NONE',  ( -94.88319868027859627, -277.3446380700085001, -223.4586507975719485 ) ) ;
#87443 = CARTESIAN_POINT ( 'NONE',  ( -92.93426618295407593, -281.8497423685461172, -320.7236659856005758 ) ) ;
#87444 = DIRECTION ( 'NONE',  ( 0.9531768234071978929, -0.3024135303179465439, 0.000000000000000000 ) ) ;
#87445 = CARTESIAN_POINT ( 'NONE',  ( -84.12643378733078237, -277.9024122162133494, -210.0124553379182544 ) ) ;
#87446 = CARTESIAN_POINT ( 'NONE',  ( -106.7318251203581099, -283.0524995122739256, -303.0184764554630306 ) ) ;
#87447 = CARTESIAN_POINT ( 'NONE',  ( -110.3506725206230072, -273.4267192413486782, -264.9115845521561710 ) ) ;
#87448 = CARTESIAN_POINT ( 'NONE',  ( -33.38316814304199198, -299.4159035733547398, -193.8534013558464153 ) ) ;
#87449 = CARTESIAN_POINT ( 'NONE',  ( -11.25044979024342773, -276.3692630959180860, -338.5618081739960417 ) ) ;
#87450 = CARTESIAN_POINT ( 'NONE',  ( -5.903989809654467180, -296.6390399639862494, -338.4542235263243697 ) ) ;
#87451 = CARTESIAN_POINT ( 'NONE',  ( -34.66469536096866477, -289.1860616094461420, -347.3145691722260722 ) ) ;
#87452 = CARTESIAN_POINT ( 'NONE',  ( 31.07788996442805285, -280.0518135727807589, -302.5478941078378057 ) ) ;
#87453 = CARTESIAN_POINT ( 'NONE',  ( -0.8019872655570401410, -292.3571057214098232, -202.5831762283037847 ) ) ;
#87454 = CARTESIAN_POINT ( 'NONE',  ( -82.70135900316022060, -288.7486863419639462, -327.8581595943308002 ) ) ;
#87455 = CARTESIAN_POINT ( 'NONE',  ( 34.44767913258165493, -291.8337937117538559, -292.2459588730054065 ) ) ;
#87456 = EDGE_LOOP ( 'NONE', ( #1778, #5576, #45574 ) ) ;
#87457 = DIRECTION ( 'NONE',  ( 1.000000000000000000, 0.000000000000000000, -0.000000000000000000 ) ) ;
#87458 = CARTESIAN_POINT ( 'NONE',  ( -90.64194189747172459, -289.3406535356612039, -320.4057245494398671 ) ) ;
#87459 = DIRECTION ( 'NONE',  ( -0.000000000000000000, -1.000000000000000000, -0.000000000000000000 ) ) ;
#87460 = CARTESIAN_POINT ( 'NONE',  ( 33.63727689354109174, -288.1191482891186979, -240.9852545110913979 ) ) ;
#87461 = CARTESIAN_POINT ( 'NONE',  ( -105.5937364680635966, -287.2662352645559167, -254.8156830097664738 ) ) ;
#87462 = CARTESIAN_POINT ( 'NONE',  ( -13.86543179726718833, -293.8135163188520096, -343.4479501600656022 ) ) ;
#87463 = CARTESIAN_POINT ( 'NONE',  ( -52.80148409090261197, -284.5613071630124296, -345.3438468166185658 ) ) ;
#87464 = CARTESIAN_POINT ( 'NONE',  ( -107.3543529578805078, -284.6610613146342530, -249.5163129704913842 ) ) ;
#87465 = CARTESIAN_POINT ( 'NONE',  ( 19.36877850266219880, -276.2092558774691042, -223.6153685185697100 ) ) ;
#87466 = CARTESIAN_POINT ( 'NONE',  ( -28.73071693741689003, -292.9626700724140846, -344.5597412658509597 ) ) ;
#87467 = CARTESIAN_POINT ( 'NONE',  ( -35.36433102320749100, -272.8724076525500664, -196.9781112787953248 ) ) ;
#87468 = VERTEX_POINT ( 'NONE', #55283 ) ;
#87469 = CARTESIAN_POINT ( 'NONE',  ( 5.045406874201050940, -57.93311274753654061, -355.0152878038887820 ) ) ;
#87470 = CARTESIAN_POINT ( 'NONE',  ( -39.11160818181522103, -294.7405154851434759, -347.3196244461289552 ) ) ;
#87471 = CARTESIAN_POINT ( 'NONE',  ( -7.703651408092746067, -288.3638230883290134, -202.0756856551316787 ) ) ;
#87472 = CARTESIAN_POINT ( 'NONE',  ( -108.0845627511785807, -297.2520945643541950, -300.1116742640614348 ) ) ;
#87473 = CARTESIAN_POINT ( 'NONE',  ( -41.33678258224720992, -286.6519756750923307, -197.3559177859472982 ) ) ;
#87474 = CARTESIAN_POINT ( 'NONE',  ( -101.6874254727223246, -278.1634744556908458, -228.4027054707015623 ) ) ;
#87475 = CARTESIAN_POINT ( 'NONE',  ( 29.49019281657561109, -294.6993810122234549, -308.5056728672675490 ) ) ;
#87476 = CARTESIAN_POINT ( 'NONE',  ( 11.59960011635695309, -286.5208722300635031, -328.1975650402567339 ) ) ;
#87477 = CARTESIAN_POINT ( 'NONE',  ( 37.44047841697738477, -294.1145115046701903, -288.6747107508439854 ) ) ;
#87478 = CARTESIAN_POINT ( 'NONE',  ( -47.00146186372176516, -292.2593546115554659, -197.9817252665747276 ) ) ;
#87479 = FACE_OUTER_BOUND ( 'NONE', #40850, .T. ) ;
#87480 = CARTESIAN_POINT ( 'NONE',  ( 169.8384340989974532, 250.0000000000000568, -24.41176470588234437 ) ) ;
#87481 = CARTESIAN_POINT ( 'NONE',  ( 103.6749136202614778, 114.2737147221711211, -279.7089131146261138 ) ) ;
#87482 = CARTESIAN_POINT ( 'NONE',  ( 30.79393473868758591, -288.6261657213288458, -236.0064529106052760 ) ) ;
#87483 = CARTESIAN_POINT ( 'NONE',  ( -115.3430155898818299, -281.8380690714489560, -288.1317622949166548 ) ) ;
#87484 = ORIENTED_EDGE ( 'NONE', *, *, #133, .F. ) ;
#87485 = CARTESIAN_POINT ( 'NONE',  ( -113.6149008061959194, -278.0283247093928480, -260.1731331670051190 ) ) ;
#87486 = CARTESIAN_POINT ( 'NONE',  ( 34.48735314361493920, -283.2814240054922834, -249.3702739330317968 ) ) ;
#87487 = CARTESIAN_POINT ( 'NONE',  ( 7.635230013240764890, -59.72540331351240894, -353.5597951569748147 ) ) ;
#87488 = CARTESIAN_POINT ( 'NONE',  ( -96.72602834267753735, -282.4768190808816257, -318.4660678217218788 ) ) ;
#87489 = CARTESIAN_POINT ( 'NONE',  ( -26.28468064830018847, -286.9903124395260647, -344.0274140495475308 ) ) ;
#87490 = CARTESIAN_POINT ( 'NONE',  ( -36.96997225697152345, -275.9172012707707040, -194.5843838876608913 ) ) ;
#87491 = CARTESIAN_POINT ( 'NONE',  ( -77.55107103287573977, -297.9890958341909482, -209.2987225683046120 ) ) ;
#87492 = EDGE_CURVE ( 'NONE', #90289, #15111, #15843, .T. ) ;
#87493 = CARTESIAN_POINT ( 'NONE',  ( -18.10745509621242277, -293.4837920332224144, -341.2926856711375194 ) ) ;
#87494 = CARTESIAN_POINT ( 'NONE',  ( -95.83367969966693067, -279.8779490945777866, -220.4209434580480718 ) ) ;
#87496 = CARTESIAN_POINT ( 'NONE',  ( -74.55053736222001248, -278.8919499869463721, -207.3792141205761368 ) ) ;
#87495 = CARTESIAN_POINT ( 'NONE',  ( -19.01694518221568941, -276.8096177405436720, -341.0237202285427429 ) ) ;
#87497 = CARTESIAN_POINT ( 'NONE',  ( 30.96870528085740304, -276.1810438587848466, -235.5016713180875740 ) ) ;
#87498 = CARTESIAN_POINT ( 'NONE',  ( -77.66412260773562082, -276.4999882806125697, -335.6577557231277638 ) ) ;
#87499 = DIRECTION ( 'NONE',  ( 0.000000000000000000, 1.000000000000000000, 0.000000000000000000 ) ) ;
#87500 = CARTESIAN_POINT ( 'NONE',  ( -74.76067976648381830, -275.5496681823021845, -335.4179607720236618 ) ) ;
#87501 = EDGE_CURVE ( 'NONE', #6151, #30132, #34897, .T. ) ;
#87502 = CARTESIAN_POINT ( 'NONE',  ( -105.4243873815916430, -297.5259267141387909, -305.1670114128638147 ) ) ;
#87503 = LINE ( 'NONE', #43956, #74555 ) ;
#87504 = AXIS2_PLACEMENT_3D ( 'NONE', #73602, #82555, #31444 ) ;
#87505 = FACE_OUTER_BOUND ( 'NONE', #65302, .T. ) ;
#87506 = CARTESIAN_POINT ( 'NONE',  ( -68.92049531987663613, -286.7065460484066648, -204.1883253691638913 ) ) ;
#87507 = CARTESIAN_POINT ( 'NONE',  ( -113.3144487282843755, -286.3526147049877295, -267.1794917998780647 ) ) ;
#87508 = CARTESIAN_POINT ( 'NONE',  ( 0.2281604315425367902, -285.9149977900521549, -207.5932631964456050 ) ) ;
#87509 = CARTESIAN_POINT ( 'NONE',  ( -110.0779924788421198, -276.7881326928743420, -282.9208106700475582 ) ) ;
#87510 = CARTESIAN_POINT ( 'NONE',  ( -97.59095512839444098, -287.0091669695266319, -226.9701629338598252 ) ) ;
#87511 = CARTESIAN_POINT ( 'NONE',  ( -74.84208895854072807, -278.0233813588476437, -206.8640880892528742 ) ) ;
#87512 = CARTESIAN_POINT ( 'NONE',  ( -76.50940247791791649, -278.6689211493159064, -332.3894928956623289 ) ) ;
#87513 = CARTESIAN_POINT ( 'NONE',  ( 200.2349812190172713, 66.43136063442170780, -7.741079165001072404 ) ) ;
#87514 = CARTESIAN_POINT ( 'NONE',  ( 33.30329851965409915, -276.2903645851201873, -288.9963697350226539 ) ) ;
#87515 =( BOUNDED_CURVE ( )  B_SPLINE_CURVE ( 3, ( #20415, #34, #27509, #72472 ),
 .UNSPECIFIED., .F., .F. ) 
 B_SPLINE_CURVE_WITH_KNOTS ( ( 4, 4 ),
 ( 1.570796326794896558, 3.141592653589793116 ),
 .UNSPECIFIED. ) 
 CURVE ( )  GEOMETRIC_REPRESENTATION_ITEM ( )  RATIONAL_B_SPLINE_CURVE ( ( 1.000000000000000000, 0.8047378541243649375, 0.8047378541243649375, 1.000000000000000000 ) ) 
 REPRESENTATION_ITEM ( '' )  );
#87516 = CARTESIAN_POINT ( 'NONE',  ( 38.51009246984892798, -282.5098452898087658, -282.7179164840283079 ) ) ;
#87517 = CARTESIAN_POINT ( 'NONE',  ( -44.40731385203950765, -283.6314734543273630, -347.0277734786789665 ) ) ;
#87518 = VERTEX_POINT ( 'NONE', #77516 ) ;
#87519 = VERTEX_POINT ( 'NONE', #20226 ) ;
#87520 = CARTESIAN_POINT ( 'NONE',  ( 196.0490226090805379, 41.97839894083266188, 13.84150264294241239 ) ) ;
#87521 = CARTESIAN_POINT ( 'NONE',  ( 13.78789841822058904, -290.2052667678747184, -326.3434982694111000 ) ) ;
#87522 =( BOUNDED_CURVE ( )  B_SPLINE_CURVE ( 3, ( #72485, #56901, #7601, #516 ),
 .UNSPECIFIED., .F., .F. ) 
 B_SPLINE_CURVE_WITH_KNOTS ( ( 4, 4 ),
 ( 5.134959379131573520, 6.283185307179586232 ),
 .UNSPECIFIED. ) 
 CURVE ( )  GEOMETRIC_REPRESENTATION_ITEM ( )  RATIONAL_B_SPLINE_CURVE ( ( 1.000000000000000000, 0.8931162488198156613, 0.8931162488198156613, 1.000000000000000000 ) ) 
 REPRESENTATION_ITEM ( '' )  );
#87523 = CARTESIAN_POINT ( 'NONE',  ( -96.02365161109059954, -288.5719215777939439, -319.4704125664965204 ) ) ;
#87524 = CARTESIAN_POINT ( 'NONE',  ( -65.62572121608263842, -296.8696999052388037, -202.8880427721977924 ) ) ;
#87525 = CARTESIAN_POINT ( 'NONE',  ( -4.639949800427709548, -291.8203395988667808, -200.7629261049724505 ) ) ;
#87526 = CARTESIAN_POINT ( 'NONE',  ( 24.81282923063587020, -286.5743261034620559, -309.9530645397802004 ) ) ;
#87527 = CARTESIAN_POINT ( 'NONE',  ( 31.34076396985507884, -288.4120111772829205, -244.3362754279621640 ) ) ;
#87528 = CARTESIAN_POINT ( 'NONE',  ( -54.42813229853333468, -297.7662352645559167, -345.3683826091709648 ) ) ;
#87529 = CARTESIAN_POINT ( 'NONE',  ( -71.10632659307661640, -287.4966203649944987, -337.5174909502709966 ) ) ;
#87530 = CARTESIAN_POINT ( 'NONE',  ( -80.75601236308186515, -284.5985298707938114, -329.4039128301236588 ) ) ;
#87531 = CARTESIAN_POINT ( 'NONE',  ( -76.24279594863611464, -293.5340424947768270, -205.9836385051075922 ) ) ;
#87532 = CARTESIAN_POINT ( 'NONE',  ( 175.2296996224750103, 20.99999999999998934, -25.00000000000000355 ) ) ;
#87533 = CARTESIAN_POINT ( 'NONE',  ( 209.7513585654922679, 305.7026273589066818, -40.00000000000000711 ) ) ;
#87534 = CARTESIAN_POINT ( 'NONE',  ( -34.14802657023491150, -300.0119829776966185, -194.8000747783010524 ) ) ;
#87535 = PRODUCT_DEFINITION_SHAPE ( 'NONE', 'NONE',  #93721 ) ;
#87536 = CARTESIAN_POINT ( 'NONE',  ( 19.47097385672049796, -281.4003305579699372, -316.4777359957691942 ) ) ;
#87537 = CARTESIAN_POINT ( 'NONE',  ( -99.19585473824058397, -281.9762871659203824, -312.8670508382804201 ) ) ;
#87538 = CARTESIAN_POINT ( 'NONE',  ( 37.91037156935676933, -292.9439976829007719, -285.8944539526964945 ) ) ;
#87539 = CARTESIAN_POINT ( 'NONE',  ( -108.1596390510478187, -271.0750294385023835, -248.6730993082246925 ) ) ;
#87540 = CARTESIAN_POINT ( 'NONE',  ( 36.12435790985168182, -273.7912828932889511, -282.6741484721150641 ) ) ;
#87541 = CARTESIAN_POINT ( 'NONE',  ( -60.68832360411418847, -299.0581455123403316, -200.6209957712173377 ) ) ;
#87542 = DIRECTION ( 'NONE',  ( -1.000000000000000000, -0.000000000000000000, 0.000000000000000000 ) ) ;
#87543 = CARTESIAN_POINT ( 'NONE',  ( -81.30394289193519342, -293.8802244051389607, -332.4035795776117084 ) ) ;
#87544 = CARTESIAN_POINT ( 'NONE',  ( -2.851656814702925313, -296.0120871980672064, -335.3673625330421828 ) ) ;
#87545 = DIRECTION ( 'NONE',  ( 0.000000000000000000, 1.000000000000000000, 0.000000000000000000 ) ) ;
#87546 = CARTESIAN_POINT ( 'NONE',  ( -38.33425059091678833, -295.8677434835836380, -343.5158619919911871 ) ) ;
#87547 = CARTESIAN_POINT ( 'NONE',  ( 152.4536156746142410, 130.6065089285656313, 11.50000000000000000 ) ) ;
#87549 = CARTESIAN_POINT ( 'NONE',  ( -90.04586497955105528, -297.2817562745242981, -219.7786690494482684 ) ) ;
#87548 = CARTESIAN_POINT ( 'NONE',  ( -109.9143609314994023, -282.3124927603950027, -290.6494325634084817 ) ) ;
#87550 = CARTESIAN_POINT ( 'NONE',  ( -110.6855457350264089, -284.2568996930114054, -293.8498614111003917 ) ) ;
#87551 = CARTESIAN_POINT ( 'NONE',  ( 35.80408693258499397, -283.7139639184255202, -289.3086253683503628 ) ) ;
#87552 = CARTESIAN_POINT ( 'NONE',  ( 39.58297291944533214, -287.2697232695270486, -274.4260518540313001 ) ) ;
#87553 = CARTESIAN_POINT ( 'NONE',  ( -33.38669500999364459, -290.1018730315056473, -195.6195603438067110 ) ) ;
#87554 = EDGE_CURVE ( 'NONE', #5855, #2870, #53279, .T. ) ;
#87555 = CARTESIAN_POINT ( 'NONE',  ( -22.58714906154741442, -279.4334352304951494, -194.8983413833674376 ) ) ;
#87556 = EDGE_CURVE ( 'NONE', #90952, #57748, #36356, .T. ) ;
#87557 = CARTESIAN_POINT ( 'NONE',  ( 39.58706461736020543, -279.0523547857347353, -270.3937649182068981 ) ) ;
#87558 = CARTESIAN_POINT ( 'NONE',  ( -48.18343439339133027, -253.5923708015767772, -491.0188676228033273 ) ) ;
#87559 = CARTESIAN_POINT ( 'NONE',  ( 29.78200958327513703, -286.7459899928995242, -300.1778632230015660 ) ) ;
#87560 = CARTESIAN_POINT ( 'NONE',  ( -59.94932255653006337, -288.2587668073750820, -343.6440485817265653 ) ) ;
#87561 = DIRECTION ( 'NONE',  ( 1.000000000000000000, -0.000000000000000000, 0.000000000000000000 ) ) ;
#87562 = CARTESIAN_POINT ( 'NONE',  ( -110.8947425426318318, -298.0657688213805159, -276.9915744421043087 ) ) ;
#87563 = CARTESIAN_POINT ( 'NONE',  ( -97.45403635994424008, -279.3419342140627464, -317.5322249034054494 ) ) ;
#87565 = CARTESIAN_POINT ( 'NONE',  ( 20.53528754459697225, -280.5922171555554314, -225.8172970462405829 ) ) ;
#87564 = CARTESIAN_POINT ( 'NONE',  ( -70.11579738028902398, -293.5018121659139752, -338.2300571174537254 ) ) ;
#87566 = CARTESIAN_POINT ( 'NONE',  ( 24.03026120878803695, -294.3383627706788843, -316.8636164766572847 ) ) ;
#87567 = CARTESIAN_POINT ( 'NONE',  ( -5.360778727914657260, -284.5495124266410585, -201.9028469816150562 ) ) ;
#87568 = CARTESIAN_POINT ( 'NONE',  ( -112.3833687534820172, -280.5363918678977484, -271.6014193245699744 ) ) ;
#87570 = CARTESIAN_POINT ( 'NONE',  ( -66.15671935062889020, -294.4975776610245930, -337.6894412632343005 ) ) ;
#87569 = VECTOR ( 'NONE', #66402, 1000.000000000000000 ) ;
#87571 = ORIENTED_EDGE ( 'NONE', *, *, #69946, .F. ) ;
#87572 = LINE ( 'NONE', #38319, #42296 ) ;
#87573 = CARTESIAN_POINT ( 'NONE',  ( 26.53095494188747239, -283.0108534428742360, -231.6328984051195050 ) ) ;
#87574 = CARTESIAN_POINT ( 'NONE',  ( -109.8663645048646345, -295.9379310576269972, -279.6074175544224545 ) ) ;
#87575 = CARTESIAN_POINT ( 'NONE',  ( 175.2296996224750103, 133.0000000000000000, 0.000000000000000000 ) ) ;
#87576 = CARTESIAN_POINT ( 'NONE',  ( 39.58706461736021254, -279.0523547857347921, -270.3937649182068981 ) ) ;
#87577 = CARTESIAN_POINT ( 'NONE',  ( -55.28597065623892348, -273.0241447500357594, -195.6472506271032046 ) ) ;
#87578 = CARTESIAN_POINT ( 'NONE',  ( -85.92744527199947413, -291.1901943325169100, -215.8098238759642982 ) ) ;
#87579 = CARTESIAN_POINT ( 'NONE',  ( -102.7803826199349970, -280.5301319594593679, -236.3606751181626464 ) ) ;
#87580 = CARTESIAN_POINT ( 'NONE',  ( -6.209839808988696142, -276.0683258064257757, -203.4488792625690223 ) ) ;
#87581 = CARTESIAN_POINT ( 'NONE',  ( 13.16593101578489033, -283.9605066859061253, -327.4876547216936729 ) ) ;
#87582 = CARTESIAN_POINT ( 'NONE',  ( 29.67075810574870331, -280.7495660452669881, -300.4268066405655304 ) ) ;
#87583 = CARTESIAN_POINT ( 'NONE',  ( -36.41663272233579107, -279.0407500617605479, -345.3682255897130631 ) ) ;
#87584 = EDGE_LOOP ( 'NONE', ( #12192, #61868, #69, #55502 ) ) ;
#87585 = CARTESIAN_POINT ( 'NONE',  ( -2.555644637146083475, -274.3326974178143587, -201.6519440078532455 ) ) ;
#87586 = CARTESIAN_POINT ( 'NONE',  ( -6.699395299630709566, -294.3777681672877407, -202.5203974996412342 ) ) ;
#87587 = LINE ( 'NONE', #71086, #83818 ) ;
#87588 = DIRECTION ( 'NONE',  ( 0.000000000000000000, 0.000000000000000000, 1.000000000000000000 ) ) ;
#87589 = CARTESIAN_POINT ( 'NONE',  ( 36.85605935456775484, -291.8865854144556238, -285.6907615350536958 ) ) ;
#87590 = CARTESIAN_POINT ( 'NONE',  ( -74.29910333014065316, -273.0545169139391533, -207.2776089167914506 ) ) ;
#87591 = DIRECTION ( 'NONE',  ( 0.000000000000000000, 0.000000000000000000, 1.000000000000000000 ) ) ;
#87592 = CARTESIAN_POINT ( 'NONE',  ( -30.77639269453639415, -293.6536957653947297, -194.2851246914145236 ) ) ;
#87594 = CARTESIAN_POINT ( 'NONE',  ( -74.49979213554404112, -292.7742028081192984, -203.3739183294904649 ) ) ;
#87593 = CARTESIAN_POINT ( 'NONE',  ( -4.771743288812468897, -279.1233781216988064, -337.9199732462171255 ) ) ;
#87595 = CARTESIAN_POINT ( 'NONE',  ( -20.69740580411836461, -290.8381335221212112, -343.3199823501925607 ) ) ;
#87596 = CARTESIAN_POINT ( 'NONE',  ( -24.02783698658281608, -274.8816854538034704, -344.0533143627347954 ) ) ;
#87597 = CARTESIAN_POINT ( 'NONE',  ( -9.426098482943086054, -278.6046351802551158, -339.3824413155019215 ) ) ;
#87598 = CARTESIAN_POINT ( 'NONE',  ( 25.63266268321738650, -292.1708600324493545, -310.1510163022412598 ) ) ;
#87599 = CARTESIAN_POINT ( 'NONE',  ( -6.751163037297327030, -282.3098324955339535, -201.0323995500967555 ) ) ;
#87600 = ORIENTED_EDGE ( 'NONE', *, *, #64244, .T. ) ;
#87601 = CARTESIAN_POINT ( 'NONE',  ( -91.68361916541283563, -283.5208182553025722, -319.1553718120687222 ) ) ;
#87602 = CARTESIAN_POINT ( 'NONE',  ( -97.46317221718877022, -280.2714837524911218, -222.7491330918078631 ) ) ;
#87603 = CARTESIAN_POINT ( 'NONE',  ( 11.22892348023847120, -281.1916719194254597, -329.6657441995660065 ) ) ;
#87604 = CARTESIAN_POINT ( 'NONE',  ( 12.56077744296938192, -277.3173491543691966, -328.6926098594030918 ) ) ;
#87605 = DIRECTION ( 'NONE',  ( 1.000000000000000000, 0.000000000000000000, 0.000000000000000000 ) ) ;
#87606 = CARTESIAN_POINT ( 'NONE',  ( 38.86070081911479690, -277.0104812500239291, -265.4647988023256744 ) ) ;
#87607 = CARTESIAN_POINT ( 'NONE',  ( 17.36665895637874613, -289.4090924074130839, -226.6919474004047572 ) ) ;
#87608 = EDGE_LOOP ( 'NONE', ( #68798, #39989, #63937, #1589 ) ) ;
#87609 = VERTEX_POINT ( 'NONE', #93118 ) ;
#87610 = CARTESIAN_POINT ( 'NONE',  ( -53.07894532440435853, -299.8507008661060809, -196.9774608745953799 ) ) ;
#87611 = CARTESIAN_POINT ( 'NONE',  ( -95.75560999814437935, -275.9302629771005400, -316.8537058867900100 ) ) ;
#87612 = CARTESIAN_POINT ( 'NONE',  ( -55.96245056272222484, -293.5758457683152187, -196.6370734048880422 ) ) ;
#87613 = CARTESIAN_POINT ( 'NONE',  ( -25.38425869722593831, -291.5570391642943378, -198.1922159257624116 ) ) ;
#87614 = CARTESIAN_POINT ( 'NONE',  ( -8.262206471111200656, -288.1891069550692919, -341.6067554536527382 ) ) ;
#87615 = FACE_OUTER_BOUND ( 'NONE', #12256, .T. ) ;
#87617 = CARTESIAN_POINT ( 'NONE',  ( -69.37464076112472355, -281.8807275088116739, -336.8606453119332969 ) ) ;
#87616 = CARTESIAN_POINT ( 'NONE',  ( 36.85418429646944816, -291.8966452661995277, -252.0970267261715207 ) ) ;
#87618 = CARTESIAN_POINT ( 'NONE',  ( -110.3902244750873223, -292.2410733930450419, -283.5815027249457785 ) ) ;
#87619 = CARTESIAN_POINT ( 'NONE',  ( -109.6050828115442499, -283.2208122014051810, -255.9142748241255561 ) ) ;
#87620 = CARTESIAN_POINT ( 'NONE',  ( 30.79798100044280318, -283.2335899928863796, -297.8970460153339559 ) ) ;
#87621 = ORIENTED_EDGE ( 'NONE', *, *, #10105, .F. ) ;
#87622 = CARTESIAN_POINT ( 'NONE',  ( -9.637034140845045727, -289.6401255389210405, -341.9521208772692376 ) ) ;
#87623 = CARTESIAN_POINT ( 'NONE',  ( 11.34216485102379757, -281.2413471421197073, -215.8829596785950287 ) ) ;
#87624 = CARTESIAN_POINT ( 'NONE',  ( -0.9787474148457222523, -291.3188778073098888, -202.9389822313664808 ) ) ;
#87625 = CARTESIAN_POINT ( 'NONE',  ( 26.21803381920792475, -287.7842217834903522, -227.1598572191831238 ) ) ;
#87626 = EDGE_CURVE ( 'NONE', #2619, #51697, #91707, .T. ) ;
#87627 = CARTESIAN_POINT ( 'NONE',  ( 28.85399186004476135, -288.5557832374823874, -309.5740911588089261 ) ) ;
#87628 = CARTESIAN_POINT ( 'NONE',  ( -9.495354637964695144, -286.5931257222802628, -202.8673832001296091 ) ) ;
#87629 = ORIENTED_EDGE ( 'NONE', *, *, #58308, .F. ) ;
#87630 = CARTESIAN_POINT ( 'NONE',  ( 175.2296996224750103, 20.00000000000000000, 0.000000000000000000 ) ) ;
#87631 = CARTESIAN_POINT ( 'NONE',  ( 28.51295730169438869, -295.9081890810738287, -307.9300671776576337 ) ) ;
#87632 = CARTESIAN_POINT ( 'NONE',  ( -47.58224614309366984, -293.8645745941540213, -346.1795160742690882 ) ) ;
#87633 = CARTESIAN_POINT ( 'NONE',  ( -109.5200206750281069, -277.4469026621178500, -282.8328312550918895 ) ) ;
#87634 = CARTESIAN_POINT ( 'NONE',  ( -91.55777619641089871, -296.6528586230794531, -215.8273680456153727 ) ) ;
#87635 = AXIS2_PLACEMENT_3D ( 'NONE', #40273, #69189, #48325 ) ;
#87636 = CARTESIAN_POINT ( 'NONE',  ( 4.916922602897884964, -291.1142213549914572, -209.9254083739679686 ) ) ;
#87637 = CARTESIAN_POINT ( 'NONE',  ( -102.3681490373165985, -294.3161472493381439, -305.7098796792338362 ) ) ;
#87638 = CARTESIAN_POINT ( 'NONE',  ( 20.01361989501665661, -295.4008420965192840, -316.1796064249823530 ) ) ;
#87639 = CARTESIAN_POINT ( 'NONE',  ( 34.37282683833672792, -294.8323773731113420, -285.6283781040641543 ) ) ;
#87640 = CARTESIAN_POINT ( 'NONE',  ( -43.18343439339132317, -283.1093320178187582, -430.6442049081568939 ) ) ;
#87641 = CARTESIAN_POINT ( 'NONE',  ( 12.16865261693645550, -292.3655376346080743, -326.9876309818918685 ) ) ;
#87642 = CIRCLE ( 'NONE', #58944, 2.500000000000000444 ) ;
#87643 = CARTESIAN_POINT ( 'NONE',  ( -108.4779915619095192, -298.2432961741336044, -294.2840549399437577 ) ) ;
#87644 = CARTESIAN_POINT ( 'NONE',  ( -109.6495107990008933, -291.3395972305177679, -282.0583913210004994 ) ) ;
#87645 = CARTESIAN_POINT ( 'NONE',  ( -50.47084430307474889, -295.5577315974794033, -342.1922606709545107 ) ) ;
#87646 = CARTESIAN_POINT ( 'NONE',  ( -86.01318886397322672, -279.7022791178366674, -327.9575643388695312 ) ) ;
#87647 = CARTESIAN_POINT ( 'NONE',  ( -73.51758170409270576, -278.2672920774273848, -202.9325873657557224 ) ) ;
#87648 = CARTESIAN_POINT ( 'NONE',  ( -3.862976237089331910, -273.8308176644274567, -201.1188311114435123 ) ) ;
#87649 = CARTESIAN_POINT ( 'NONE',  ( 37.14338441879935715, -279.6448739711028111, -271.3569532551027237 ) ) ;
#87650 = CARTESIAN_POINT ( 'NONE',  ( -101.2094472046138520, -277.5047043023939750, -228.7042607584561722 ) ) ;
#87651 = CARTESIAN_POINT ( 'NONE',  ( -45.05918793247583665, -277.9546122624539635, -195.5399520672403639 ) ) ;
#87652 = CARTESIAN_POINT ( 'NONE',  ( -92.20193278392555669, -295.9316335854428530, -221.4571472679120632 ) ) ;
#87653 = CARTESIAN_POINT ( 'NONE',  ( 23.02374208698441649, -276.9449014607387198, -225.8313406892640955 ) ) ;
#87654 = DIRECTION ( 'NONE',  ( 0.000000000000000000, 1.000000000000000000, 0.000000000000000000 ) ) ;
#87655 = CARTESIAN_POINT ( 'NONE',  ( -73.85926192655631439, -289.5897492496762879, -204.4454560773035894 ) ) ;
#87656 = CARTESIAN_POINT ( 'NONE',  ( -41.76055760479342638, -289.1063468511020460, -347.2474414363900337 ) ) ;
#87657 = CARTESIAN_POINT ( 'NONE',  ( 8.374651001252306770, -276.6764850633429091, -210.6950165269120134 ) ) ;
#87658 = CARTESIAN_POINT ( 'NONE',  ( -37.11921302921708588, -296.0547944567841796, -195.5249315462412483 ) ) ;
#87659 = EDGE_CURVE ( 'NONE', #37341, #55975, #14062, .T. ) ;
#87660 = CARTESIAN_POINT ( 'NONE',  ( -49.30947078709969844, -285.1006280993699420, -194.4066966165096915 ) ) ;
#87661 = ADVANCED_FACE ( 'NONE', ( #33969 ), #86864, .F. ) ;
#87662 = DIRECTION ( 'NONE',  ( -0.000000000000000000, -1.000000000000000000, -0.000000000000000000 ) ) ;
#87663 = CARTESIAN_POINT ( 'NONE',  ( -71.23061273360882240, -281.4993107491206956, -337.2821291566444302 ) ) ;
#87664 = CARTESIAN_POINT ( 'NONE',  ( 198.1541494672131876, 25.06826132699710996, 11.52973355076513684 ) ) ;
#87665 = CARTESIAN_POINT ( 'NONE',  ( 35.69205627309717244, -292.2449138296782962, -262.5749610052877188 ) ) ;
#87666 = CARTESIAN_POINT ( 'NONE',  ( -82.20657095559761274, -283.5722075174023757, -211.2171508925511603 ) ) ;
#87667 = CARTESIAN_POINT ( 'NONE',  ( 209.1990615267463056, 35.77166376090755762, 14.26711941829674579 ) ) ;
#87668 = FILL_AREA_STYLE_COLOUR ( '', #9504 ) ;
#87669 = CARTESIAN_POINT ( 'NONE',  ( 36.81157819309344603, -291.7006130131134114, -281.9361465053453912 ) ) ;
#87670 = CARTESIAN_POINT ( 'NONE',  ( -106.0047429214089476, -279.7944202747025884, -297.4134185876326342 ) ) ;
#87671 = CARTESIAN_POINT ( 'NONE',  ( -16.23642890538016559, -283.9904199334760619, -344.0542662701463996 ) ) ;
#87673 = CARTESIAN_POINT ( 'NONE',  ( -94.95705715023834159, -285.1839775431552653, -225.5137010795961032 ) ) ;
#87672 = CARTESIAN_POINT ( 'NONE',  ( -29.95486989272370337, -272.2248079214666063, -195.1630532701500442 ) ) ;
#87674 = CARTESIAN_POINT ( 'NONE',  ( 29.61468970115871713, -276.5675960214273914, -239.7056895592586159 ) ) ;
#87675 = CARTESIAN_POINT ( 'NONE',  ( -18.96653808151215159, -277.6123211135574707, -341.1774659977460828 ) ) ;
#87676 = CARTESIAN_POINT ( 'NONE',  ( -101.2014608117364247, -286.0245128539817188, -309.6921694911256964 ) ) ;
#87677 = VERTEX_POINT ( 'NONE', #55747 ) ;
#87678 = DIRECTION ( 'NONE',  ( 0.000000000000000000, 1.000000000000000000, 0.000000000000000000 ) ) ;
#87679 = CARTESIAN_POINT ( 'NONE',  ( -72.07593502769803706, -295.3321009502789707, -339.0818057735624507 ) ) ;
#87680 = CARTESIAN_POINT ( 'NONE',  ( 24.89174481380062431, -288.9716605667255749, -229.0505342790021643 ) ) ;
#87681 = CYLINDRICAL_SURFACE ( 'NONE', #29162, 1.000000000000000888 ) ;
#87682 = CARTESIAN_POINT ( 'NONE',  ( 25.22466315766300227, -278.6948066931273047, -320.2154176792147382 ) ) ;
#87683 = CARTESIAN_POINT ( 'NONE',  ( -94.72134569164256845, -278.1646786285700728, -219.4782251284936478 ) ) ;
#87684 = CARTESIAN_POINT ( 'NONE',  ( -4.925770865371022822, -290.8717779850562692, -201.3999118701938187 ) ) ;
#87685 = CARTESIAN_POINT ( 'NONE',  ( -30.48587862925580083, -287.6604026744830094, -196.9360993798321431 ) ) ;
#87686 = CARTESIAN_POINT ( 'NONE',  ( -86.16927336917946434, -281.1239701408817950, -214.7388013948472576 ) ) ;
#87687 = CARTESIAN_POINT ( 'NONE',  ( -2.056557930385312982, -290.0194516900936605, -338.1369620161691500 ) ) ;
#87688 = CARTESIAN_POINT ( 'NONE',  ( 37.68755262768855374, -283.5285420699671022, -268.5094602435746083 ) ) ;
#87689 = CARTESIAN_POINT ( 'NONE',  ( -65.09309052314583255, -277.5714437409737911, -342.2426101730581536 ) ) ;
#87690 = CARTESIAN_POINT ( 'NONE',  ( -35.06023292077971831, -296.1009576339022260, -195.7170838746797585 ) ) ;
#87691 = CARTESIAN_POINT ( 'NONE',  ( -33.91314828073721088, -279.9274891428796082, -193.4374867841462162 ) ) ;
#87692 = CARTESIAN_POINT ( 'NONE',  ( 10.05277193782247380, -300.5700594497022848, -195.9054571269808775 ) ) ;
#87693 = ADVANCED_FACE ( 'NONE', ( #5565 ), #34436, .T. ) ;
#87694 = CARTESIAN_POINT ( 'NONE',  ( 198.7947541974662613, 298.6649591161120156, -6.475578415184554792 ) ) ;
#87695 = CARTESIAN_POINT ( 'NONE',  ( -54.42813229853333468, -291.7662352645558599, -345.3683826091709648 ) ) ;
#87696 = CIRCLE ( 'NONE', #3092, 155.4364916446740210 ) ;
#87697 = CARTESIAN_POINT ( 'NONE',  ( -97.00332737469258859, -271.4298440896898796, -223.3030235470189666 ) ) ;
#87698 = CARTESIAN_POINT ( 'NONE',  ( 202.9738562182569694, 293.9636489450776367, -59.00000000000003553 ) ) ;
#87699 = CARTESIAN_POINT ( 'NONE',  ( -49.14568172656405665, -279.4053045768581569, -198.2594227186683327 ) ) ;
#87700 = CARTESIAN_POINT ( 'NONE',  ( 30.88962546190047931, -276.3064280074575549, -235.5402201521648351 ) ) ;
#87701 = VECTOR ( 'NONE', #21268, 1000.000000000000000 ) ;
#87702 = CARTESIAN_POINT ( 'NONE',  ( -96.09797787083066112, -282.9434806833758103, -319.7830803612201294 ) ) ;
#87703 = CARTESIAN_POINT ( 'NONE',  ( 12.85935342445114138, -290.1005334165959653, -324.8167002319706853 ) ) ;
#87704 = CARTESIAN_POINT ( 'NONE',  ( -89.15188416617448297, -298.8595847898933471, -214.2679860340728908 ) ) ;
#87705 = CARTESIAN_POINT ( 'NONE',  ( -73.10895954997174329, -298.7942267989574248, -202.5625366539127015 ) ) ;
#87707 = AXIS2_PLACEMENT_3D ( 'NONE', #42307, #4931, #76902 ) ;
#87706 = CARTESIAN_POINT ( 'NONE',  ( 34.89289578589387730, -295.8047943557069175, -289.9596233341212042 ) ) ;
#87708 = CARTESIAN_POINT ( 'NONE',  ( 28.07348933608626496, -279.0672813068800906, -234.0171857338120844 ) ) ;
#87709 = CARTESIAN_POINT ( 'NONE',  ( -21.56228543215167903, -272.2755627941558032, -197.4032063387302287 ) ) ;
#87710 = CARTESIAN_POINT ( 'NONE',  ( -35.19144490035210993, -287.6788166996584550, -194.1784527693881444 ) ) ;
#87711 = CARTESIAN_POINT ( 'NONE',  ( -78.35870518029398113, -288.5384435926697506, -331.1826799100534231 ) ) ;
#87712 = CARTESIAN_POINT ( 'NONE',  ( 204.8861976254080730, 294.6280088066694702, -54.00000000002151523 ) ) ;
#87713 = ORIENTED_EDGE ( 'NONE', *, *, #68670, .F. ) ;
#87714 = CARTESIAN_POINT ( 'NONE',  ( 9.849675925451636616, -286.9917841445231943, -330.5248428514432817 ) ) ;
#87715 = CARTESIAN_POINT ( 'NONE',  ( 20.37156175138847303, -287.8489544262758955, -315.1168829400816662 ) ) ;
#87716 = ORIENTED_EDGE ( 'NONE', *, *, #92091, .F. ) ;
#87717 = CARTESIAN_POINT ( 'NONE',  ( -105.1651740154182306, -286.0971535812261095, -234.4497636982327435 ) ) ;
#87718 = CARTESIAN_POINT ( 'NONE',  ( -13.77456064013578718, -277.0711167469324323, -339.5277835418974632 ) ) ;
#87719 = CARTESIAN_POINT ( 'NONE',  ( 33.12707991427834031, -292.8609785640342125, -300.7547782340529920 ) ) ;
#87720 = CARTESIAN_POINT ( 'NONE',  ( 27.76062937459834501, -281.6658322095683502, -229.3345862278431468 ) ) ;
#87721 = CARTESIAN_POINT ( 'NONE',  ( 36.99760797571403970, -282.8543526781491551, -253.0882274791171369 ) ) ;
#87722 = CARTESIAN_POINT ( 'NONE',  ( -18.91934070798767564, -283.1546766290548476, -345.1580238620608156 ) ) ;
#87723 = CARTESIAN_POINT ( 'NONE',  ( 19.68986935376914715, -281.2413681749819716, -224.7597192176230863 ) ) ;
#87724 = CARTESIAN_POINT ( 'NONE',  ( -106.6379572354042296, -276.4809262143061233, -236.9535640164627353 ) ) ;
#87725 = CARTESIAN_POINT ( 'NONE',  ( -83.79983398228941383, -219.7295597296427729, -352.6263433563659078 ) ) ;
#87726 = CARTESIAN_POINT ( 'NONE',  ( -79.64798785157238115, -279.6250536609471737, -332.1510719737299269 ) ) ;
#87727 = CARTESIAN_POINT ( 'NONE',  ( -64.64839057758955221, -182.1492425233583390, -361.6151995916652595 ) ) ;
#87728 = CARTESIAN_POINT ( 'NONE',  ( 187.6320441055845265, 269.2822349766076968, -137.7557671003276596 ) ) ;
#87729 = CARTESIAN_POINT ( 'NONE',  ( -77.56114516728148089, -296.8455196481110647, -209.2569580648613226 ) ) ;
#87730 = CARTESIAN_POINT ( 'NONE',  ( 39.59470444098784014, -293.0233091165462156, -267.4451949993101607 ) ) ;
#87731 = CARTESIAN_POINT ( 'NONE',  ( -20.90964142997582087, -109.3750234531322434, -359.1970471300297731 ) ) ;
#87733 = CARTESIAN_POINT ( 'NONE',  ( -98.01813882430053582, -288.3728288070954022, -312.3929722805241340 ) ) ;
#87732 = CARTESIAN_POINT ( 'NONE',  ( -84.83588423967957226, -295.9863936537509517, -210.5037143732127731 ) ) ;
#87734 = CARTESIAN_POINT ( 'NONE',  ( -63.99064704868445830, -297.2637255795025908, -339.7026515647153246 ) ) ;
#87735 = CARTESIAN_POINT ( 'NONE',  ( -10.52867414003060631, -290.0101937330874193, -338.8430767880722669 ) ) ;
#87736 = ORIENTED_EDGE ( 'NONE', *, *, #79684, .T. ) ;
#87737 = CARTESIAN_POINT ( 'NONE',  ( -68.12080236320932158, -296.3878132635525162, -340.6851329357700138 ) ) ;
#87738 = CARTESIAN_POINT ( 'NONE',  ( -42.68488116543220912, -286.4753045616939175, -197.4825853240655249 ) ) ;
#87739 = CARTESIAN_POINT ( 'NONE',  ( -37.23863709957562662, -296.8483480566467279, -193.7574484753887702 ) ) ;
#87740 = CARTESIAN_POINT ( 'NONE',  ( -73.36707471665447144, -292.3895830916884506, -202.4762905216695117 ) ) ;
#87741 = CARTESIAN_POINT ( 'NONE',  ( 39.44119486658600238, -294.1154316632586188, -276.0283630418419989 ) ) ;
#87742 = CARTESIAN_POINT ( 'NONE',  ( -41.59495959226429562, -292.1639144248005096, -197.4352824795317645 ) ) ;
#87743 = ORIENTED_EDGE ( 'NONE', *, *, #84671, .T. ) ;
#87744 = CARTESIAN_POINT ( 'NONE',  ( -110.4317800807580454, -274.7190581390205466, -250.9993558362557167 ) ) ;
#87745 = CARTESIAN_POINT ( 'NONE',  ( 23.32781192550636007, -273.7194835547869616, -223.5720484397543260 ) ) ;
#87746 = VERTEX_POINT ( 'NONE', #42926 ) ;
#87747 = CARTESIAN_POINT ( 'NONE',  ( -14.61386100977054880, -276.2730603983901574, -343.9218104195533670 ) ) ;
#87748 = CARTESIAN_POINT ( 'NONE',  ( -111.1409416881142960, -270.9882135121230249, -267.5870818430676081 ) ) ;
#87749 = CARTESIAN_POINT ( 'NONE',  ( 27.84016578767272421, -274.1699115899199342, -305.9958289008915244 ) ) ;
#87750 = CARTESIAN_POINT ( 'NONE',  ( -69.63948234451837038, -274.6962687544138930, -204.5501816681222067 ) ) ;
#87751 = CARTESIAN_POINT ( 'NONE',  ( -96.47844273691961803, -274.0973830620596914, -227.0766828920960165 ) ) ;
#87752 = CARTESIAN_POINT ( 'NONE',  ( -113.1714757354526029, -274.3837324972880083, -264.7240405394982190 ) ) ;
#87753 = CARTESIAN_POINT ( 'NONE',  ( 23.03436878347866212, -274.1852251613643148, -315.4514396538984329 ) ) ;
#87754 = CARTESIAN_POINT ( 'NONE',  ( -68.55333468295162902, -296.1248304046246744, -336.4787749857893004 ) ) ;
#87755 = CARTESIAN_POINT ( 'NONE',  ( 32.08999944322635400, -292.4505204592193195, -294.8982949945201426 ) ) ;
#87756 = DIRECTION ( 'NONE',  ( 0.000000000000000000, -1.000000000000000000, 0.000000000000000000 ) ) ;
#87757 = CARTESIAN_POINT ( 'NONE',  ( 14.84604505116894124, -276.8326866572894573, -326.9665113025326377 ) ) ;
#87758 = CARTESIAN_POINT ( 'NONE',  ( 5.175022792764202073, -274.8116094583524500, -210.9578614270271260 ) ) ;
#87759 = CARTESIAN_POINT ( 'NONE',  ( -113.3278864882182972, -283.3491378818575299, -261.4505762110455862 ) ) ;
#87760 = CARTESIAN_POINT ( 'NONE',  ( -109.8602776456810943, -298.8082655518210800, -250.3926887040111637 ) ) ;
#87761 = CARTESIAN_POINT ( 'NONE',  ( 209.0207885866473134, 36.54472185027779574, 14.72030241339632894 ) ) ;
#87762 = CARTESIAN_POINT ( 'NONE',  ( -57.42892732028073510, -284.9834640621994595, -199.9585149068916792 ) ) ;
#87763 = EDGE_CURVE ( 'NONE', #36646, #17445, #86932, .T. ) ;
#87764 = CARTESIAN_POINT ( 'NONE',  ( -109.1607529504536700, -276.5585648801060756, -288.3019083407866106 ) ) ;
#87765 = CARTESIAN_POINT ( 'NONE',  ( -96.57802182668140745, -276.5196006078688811, -314.0449661716374976 ) ) ;
#87767 = CARTESIAN_POINT ( 'NONE',  ( -14.72095575521275634, -284.7593253708719203, -341.9223017075121902 ) ) ;
#87766 = AXIS2_PLACEMENT_3D ( 'NONE', #3055, #39473, #61312 ) ;
#87768 = CARTESIAN_POINT ( 'NONE',  ( -5.147665521381033393, -275.6907077862326219, -204.3875763608342879 ) ) ;
#87769 = CARTESIAN_POINT ( 'NONE',  ( 154.0637704119390321, 19.72112694978655867, 13.30738029212317564 ) ) ;
#87770 = CARTESIAN_POINT ( 'NONE',  ( 26.96265883984539258, -274.4946107954796162, -311.3417942069518176 ) ) ;
#87771 = TOROIDAL_SURFACE ( 'NONE', #6165, 2.103083949679977582, 3.000000000000000000 ) ;
#87772 = CARTESIAN_POINT ( 'NONE',  ( -36.79216438632334985, -282.0592019842418949, -195.1837213708406580 ) ) ;
#87773 = EDGE_CURVE ( 'NONE', #91222, #43507, #19749, .T. ) ;
#87774 = DIRECTION ( 'NONE',  ( 0.000000000000000000, 0.000000000000000000, -1.000000000000000000 ) ) ;
#87775 = CARTESIAN_POINT ( 'NONE',  ( 25.15236128287760664, -288.9013629590166943, -227.8667723274509456 ) ) ;
#87776 = CARTESIAN_POINT ( 'NONE',  ( 153.5041831715920750, 19.57420759269873045, -11.76949543551211619 ) ) ;
#87777 = CARTESIAN_POINT ( 'NONE',  ( -110.9992461515954432, -288.7342405490479109, -256.1672670994903456 ) ) ;
#87778 = CARTESIAN_POINT ( 'NONE',  ( 204.6539576904058606, 300.0210572133868823, -5.225551010890672643 ) ) ;
#87779 = CARTESIAN_POINT ( 'NONE',  ( -98.24251575579194196, -271.8060356762467222, -229.1323689943044997 ) ) ;
#87780 = CARTESIAN_POINT ( 'NONE',  ( -110.4898117228061949, -288.8597326408641379, -257.4103788922319040 ) ) ;
#87781 = CARTESIAN_POINT ( 'NONE',  ( -30.04969936926732288, -125.9919632799748683, -361.3284013991797110 ) ) ;
#87782 = CARTESIAN_POINT ( 'NONE',  ( 164.6329196456214277, 249.5000000000000568, 23.09031830825855991 ) ) ;
#87783 = CARTESIAN_POINT ( 'NONE',  ( 35.71593305586371514, -286.3115636853480055, -292.4357594100327447 ) ) ;
#87784 = CARTESIAN_POINT ( 'NONE',  ( -36.16051173489322679, -284.6372286024638356, -344.1516675898475910 ) ) ;
#87785 = CARTESIAN_POINT ( 'NONE',  ( -109.7271653665450089, -282.4970424126898934, -293.5193965673146863 ) ) ;
#87786 = CARTESIAN_POINT ( 'NONE',  ( 33.29512897756002587, -282.7066286504908135, -249.7258740607108223 ) ) ;
#87787 = CARTESIAN_POINT ( 'NONE',  ( -16.07582197716827110, -283.5728422136733684, -340.3637190274759519 ) ) ;
#87788 = CARTESIAN_POINT ( 'NONE',  ( -43.03238562738368955, -291.1035554964944936, -345.5011399529491882 ) ) ;
#87789 = B_SPLINE_CURVE_WITH_KNOTS ( 'NONE', 3,
 ( #68443, #82174, #24892, #54227 ),
 .UNSPECIFIED., .F., .F.,
 ( 4, 4 ),
 ( 0.0006709229447830969287, 0.0008458583158006164563 ),
 .UNSPECIFIED. ) ;
#87790 = CARTESIAN_POINT ( 'NONE',  ( -71.39726666672559929, -273.9479541658585617, -201.3251659040370782 ) ) ;
#87791 = CARTESIAN_POINT ( 'NONE',  ( 27.65242258729247737, -286.1436706010331363, -308.8978304606699226 ) ) ;
#87792 = CARTESIAN_POINT ( 'NONE',  ( 7.234989325463415888, -274.6407946568432408, -207.5109817883472090 ) ) ;
#87793 = CARTESIAN_POINT ( 'NONE',  ( 0.08817779316672660905, -296.5316065945155515, -335.0022472712446984 ) ) ;
#87794 = CARTESIAN_POINT ( 'NONE',  ( -48.18343439339132317, -253.7899642232643203, -458.8318842538539002 ) ) ;
#87795 = CARTESIAN_POINT ( 'NONE',  ( -114.2704648735229114, -299.0519495502701943, -270.3937649182068981 ) ) ;
#87796 = CARTESIAN_POINT ( 'NONE',  ( -61.71395680402517314, -282.0602883975840882, -339.7489571766276413 ) ) ;
#87797 = CARTESIAN_POINT ( 'NONE',  ( -110.3994766756951265, -276.3247971815480923, -288.0953096142770278 ) ) ;
#87798 = CARTESIAN_POINT ( 'NONE',  ( 97.44483485902340192, -298.1127538979946507, -194.1970331066050619 ) ) ;
#87799 = CARTESIAN_POINT ( 'NONE',  ( 32.96034237152142765, -274.6340168712055174, -250.1423167060101775 ) ) ;
#87800 = CARTESIAN_POINT ( 'NONE',  ( 30.48638752210645109, -294.6875438753584149, -241.4199154866854826 ) ) ;
#87801 = CARTESIAN_POINT ( 'NONE',  ( -4.739066623368627162, -293.4336835495118976, -204.7691291320868459 ) ) ;
#87802 = CARTESIAN_POINT ( 'NONE',  ( -105.5398861930802923, -286.6945283810787828, -241.4720055665673328 ) ) ;
#87803 = CARTESIAN_POINT ( 'NONE',  ( 24.32808310391603257, -294.3737885216199857, -225.2452213375096903 ) ) ;
#87804 = CARTESIAN_POINT ( 'NONE',  ( 35.02545210688794697, -295.1840497100538414, -295.3488295946599465 ) ) ;
#87805 = CARTESIAN_POINT ( 'NONE',  ( -107.9701166240041914, -296.1412091993184390, -288.8666236863512609 ) ) ;
#87806 = CARTESIAN_POINT ( 'NONE',  ( -53.82392899427642874, -291.2638794729775213, -343.5276183582624867 ) ) ;
#87807 = CARTESIAN_POINT ( 'NONE',  ( -109.3021968867851825, -284.3703423667047332, -297.9083487441680518 ) ) ;
#87808 = CARTESIAN_POINT ( 'NONE',  ( -111.2332909333861295, -270.9045546711798806, -253.6178120569185808 ) ) ;
#87809 = CARTESIAN_POINT ( 'NONE',  ( -114.3549592388131089, -284.3543816369453907, -272.8471154920035815 ) ) ;
#87810 = CARTESIAN_POINT ( 'NONE',  ( -110.9027961722705271, -280.3675749993185491, -283.1097993243005249 ) ) ;
#87811 = CARTESIAN_POINT ( 'NONE',  ( -27.76965548478910861, -284.9713397811583491, -197.5908873549930433 ) ) ;
#87812 = CARTESIAN_POINT ( 'NONE',  ( 37.10208548340217760, -285.6744022902821598, -279.8948927138080194 ) ) ;
#87813 = CARTESIAN_POINT ( 'NONE',  ( -68.14823486232465655, -277.7915250317406617, -201.1280163957479488 ) ) ;
#87814 = CARTESIAN_POINT ( 'NONE',  ( 202.9737475146022803, 296.4636489462809550, -68.70538243550777224 ) ) ;
#87815 = CARTESIAN_POINT ( 'NONE',  ( -108.1544170132208791, -283.8225921268827392, -288.3485460695171128 ) ) ;
#87816 = CARTESIAN_POINT ( 'NONE',  ( 38.27835170231957562, -282.9120234988077982, -282.6749376175422981 ) ) ;
#87817 = CARTESIAN_POINT ( 'NONE',  ( -26.19061364126050151, -287.9722492800315194, -346.3115852793948193 ) ) ;
#87818 = ADVANCED_FACE ( 'NONE', ( #78461 ), #12667, .T. ) ;
#87819 = CARTESIAN_POINT ( 'NONE',  ( -37.10873657626705580, -278.6493676701351205, -346.5736879694478034 ) ) ;
#87820 = CARTESIAN_POINT ( 'NONE',  ( -8.057802707929381469, -277.9916883904425049, -341.0559438451780352 ) ) ;
#87821 = CARTESIAN_POINT ( 'NONE',  ( -7.997497824453166260, -280.2808996707357210, -203.5049603901559294 ) ) ;
#87822 = CARTESIAN_POINT ( 'NONE',  ( -13.56486134083658435, -276.3422641958318309, -199.6044311005867939 ) ) ;
#87823 = CARTESIAN_POINT ( 'NONE',  ( 32.23002095770841180, -293.9764070862005383, -303.4820113631884055 ) ) ;
#87824 = CARTESIAN_POINT ( 'NONE',  ( 34.05526970268553555, -285.8438185008992605, -292.9499299655890923 ) ) ;
#87825 = CARTESIAN_POINT ( 'NONE',  ( -50.44898863516970522, -293.4875930038789420, -195.2968828128720702 ) ) ;
#87826 = CARTESIAN_POINT ( 'NONE',  ( 27.42474573565889173, -292.9396627380633049, -304.8138938082633445 ) ) ;
#87827 = CARTESIAN_POINT ( 'NONE',  ( -36.99971132733521273, -294.7144391003879491, -343.3938889260370502 ) ) ;
#87828 = CARTESIAN_POINT ( 'NONE',  ( -113.9418871746607351, -291.5850002449833482, -274.0899051016820067 ) ) ;
#87829 = CARTESIAN_POINT ( 'NONE',  ( 35.66814197358649352, -282.2518914777602959, -274.0293088406166930 ) ) ;
#87830 = CARTESIAN_POINT ( 'NONE',  ( -91.99311309434833106, -272.3536719687461414, -216.4533887270412151 ) ) ;
#87831 = CARTESIAN_POINT ( 'NONE',  ( 20.50170990633611368, -288.8901530173038168, -321.0509953840277717 ) ) ;
#87832 = CARTESIAN_POINT ( 'NONE',  ( 14.88466924481015674, -280.4648643266436920, -325.2492935840791688 ) ) ;
#87833 = CARTESIAN_POINT ( 'NONE',  ( -12.22661540687209225, -289.0675544385782700, -343.1835667766744677 ) ) ;
#87834 = CARTESIAN_POINT ( 'NONE',  ( -9.489252198181928222, -286.7596999542889193, -202.8470241216411694 ) ) ;
#87835 = CARTESIAN_POINT ( 'NONE',  ( 184.9426652459831644, 263.7189940585919317, -153.2499980065188083 ) ) ;
#87836 = CARTESIAN_POINT ( 'NONE',  ( 172.1150633234479130, 242.8691282751317715, -178.3881156067890856 ) ) ;
#87837 = CARTESIAN_POINT ( 'NONE',  ( -111.3619333908369669, -270.6190337206908225, -283.6441699463446184 ) ) ;
#87838 = CIRCLE ( 'NONE', #15272, 0.4999999999999923395 ) ;
#87839 = CARTESIAN_POINT ( 'NONE',  ( -103.2809712672784315, -277.3200524974452605, -302.1740254065236400 ) ) ;
#87840 = CARTESIAN_POINT ( 'NONE',  ( -108.5868433879396378, -277.6994155706966012, -253.0881438177620737 ) ) ;
#87841 = CARTESIAN_POINT ( 'NONE',  ( -93.15391103601244538, -272.9438044071365539, -217.3254572891859482 ) ) ;
#87842 = CARTESIAN_POINT ( 'NONE',  ( -110.3499187692159751, -272.5619384843310513, -283.8193449378834998 ) ) ;
#87843 = CARTESIAN_POINT ( 'NONE',  ( -86.41232297056691891, -277.9613019756524750, -211.7201583158244773 ) ) ;
#87844 = CARTESIAN_POINT ( 'NONE',  ( 16.85473502620386910, -296.0538781816921983, -323.6968519325373563 ) ) ;
#87845 = EDGE_CURVE ( 'NONE', #30132, #78431, #7084, .T. ) ;
#87846 = CARTESIAN_POINT ( 'NONE',  ( -14.83339368574036321, -292.8441582102327061, -200.8530998648516004 ) ) ;
#87847 = CARTESIAN_POINT ( 'NONE',  ( -109.8834447827226768, -273.8109361534544632, -245.2510503775759219 ) ) ;
#87848 = CARTESIAN_POINT ( 'NONE',  ( -8.037149255852190421, -287.3450067515114483, -337.8134887777105746 ) ) ;
#87849 = CARTESIAN_POINT ( 'NONE',  ( -94.07567327386276190, -273.9106882332212649, -218.4324347911523887 ) ) ;
#87850 = CARTESIAN_POINT ( 'NONE',  ( -72.84873852150612095, -297.7343737101769534, -206.5782815056311961 ) ) ;
#87851 = ORIENTED_EDGE ( 'NONE', *, *, #39617, .F. ) ;
#87852 = FACE_OUTER_BOUND ( 'NONE', #90554, .T. ) ;
#87853 = CARTESIAN_POINT ( 'NONE',  ( -61.60874427780643714, -281.6595886891419696, -198.7487871562420594 ) ) ;
#87854 = CARTESIAN_POINT ( 'NONE',  ( -108.9115236253497727, -279.8410365807625340, -254.4295215951917157 ) ) ;
#87855 = CARTESIAN_POINT ( 'NONE',  ( -106.6426046061193347, -279.9074602337205988, -301.6556943183560406 ) ) ;
#87856 = CARTESIAN_POINT ( 'NONE',  ( -51.67756258524116220, -272.3454429611390424, -198.0233580618600229 ) ) ;
#87857 = CARTESIAN_POINT ( 'NONE',  ( -23.40286736638519471, -122.5496321078137356, -21.50000000000000000 ) ) ;
#87858 = CARTESIAN_POINT ( 'NONE',  ( 175.2296996224750103, 160.0000000000000568, 0.000000000000000000 ) ) ;
#87859 = CARTESIAN_POINT ( 'NONE',  ( -66.07165578414669938, -279.8320861067056740, -203.2386890866297620 ) ) ;
#87860 = CARTESIAN_POINT ( 'NONE',  ( 27.51802948873118737, -276.8971844221867400, -311.6592441789029522 ) ) ;
#87861 = CARTESIAN_POINT ( 'NONE',  ( 0.07202887891175330237, -278.5547186161049353, -335.4216775580864578 ) ) ;
#87862 = CARTESIAN_POINT ( 'NONE',  ( -41.37165895666818471, -275.6766613382840774, -346.6786536304115316 ) ) ;
#87863 = EDGE_LOOP ( 'NONE', ( #193, #48275, #27327 ) ) ;
#87864 = CARTESIAN_POINT ( 'NONE',  ( 76.08708295871279859, -293.9068999365417199, -430.6442049081568939 ) ) ;
#87865 = CARTESIAN_POINT ( 'NONE',  ( 25.36740913513376228, -284.0940114570599349, -312.1459767013844839 ) ) ;
#87866 = CARTESIAN_POINT ( 'NONE',  ( -52.39302613426399802, -291.0517364691212379, -198.7126004384512612 ) ) ;
#87867 = CARTESIAN_POINT ( 'NONE',  ( -30.88413497854260825, -285.4803013588013414, -193.7213920461151702 ) ) ;
#87868 = ADVANCED_FACE ( 'NONE', ( #42449 ), #18883, .T. ) ;
#87869 = CARTESIAN_POINT ( 'NONE',  ( -102.6761366201529881, -282.3233178885338930, -305.2464769691491142 ) ) ;
#87870 = CARTESIAN_POINT ( 'NONE',  ( -21.27712114649834874, -281.4169056330804892, -342.2279213674067933 ) ) ;
#87871 = CARTESIAN_POINT ( 'NONE',  ( 33.83691006298187887, -282.5215504107740685, -252.4009963932691960 ) ) ;
#87872 = FACE_OUTER_BOUND ( 'NONE', #83541, .T. ) ;
#87873 = CARTESIAN_POINT ( 'NONE',  ( -0.7774042487873865648, -280.9747885032955423, -337.2301645685524818 ) ) ;
#87874 = CARTESIAN_POINT ( 'NONE',  ( -2.863612568200582853, -296.5965519383203741, -336.9663890208366865 ) ) ;
#87875 = CARTESIAN_POINT ( 'NONE',  ( -92.58994931416631857, -287.2637938616313136, -219.3175681747101464 ) ) ;
#87876 = CARTESIAN_POINT ( 'NONE',  ( 151.4851178187871312, 20.00000000000000000, 3.492110388858666870 ) ) ;
#87877 = CARTESIAN_POINT ( 'NONE',  ( -89.80406003569667917, -293.2393824680316925, -215.9100361501383816 ) ) ;
#87878 = CARTESIAN_POINT ( 'NONE',  ( -10.56310195994404744, -274.7026527240260521, -340.4175761360866090 ) ) ;
#87879 = CARTESIAN_POINT ( 'NONE',  ( 3.086462501390835111, -287.7214100702919382, -335.7666434807213136 ) ) ;
#87880 = CARTESIAN_POINT ( 'NONE',  ( 35.00472939265675620, -291.7618352757755247, -255.7859832433047131 ) ) ;
#87881 = CARTESIAN_POINT ( 'NONE',  ( -78.92473631777671983, -276.3102529597454122, -331.0209059810728149 ) ) ;
#87882 = CARTESIAN_POINT ( 'NONE',  ( -111.4764145802917739, -294.6416401280158084, -274.2224119298620622 ) ) ;
#87883 = CARTESIAN_POINT ( 'NONE',  ( -78.43638957310510307, -290.9329033703104983, -331.3524169317448695 ) ) ;
#87884 = CARTESIAN_POINT ( 'NONE',  ( 139.1539576904058606, 250.5000000000000568, -10.49999999999999822 ) ) ;
#87885 = CARTESIAN_POINT ( 'NONE',  ( -5.802570524182329770, -229.5268262511776527, -22.50000000000000000 ) ) ;
#87886 = CARTESIAN_POINT ( 'NONE',  ( -95.99106007723788991, -294.3693075224383620, -319.1970165281655341 ) ) ;
#87887 = CARTESIAN_POINT ( 'NONE',  ( 33.08310672844088884, -289.4435265653527836, -292.5946040085141817 ) ) ;
#87888 = CARTESIAN_POINT ( 'NONE',  ( -105.0903484159690464, -289.2422833965050017, -235.8344908930976089 ) ) ;
#87889 = EDGE_CURVE ( 'NONE', #91480, #35022, #30986, .T. ) ;
#87890 = CARTESIAN_POINT ( 'NONE',  ( -73.82141028047767861, -290.9719447049801602, -334.2865637977051847 ) ) ;
#87891 = DIRECTION ( 'NONE',  ( -0.000000000000000000, -1.000000000000000000, -0.000000000000000000 ) ) ;
#87892 = CARTESIAN_POINT ( 'NONE',  ( -58.72658632304552384, -290.1386151735616750, -340.3803734966105594 ) ) ;
#87893 = CARTESIAN_POINT ( 'NONE',  ( 196.8803347170859865, 250.0000000000000568, -12.49999999999999289 ) ) ;
#87894 = CARTESIAN_POINT ( 'NONE',  ( 28.56994127070791833, -289.2683969637597556, -309.3952600369004244 ) ) ;
#87895 = CARTESIAN_POINT ( 'NONE',  ( -50.62440045209152828, -277.9034137490165222, -196.1858075877599674 ) ) ;
#87896 = CARTESIAN_POINT ( 'NONE',  ( -17.00166326942441941, -280.6411188445425182, -196.1180900807452190 ) ) ;
#87897 = EDGE_CURVE ( 'NONE', #63820, #29329, #43084, .T. ) ;
#87898 = CARTESIAN_POINT ( 'NONE',  ( -84.55061755013238667, -279.0890620244917955, -209.4901913336462655 ) ) ;
#87899 = CARTESIAN_POINT ( 'NONE',  ( -22.02722297091859005, -284.2480557307476943, -196.8880092554559553 ) ) ;
#87900 = DIRECTION ( 'NONE',  ( 0.000000000000000000, -1.000000000000000000, 0.000000000000000000 ) ) ;
#87901 = CARTESIAN_POINT ( 'NONE',  ( -7.481216490278900899, -278.5874375800243001, -202.3823900990478535 ) ) ;
#87902 = CARTESIAN_POINT ( 'NONE',  ( -0.1462403245302671961, -280.5572363392818716, -335.5027392383176448 ) ) ;
#87903 = CARTESIAN_POINT ( 'NONE',  ( 65.57626948303558834, 46.04035151990646568, -315.5245225855154558 ) ) ;
#87904 = CARTESIAN_POINT ( 'NONE',  ( -102.8067277124654737, -277.5490806789696876, -231.0533460065475992 ) ) ;
#87905 = AXIS2_PLACEMENT_3D ( 'NONE', #60913, #75115, #25834 ) ;
#87906 = CARTESIAN_POINT ( 'NONE',  ( -93.28324136726352833, -298.7488908410369390, -222.3703382689367345 ) ) ;
#87907 = CARTESIAN_POINT ( 'NONE',  ( -93.21579149257897257, -282.7524505627250733, -322.9120638260972100 ) ) ;
#87908 = CARTESIAN_POINT ( 'NONE',  ( -93.04335610944514201, -274.0283414755382978, -222.9083780918271316 ) ) ;
#87909 = CARTESIAN_POINT ( 'NONE',  ( -100.7299780848046851, -274.5449262412594749, -227.5991901259323811 ) ) ;
#87910 = CARTESIAN_POINT ( 'NONE',  ( 9.674423792316273918, -276.0506426022662367, -326.2321442679535153 ) ) ;
#87911 = CARTESIAN_POINT ( 'NONE',  ( -50.80591882042548235, -297.2243425790355218, -344.1426567367664120 ) ) ;
#87912 = CARTESIAN_POINT ( 'NONE',  ( -99.02786209136434081, -290.1054647251472716, -316.4678148511616769 ) ) ;
#87913 = CARTESIAN_POINT ( 'NONE',  ( -35.34902974488176142, -278.1567995710110495, -194.8145030839573622 ) ) ;
#87914 = CARTESIAN_POINT ( 'NONE',  ( -103.2147430340040017, -290.9070216713524815, -230.3867501558528659 ) ) ;
#87915 = CARTESIAN_POINT ( 'NONE',  ( -63.91742271541528453, -288.4660337244906714, -338.6587187799153753 ) ) ;
#87916 = CARTESIAN_POINT ( 'NONE',  ( 31.49900719815166994, -291.1625969176334365, -240.5960770669717022 ) ) ;
#87917 = ORIENTED_EDGE ( 'NONE', *, *, #78116, .F. ) ;
#87918 = CARTESIAN_POINT ( 'NONE',  ( 152.0194914954574870, 20.99319818809533089, 6.266237208439005890 ) ) ;
#87919 = CARTESIAN_POINT ( 'NONE',  ( -91.71476639531482533, -290.7578320876427256, -221.5411972717067215 ) ) ;
#87920 = CARTESIAN_POINT ( 'NONE',  ( 209.6287663260176259, 29.00782453271233052, 12.90102856104451412 ) ) ;
#87921 = CARTESIAN_POINT ( 'NONE',  ( 14.08034650069721394, -287.6942441104267800, -213.2933802456728927 ) ) ;
#87922 = CARTESIAN_POINT ( 'NONE',  ( 7.450504543161046378, -290.9090924074130839, -326.4764044574609443 ) ) ;
#87923 = CARTESIAN_POINT ( 'NONE',  ( -76.97106242482884397, -294.6277348318757277, -336.1674232490917120 ) ) ;
#87924 = CARTESIAN_POINT ( 'NONE',  ( 33.11834065751056499, -283.2506969315764422, -300.3072340868965853 ) ) ;
#87925 = CARTESIAN_POINT ( 'NONE',  ( -103.4845654490978006, -284.8040106972706553, -239.3524400010108195 ) ) ;
#87926 = CARTESIAN_POINT ( 'NONE',  ( 31.57499046054697445, -276.5291850193854657, -244.8320514969676083 ) ) ;
#87927 = CARTESIAN_POINT ( 'NONE',  ( -15.12683528741805006, -292.7832932191679447, -341.6779998885816667 ) ) ;
#87928 = CARTESIAN_POINT ( 'NONE',  ( -34.00736838304376164, -272.8899445245073139, -197.0398200030965086 ) ) ;
#87929 = ORIENTED_EDGE ( 'NONE', *, *, #29767, .T. ) ;
#87930 = CARTESIAN_POINT ( 'NONE',  ( 196.0143093133015384, 42.36571313990104670, 11.99999999999999112 ) ) ;
#87931 = CARTESIAN_POINT ( 'NONE',  ( -41.94853952484770332, -294.7752964004404816, -347.2543800968483083 ) ) ;
#87932 = CARTESIAN_POINT ( 'NONE',  ( -49.68389497884351869, -287.8138363986287800, -196.8988984098576225 ) ) ;
#87933 = CARTESIAN_POINT ( 'NONE',  ( -106.2416603535695003, -298.0660356230430352, -236.6819257446770735 ) ) ;
#87934 = CARTESIAN_POINT ( 'NONE',  ( -4.556271929034998003, -287.1474464090086940, -205.0234690629803822 ) ) ;
#87935 = CARTESIAN_POINT ( 'NONE',  ( -104.7746302762587334, -277.1347619277786407, -307.0438134120429936 ) ) ;
#87936 = CARTESIAN_POINT ( 'NONE',  ( -47.60974176277625247, -295.8308449965302316, -346.5705669201018964 ) ) ;
#87937 = CARTESIAN_POINT ( 'NONE',  ( -86.59965555868208753, -287.8673341026253638, -327.9970452266349525 ) ) ;
#87938 = CARTESIAN_POINT ( 'NONE',  ( -0.7124965584789343387, -294.9125224610830855, -338.0815808444419304 ) ) ;
#87939 = CARTESIAN_POINT ( 'NONE',  ( -20.07127747165285214, -292.6134109575561979, -199.3594156553337200 ) ) ;
#87940 = CARTESIAN_POINT ( 'NONE',  ( 196.0143093133015384, 73.40565171261611965, -12.00000000000000355 ) ) ;
#87941 =( NAMED_UNIT ( * ) SI_UNIT ( $, .STERADIAN. ) SOLID_ANGLE_UNIT ( ) );
#87942 = CARTESIAN_POINT ( 'NONE',  ( 202.8071895515903122, 291.9636489450776367, -53.99999999998529887 ) ) ;
#87943 = CARTESIAN_POINT ( 'NONE',  ( 22.43654311266901757, -288.4316029728053081, -222.9138358805863049 ) ) ;
#87944 = CARTESIAN_POINT ( 'NONE',  ( -55.63300648810263738, -280.7666405000205145, -350.3538533559490702 ) ) ;
#87945 = ORIENTED_EDGE ( 'NONE', *, *, #75074, .T. ) ;
#87946 = CARTESIAN_POINT ( 'NONE',  ( -106.4697971116899708, -283.1472905864703762, -294.9158951522919097 ) ) ;
#87947 = CARTESIAN_POINT ( 'NONE',  ( -68.62345302996259022, -279.0003322675260051, -200.0988715810434257 ) ) ;
#87948 = CARTESIAN_POINT ( 'NONE',  ( 8.239338077805580696, -282.6770541049942835, -210.9457823598843902 ) ) ;
#87949 = CARTESIAN_POINT ( 'NONE',  ( 195.6275670422409121, 276.7432394079091864, -125.1359736961868094 ) ) ;
#87950 = CARTESIAN_POINT ( 'NONE',  ( -85.13016272798500950, -283.9816499904911211, -210.7383946833309096 ) ) ;
#87951 = CARTESIAN_POINT ( 'NONE',  ( -40.03424356761348690, -287.1659660441360984, -344.8029690430848291 ) ) ;
#87952 = CARTESIAN_POINT ( 'NONE',  ( -70.87772589190122119, -275.4748417354322214, -202.4226129911748444 ) ) ;
#87953 = CARTESIAN_POINT ( 'NONE',  ( -35.82025859689427705, -298.5640525009145563, -197.2994475690733225 ) ) ;
#87954 = CARTESIAN_POINT ( 'NONE',  ( -69.95788853338572721, -294.1759199753086023, -336.2202687019762379 ) ) ;
#87955 = CARTESIAN_POINT ( 'NONE',  ( -110.4553604842015062, -279.5056089338852416, -246.3654859261420711 ) ) ;
#87956 = CARTESIAN_POINT ( 'NONE',  ( -6.276626249304853467, -276.6322962131042118, -336.4351709322590978 ) ) ;
#87957 = CARTESIAN_POINT ( 'NONE',  ( -70.01263078546087115, -274.7115398422857311, -200.9630256873461178 ) ) ;
#87958 = CARTESIAN_POINT ( 'NONE',  ( -70.18118318084478346, -276.3950422615041589, -339.6796170912918456 ) ) ;
#87959 = CARTESIAN_POINT ( 'NONE',  ( 201.7240241516113883, 293.7293971981039249, -83.18315247050524874 ) ) ;
#87960 = CARTESIAN_POINT ( 'NONE',  ( 35.71074788677532297, -273.3332557589060912, -253.3251306200568536 ) ) ;
#87961 = ADVANCED_FACE ( 'NONE', ( #58086 ), #29478, .F. ) ;
#87962 = CARTESIAN_POINT ( 'NONE',  ( -113.0207262607261498, -298.1115689942610629, -259.7168405879997977 ) ) ;
#87963 = CARTESIAN_POINT ( 'NONE',  ( -4.829096099716510437, -276.9805209788416391, -202.7746430608542312 ) ) ;
#87964 = VECTOR ( 'NONE', #21161, 1000.000000000000114 ) ;
#87965 = CARTESIAN_POINT ( 'NONE',  ( 209.3463111024439343, 0.03396820302666800351, -7.457905934263069803 ) ) ;
#87966 = CIRCLE ( 'NONE', #7824, 7.500000000000012434 ) ;
#87967 = CARTESIAN_POINT ( 'NONE',  ( 0.3156950102680667891, -287.6458032309157602, -207.4040360855865401 ) ) ;
#87968 = CARTESIAN_POINT ( 'NONE',  ( -111.5308084045867645, -286.1040646807946359, -286.7912802056800388 ) ) ;
#87969 = CARTESIAN_POINT ( 'NONE',  ( -71.21810162729639160, -284.9410305949313624, -205.5824016482220031 ) ) ;
#87970 = CARTESIAN_POINT ( 'NONE',  ( -100.1378508476021949, -277.4820002764039941, -231.4940445704830267 ) ) ;
#87971 = CARTESIAN_POINT ( 'NONE',  ( -96.89878241031334483, -285.8012777371054653, -314.6761203247119738 ) ) ;
#87972 = CARTESIAN_POINT ( 'NONE',  ( -51.94600347293249598, -278.3418665363128071, -198.0771736227187887 ) ) ;
#87973 = CARTESIAN_POINT ( 'NONE',  ( 22.72699112690552425, -277.2164240022154900, -312.4718365316028326 ) ) ;
#87974 = CARTESIAN_POINT ( 'NONE',  ( -24.59185279622966291, -274.7114757930288533, -198.3690263999752119 ) ) ;
#87975 = CIRCLE ( 'NONE', #47085, 1.000000000000000888 ) ;
#87976 = CARTESIAN_POINT ( 'NONE',  ( 33.42122297475751935, -282.7384379602993931, -300.4431182021271525 ) ) ;
#87977 = CARTESIAN_POINT ( 'NONE',  ( -37.30797974140362072, -283.5440486210492850, -347.3126272967377872 ) ) ;
#87978 = VERTEX_POINT ( 'NONE', #19373 ) ;
#87979 = ORIENTED_EDGE ( 'NONE', *, *, #15328, .F. ) ;
#87980 = CARTESIAN_POINT ( 'NONE',  ( 199.0883366025630323, 17.54655016014115176, -10.45170682515238170 ) ) ;
#87981 = CARTESIAN_POINT ( 'NONE',  ( -2.807406897773097487, -288.3640664758796106, -202.9100554294749372 ) ) ;
#87982 = CARTESIAN_POINT ( 'NONE',  ( -107.2873572870556416, -288.8373857931518387, -301.4899233774992808 ) ) ;
#87983 = CARTESIAN_POINT ( 'NONE',  ( -108.9350283906195642, -295.9484065043043302, -255.2345005460501852 ) ) ;
#87984 = CARTESIAN_POINT ( 'NONE',  ( -19.40249083884732428, -291.6255195040851618, -195.5300499481670613 ) ) ;
#87985 = ADVANCED_FACE ( 'NONE', ( #26484 ), #49161, .F. ) ;
#87986 = CARTESIAN_POINT ( 'NONE',  ( 12.61169566093211181, -286.8207983584915723, -324.6094593921056344 ) ) ;
#87987 = CARTESIAN_POINT ( 'NONE',  ( -61.46516422921862954, -287.9464802710733693, -339.8840163422664773 ) ) ;
#87988 = CARTESIAN_POINT ( 'NONE',  ( -65.25838830001563906, -286.8841930095118187, -202.4263146863197562 ) ) ;
#87989 = CARTESIAN_POINT ( 'NONE',  ( -111.1034233778913887, -276.3768176456035235, -284.0041622790973292 ) ) ;
#87990 = CARTESIAN_POINT ( 'NONE',  ( 36.36535705571708377, -286.1965563239162407, -289.6927019466888851 ) ) ;
#87991 = CARTESIAN_POINT ( 'NONE',  ( 37.36010764197031619, -289.4593949982132131, -263.1242357017363815 ) ) ;
#87992 = CARTESIAN_POINT ( 'NONE',  ( 4.514799762249682047, -286.4885950582082046, -332.7955783505865384 ) ) ;
#87993 = CARTESIAN_POINT ( 'NONE',  ( -104.3236853509115463, -285.0961815561117874, -299.9723000431780520 ) ) ;
#87994 = CARTESIAN_POINT ( 'NONE',  ( -70.12177187658431876, -293.6214269528587124, -202.7187102213882497 ) ) ;
#87995 = LINE ( 'NONE', #23148, #39784 ) ;
#87996 = FACE_OUTER_BOUND ( 'NONE', #57685, .T. ) ;
#87997 = CARTESIAN_POINT ( 'NONE',  ( -97.95226509816951932, -299.0840389123143268, -225.2210749450559888 ) ) ;
#87998 = CARTESIAN_POINT ( 'NONE',  ( -39.69620903541504475, -279.2190284270445204, -197.2249899774763833 ) ) ;
#87999 = CARTESIAN_POINT ( 'NONE',  ( 35.58915388519211120, -279.7773365921232198, -287.9111417896199896 ) ) ;
#88000 = CARTESIAN_POINT ( 'NONE',  ( 38.16845473548401202, -292.5710351991092466, -256.1352495251503569 ) ) ;
#88001 = CARTESIAN_POINT ( 'NONE',  ( -74.76669074656729208, -271.7869274108691684, -206.4476740750432668 ) ) ;
#88002 = CARTESIAN_POINT ( 'NONE',  ( -32.34790973844188500, -275.0686768468325454, -344.6843819489247949 ) ) ;
#88003 = CARTESIAN_POINT ( 'NONE',  ( -86.80963664459045503, -297.0729216642727692, -324.7133647965742966 ) ) ;
#88004 = CARTESIAN_POINT ( 'NONE',  ( 139.6925840978351516, 0.000000000000000000, -21.49999999999998579 ) ) ;
#88005 = CARTESIAN_POINT ( 'NONE',  ( -46.79001135833403424, -272.5091478152562559, -194.5367438878168116 ) ) ;
#88006 = CARTESIAN_POINT ( 'NONE',  ( -110.9920956273559653, -294.5543349724370614, -289.1111225983144095 ) ) ;
#88007 = ADVANCED_FACE ( 'NONE', ( #4233 ), #52183, .T. ) ;
#88008 = CARTESIAN_POINT ( 'NONE',  ( 32.91470747113712036, -295.2652479807409236, -292.2565994486166119 ) ) ;
#88009 = DIRECTION ( 'NONE',  ( 0.000000000000000000, 0.000000000000000000, 1.000000000000000000 ) ) ;
#88010 = CARTESIAN_POINT ( 'NONE',  ( -84.57457205418812407, -296.5248457773866448, -326.2994218480039308 ) ) ;
#88011 = CARTESIAN_POINT ( 'NONE',  ( -36.09237171215955442, -122.5496321078137356, -22.50000000000000000 ) ) ;
#88013 = CARTESIAN_POINT ( 'NONE',  ( -110.3841182491784991, -296.5376149731446276, -271.4631167961459823 ) ) ;
#88012 = CARTESIAN_POINT ( 'NONE',  ( -57.29559367141229842, -283.8161574905348630, -197.6416323532493493 ) ) ;
#88014 = CARTESIAN_POINT ( 'NONE',  ( -76.75789514397068558, -283.5641499417304772, -336.5694682708411847 ) ) ;
#88015 = CARTESIAN_POINT ( 'NONE',  ( 32.24941778125134562, -283.8555796135488549, -299.9293527373164352 ) ) ;
#88016 = CARTESIAN_POINT ( 'NONE',  ( -64.53574935218415476, -285.3734318282904496, -198.3314841712942211 ) ) ;
#88017 = CARTESIAN_POINT ( 'NONE',  ( -0.3282714067713123907, -290.5452906432827263, -205.3075611051781948 ) ) ;
#88018 = CARTESIAN_POINT ( 'NONE',  ( -95.95921662488163406, -276.6952119285918457, -223.5744983911110353 ) ) ;
#88019 = CARTESIAN_POINT ( 'NONE',  ( -48.18343439339133027, -272.5190275734900069, -500.7427710989320531 ) ) ;
#88020 = CARTESIAN_POINT ( 'NONE',  ( 7.179900938095929774, -285.4687564448618673, -211.9448784554365659 ) ) ;
#88021 = CARTESIAN_POINT ( 'NONE',  ( -69.24132009131211873, -288.3823767429618670, -340.1171996956661587 ) ) ;
#88022 = PLANE ( 'NONE',  #55166 ) ;
#88023 = CARTESIAN_POINT ( 'NONE',  ( -113.6236803329639429, -280.0333115146350451, -265.9265055395104014 ) ) ;
#88025 = CARTESIAN_POINT ( 'NONE',  ( 33.78194858457152350, -281.0007626259030644, -253.8228568684648963 ) ) ;
#88024 = CARTESIAN_POINT ( 'NONE',  ( -34.93302407509652596, -293.0421440463298381, -345.6778165645779382 ) ) ;
#88026 = CARTESIAN_POINT ( 'NONE',  ( 19.53111540539381608, -294.4252453836471091, -322.3471917137055698 ) ) ;
#88027 = ADVANCED_FACE ( 'NONE', ( #76671 ), #44610, .F. ) ;
#88028 = CARTESIAN_POINT ( 'NONE',  ( -83.36039144849959825, -281.4221282135485467, -211.0730805485362396 ) ) ;
#88029 = CARTESIAN_POINT ( 'NONE',  ( -38.35754238776203806, -294.1239411967820843, -343.5893674043023793 ) ) ;
#88030 = CIRCLE ( 'NONE', #18491, 4.499999999999990230 ) ;
#88031 = CARTESIAN_POINT ( 'NONE',  ( -36.88564129984808204, -296.0577044583180850, -195.3612647501385595 ) ) ;
#88032 = ORIENTED_EDGE ( 'NONE', *, *, #21756, .T. ) ;
#88033 = FACE_OUTER_BOUND ( 'NONE', #13375, .T. ) ;
#88035 = CARTESIAN_POINT ( 'NONE',  ( 14.45878185895233692, -282.7644997205793516, -216.5438152142829438 ) ) ;
#88034 = AXIS2_PLACEMENT_3D ( 'NONE', #5144, #49159, #14123 ) ;
#88036 = CARTESIAN_POINT ( 'NONE',  ( -93.13344359532653982, -295.3897704676152216, -317.5532668033202413 ) ) ;
#88037 = CARTESIAN_POINT ( 'NONE',  ( 2.197429475817664013, -229.5268262511776527, 22.50000000000000000 ) ) ;
#88038 = CARTESIAN_POINT ( 'NONE',  ( -69.91165696735023971, -280.9809262143061233, -337.9199732462171255 ) ) ;
#88039 = CARTESIAN_POINT ( 'NONE',  ( -13.10371249219858925, -273.5564123017754810, -197.4455587681865723 ) ) ;
#88040=STYLED_ITEM('',(#93738),#27724);
#88041 = CARTESIAN_POINT ( 'NONE',  ( -94.10562526046624043, -289.7362468628363672, -316.2616278719199272 ) ) ;
#88042 = CIRCLE ( 'NONE', #66838, 4.999999999999993783 ) ;
#88043 = CARTESIAN_POINT ( 'NONE',  ( -67.60858399614113523, -281.1678115959601882, -203.1564324437556763 ) ) ;
#88044 = CARTESIAN_POINT ( 'NONE',  ( -74.69570621828421508, -275.1466549277791955, -206.6535127026903353 ) ) ;
#88045 = CARTESIAN_POINT ( 'NONE',  ( -3.232469343243530080, -284.2094172916588946, -338.5151890446434209 ) ) ;
#88046 = CARTESIAN_POINT ( 'NONE',  ( -72.30542045162339093, -278.3734765558481286, -205.8268730681629108 ) ) ;
#88047 = CARTESIAN_POINT ( 'NONE',  ( 8.831183281731817658, -278.4196222314847660, -329.5294736393781818 ) ) ;
#88048 = EDGE_LOOP ( 'NONE', ( #63562, #57512, #26953, #6577 ) ) ;
#88049 = CARTESIAN_POINT ( 'NONE',  ( -34.10107067241351331, -273.9251751815434659, -193.4293408988897340 ) ) ;
#88050 = CARTESIAN_POINT ( 'NONE',  ( -5.446378197264083454, -294.3951994222476856, -203.0863604086629834 ) ) ;
#88051 = DIRECTION ( 'NONE',  ( 0.000000000000000000, 0.000000000000000000, 1.000000000000000000 ) ) ;
#88052 = CARTESIAN_POINT ( 'NONE',  ( 11.63197158325052172, -285.8906705383787994, 57.50000000000000000 ) ) ;
#88053 = CARTESIAN_POINT ( 'NONE',  ( -41.89539172292137437, -293.2484082096262910, -346.0405049937615445 ) ) ;
#88054 = CARTESIAN_POINT ( 'NONE',  ( -97.89067727954578402, -272.6287297398000078, -229.3831018076481598 ) ) ;
#88055 = DIRECTION ( 'NONE',  ( 0.000000000000000000, 0.000000000000000000, -1.000000000000000000 ) ) ;
#88056 = CARTESIAN_POINT ( 'NONE',  ( 16.98228717613609362, -294.3288933417796329, -216.6993093001383386 ) ) ;
#88057 = CARTESIAN_POINT ( 'NONE',  ( -4.829096099716510437, -282.9805209788416391, -202.7746430608542312 ) ) ;
#88058 = CARTESIAN_POINT ( 'NONE',  ( -3.794977272724276318, -288.4959754479165213, -203.4683245288587443 ) ) ;
#88059 = CARTESIAN_POINT ( 'NONE',  ( -13.21789937088826150, -274.7380510615967637, -341.2539243625914764 ) ) ;
#88060 = CARTESIAN_POINT ( 'NONE',  ( 29.33093044711479180, -277.9138853626754440, -303.5844146361203002 ) ) ;
#88061 = CARTESIAN_POINT ( 'NONE',  ( 36.73076434529306766, -291.5299507287904817, -262.4731581731098231 ) ) ;
#88062 = CARTESIAN_POINT ( 'NONE',  ( -110.5438516166715459, -280.6617613517578889, -250.7725339633181534 ) ) ;
#88063 = ORIENTED_EDGE ( 'NONE', *, *, #26993, .F. ) ;
#88064 = CARTESIAN_POINT ( 'NONE',  ( -40.23944534481395152, -282.7562954043267496, -343.3247428890520041 ) ) ;
#88065 = CARTESIAN_POINT ( 'NONE',  ( -64.64518714521443599, -280.7836883358521618, -198.6391335974570609 ) ) ;
#88066 =( BOUNDED_SURFACE ( )  B_SPLINE_SURFACE ( 3, 2, ( 
 ( #59608, #81347, #2760 ),
 ( #16497, #24525, #31641 ),
 ( #45349, #67170, #2303 ),
 ( #60531, #89369, #17442 ) ),
 .UNSPECIFIED., .F., .F., .F. ) 
 B_SPLINE_SURFACE_WITH_KNOTS ( ( 4, 4 ),
 ( 3, 3 ),
 ( 0.000000000000000000, 0.0009404805950308383440 ),
 ( 0.000000000000000000, 1.000000000000000000 ),
 .UNSPECIFIED. ) 
 GEOMETRIC_REPRESENTATION_ITEM ( )  RATIONAL_B_SPLINE_SURFACE ( (
 ( 1.000000000000000000, 0.7071067811865475727, 1.000000000000000000),
 ( 1.000000000000000000, 0.6851250445827049562, 1.000000000000000000),
 ( 1.000000000000000000, 0.6575897825470939928, 1.000000000000000000),
 ( 1.000000000000000000, 0.6287211027133905450, 1.000000000000000000) ) ) 
 REPRESENTATION_ITEM ( '' )  SURFACE ( )  );
#88067 = CARTESIAN_POINT ( 'NONE',  ( -47.22043294360042864, -281.9699420839394293, -346.3243943458421654 ) ) ;
#88068 = CARTESIAN_POINT ( 'NONE',  ( 20.65039207745597594, -277.1753149104871454, -320.6775120918483140 ) ) ;
#88069 = DIRECTION ( 'NONE',  ( 1.000000000000000000, 0.000000000000000000, 0.000000000000000000 ) ) ;
#88070 = CARTESIAN_POINT ( 'NONE',  ( 23.07194617520410063, -276.4442403298035060, -223.7254904445416344 ) ) ;
#88071 = CARTESIAN_POINT ( 'NONE',  ( -105.5795714935544112, -292.8376638359844719, -285.9686137636504668 ) ) ;
#88072 = ORIENTED_EDGE ( 'NONE', *, *, #72465, .T. ) ;
#88073 = ORIENTED_EDGE ( 'NONE', *, *, #90062, .T. ) ;
#88074 = CARTESIAN_POINT ( 'NONE',  ( -100.1356641409920059, -299.1065787196612291, -229.2558880299098689 ) ) ;
#88075 = CARTESIAN_POINT ( 'NONE',  ( -72.78841978645263566, -292.6509560028214878, -206.1343243186854863 ) ) ;
#88076 = CARTESIAN_POINT ( 'NONE',  ( -73.66393723770808322, -275.5568203661385382, -335.5873427672989351 ) ) ;
#88077 = CARTESIAN_POINT ( 'NONE',  ( -8.595433050809544895, -290.4412316765368587, -340.7145625764255215 ) ) ;
#88078 = CARTESIAN_POINT ( 'NONE',  ( -85.99068765710171647, -290.7055391803672819, -215.7295545633712663 ) ) ;
#88079 = CARTESIAN_POINT ( 'NONE',  ( 39.64079791239883832, -287.0747689296518388, -271.5565952383105355 ) ) ;
#88080 = DIRECTION ( 'NONE',  ( 0.000000000000000000, 0.000000000000000000, -1.000000000000000000 ) ) ;
#88081 = CARTESIAN_POINT ( 'NONE',  ( -53.88864543901411253, -281.6678207017998261, -342.3348377082150478 ) ) ;
#88082 = CARTESIAN_POINT ( 'NONE',  ( -72.93055549288244777, -291.3894515667271321, -335.5094015790838284 ) ) ;
#88083 = CARTESIAN_POINT ( 'NONE',  ( -102.3922678062164522, -282.5632985167258653, -305.0982545796017575 ) ) ;
#88084 = CARTESIAN_POINT ( 'NONE',  ( -39.73395180052004605, -281.3366925667725695, -196.8943062102937631 ) ) ;
#88085 = CARTESIAN_POINT ( 'NONE',  ( -106.2968676754041439, -291.0575067044758839, -304.2162379658692544 ) ) ;
#88086 = CARTESIAN_POINT ( 'NONE',  ( -110.4534897544638881, -279.0407669068110863, -270.6445443924029064 ) ) ;
#88087 = CARTESIAN_POINT ( 'NONE',  ( -19.46446794593252960, -291.0719460744298317, -195.8189035277109724 ) ) ;
#88088 = CARTESIAN_POINT ( 'NONE',  ( 34.69927799345143171, -288.0163770757100679, -243.6355442475868074 ) ) ;
#88089 = CARTESIAN_POINT ( 'NONE',  ( 38.61525139615243063, -288.2018822288491151, -282.9354233038869211 ) ) ;
#88090 = CARTESIAN_POINT ( 'NONE',  ( -39.97604399891438476, -286.1848131685628118, -197.4086660916569258 ) ) ;
#88091 = EDGE_LOOP ( 'NONE', ( #48960, #80585 ) ) ;
#88092 = FACE_OUTER_BOUND ( 'NONE', #23718, .T. ) ;
#88093 = CARTESIAN_POINT ( 'NONE',  ( 28.39203342393819440, -294.9150701284098659, -232.6864348158137261 ) ) ;
#88094 = CARTESIAN_POINT ( 'NONE',  ( -99.61691144699085498, -294.6435072871005900, -314.8924308792064721 ) ) ;
#88095 = CARTESIAN_POINT ( 'NONE',  ( 19.35616632030332696, -275.2653556777614767, -316.7355984258047670 ) ) ;
#88096 = CARTESIAN_POINT ( 'NONE',  ( -98.14825962218955624, -296.5302480525601254, -223.2667873263114302 ) ) ;
#88097 = CARTESIAN_POINT ( 'NONE',  ( 33.78080959018988239, -292.2850808385719574, -289.7040323429512227 ) ) ;
#88098 = CARTESIAN_POINT ( 'NONE',  ( -109.5858086981793633, -294.5827131127281291, -286.4472235874768558 ) ) ;
#88099 = AXIS2_PLACEMENT_3D ( 'NONE', #5813, #19083, #91494 ) ;
#88100 = CARTESIAN_POINT ( 'NONE',  ( -52.46650105825904120, -293.0593217127251364, -198.4871328024764523 ) ) ;
#88101 = CARTESIAN_POINT ( 'NONE',  ( 10.50361382554200063, -295.4525027874370267, -325.9043624448160585 ) ) ;
#88102 = DIRECTION ( 'NONE',  ( 1.000000000000000000, 0.000000000000000000, -0.000000000000000000 ) ) ;
#88103 = AXIS2_PLACEMENT_3D ( 'NONE', #70892, #64748, #80656 ) ;
#88104 = CARTESIAN_POINT ( 'NONE',  ( 32.73293801919767532, -291.9049436001784557, -297.5562188825014687 ) ) ;
#88105 = CARTESIAN_POINT ( 'NONE',  ( -96.75263409797366876, -297.9249393878914702, -316.1566897943395702 ) ) ;
#88106 = CARTESIAN_POINT ( 'NONE',  ( -110.3562042000021108, -291.4105568231588563, -276.6620431624808703 ) ) ;
#88108 = CARTESIAN_POINT ( 'NONE',  ( -42.38694992656297700, -295.4508147315298174, -343.2077578588712186 ) ) ;
#88107 =( GEOMETRIC_REPRESENTATION_CONTEXT ( 3 ) GLOBAL_UNCERTAINTY_ASSIGNED_CONTEXT ( ( #83164 ) ) GLOBAL_UNIT_ASSIGNED_CONTEXT ( ( #18050, #39795, #31789 ) ) REPRESENTATION_CONTEXT ( 'NONE', 'WORKASPACE' ) );
#88109 = AXIS2_PLACEMENT_3D ( 'NONE', #56709, #76596, #85555 ) ;
#88110 = CARTESIAN_POINT ( 'NONE',  ( -79.28920299328233057, -279.5947256136594206, -333.0243484806517245 ) ) ;
#88111 = CARTESIAN_POINT ( 'NONE',  ( -111.9172554601288567, -277.4519923052437775, -253.2794078170714158 ) ) ;
#88112 = EDGE_LOOP ( 'NONE', ( #77510, #73574, #33963, #68149, #47955 ) ) ;
#88113 = CARTESIAN_POINT ( 'NONE',  ( -66.18128497136308397, -273.0330382519287582, -199.0616873903806265 ) ) ;
#88114 = CARTESIAN_POINT ( 'NONE',  ( 22.96444719138651891, -280.2309726238613052, -314.0233138409413982 ) ) ;
#88115 = CARTESIAN_POINT ( 'NONE',  ( -112.5133435743650097, -276.7943531801821564, -282.8376735028777489 ) ) ;
#88116 = CARTESIAN_POINT ( 'NONE',  ( -108.7986888273022004, -276.8544628302996671, -246.8738483912092363 ) ) ;
#88117 = CARTESIAN_POINT ( 'NONE',  ( -63.23765619511080871, -296.3925755081279476, -201.5276133702380434 ) ) ;
#88118 = DIRECTION ( 'NONE',  ( -0.000000000000000000, -1.000000000000000000, -0.000000000000000000 ) ) ;
#88119 = CARTESIAN_POINT ( 'NONE',  ( 194.2870706637141609, 27.28231030510911381, 14.58823529411774089 ) ) ;
#88120 = CARTESIAN_POINT ( 'NONE',  ( -111.3055743514985636, -288.7573173876669443, -255.8804036379154638 ) ) ;
#88121 = CARTESIAN_POINT ( 'NONE',  ( -114.2513007961944140, -290.5055026580545814, -274.0911749622030129 ) ) ;
#88122 = CARTESIAN_POINT ( 'NONE',  ( -4.647123075323000840, -276.4819619285366343, -202.6631852457198875 ) ) ;
#88123 = CARTESIAN_POINT ( 'NONE',  ( -76.13990737606391690, -295.5326814295020199, -206.3109919767010751 ) ) ;
#88124 = CARTESIAN_POINT ( 'NONE',  ( -63.86588771210455207, -282.5865781149620943, -342.4764859241964814 ) ) ;
#88125 = CARTESIAN_POINT ( 'NONE',  ( 0.000000000000000000, 0.000000000000000000, 25.50000000000000000 ) ) ;
#88126 = CARTESIAN_POINT ( 'NONE',  ( 37.14009450132499524, -279.6704666828625818, -279.5883913115331438 ) ) ;
#88127 = CIRCLE ( 'NONE', #41212, 2.336627660646517501 ) ;
#88128 = CARTESIAN_POINT ( 'NONE',  ( 203.5977283565847813, 62.01285785379744198, 7.000000000000000000 ) ) ;
#88129 = CARTESIAN_POINT ( 'NONE',  ( 15.17026737379739387, -291.6085045964363758, -219.0084496902107674 ) ) ;
#88130 = CARTESIAN_POINT ( 'NONE',  ( -109.5617619924906592, -282.9152455127450025, -253.1271530884613981 ) ) ;
#88131 = DIRECTION ( 'NONE',  ( 1.000000000000000000, 0.000000000000000000, 0.000000000000000000 ) ) ;
#88132 = CARTESIAN_POINT ( 'NONE',  ( 0.000000000000000000, 249.5000000000000568, -12.50000000000000000 ) ) ;
#88133 = CARTESIAN_POINT ( 'NONE',  ( 29.27433581912985971, -291.0959216691383631, -235.9038342759135674 ) ) ;
#88134 = CARTESIAN_POINT ( 'NONE',  ( -96.72473094528029947, -279.5445122500848925, -314.2011936995983206 ) ) ;
#88135 = CARTESIAN_POINT ( 'NONE',  ( 8.980949324553606061, -283.6372816363866605, -331.3711242534291728 ) ) ;
#88137 = CARTESIAN_POINT ( 'NONE',  ( -85.72614845339728618, -285.3604186175128916, -215.6314559081591256 ) ) ;
#88136 = CARTESIAN_POINT ( 'NONE',  ( -8.222485250906748533, -272.5102064271576410, -200.5819330462015841 ) ) ;
#88138 = CARTESIAN_POINT ( 'NONE',  ( 34.69443761783420399, -276.7798228385889843, -255.2607302509971134 ) ) ;
#88139 = CARTESIAN_POINT ( 'NONE',  ( -69.31276912897160969, -278.2866883597445167, -336.1811584178219618 ) ) ;
#88140 = ADVANCED_FACE ( 'NONE', ( #11798 ), #53957, .T. ) ;
#88141 = CARTESIAN_POINT ( 'NONE',  ( -90.98498959451472956, -285.8140612892287322, -322.7767467906639354 ) ) ;
#88142 = ADVANCED_BREP_SHAPE_REPRESENTATION ( '', ( #27246, #18940 ), #770 ) ;
#88143 = VERTEX_POINT ( 'NONE', #40649 ) ;
#88144 = DIRECTION ( 'NONE',  ( -0.6056179655966479336, 0.7957555401921982963, 3.708340515370333519E-17 ) ) ;
#88145 = CARTESIAN_POINT ( 'NONE',  ( -113.6529222429083887, -296.2520716419392102, -281.0277591448146381 ) ) ;
#88146 = CARTESIAN_POINT ( 'NONE',  ( 7.904344611423861799, -288.6532118800534477, -210.9271306806662380 ) ) ;
#88147 = CARTESIAN_POINT ( 'NONE',  ( 157.5411741086738004, 275.0000000000000568, 16.22085278731064761 ) ) ;
#88148 = CARTESIAN_POINT ( 'NONE',  ( 40.65961533371913106, -284.8380690714489560, -252.5904736702033802 ) ) ;
#88149 = CARTESIAN_POINT ( 'NONE',  ( -69.81891132980183556, -278.5548227276381681, -200.8721641875049215 ) ) ;
#88150 = CARTESIAN_POINT ( 'NONE',  ( -55.97325112671786229, -290.2161168959786437, -196.4196302003576307 ) ) ;
#88151 = CARTESIAN_POINT ( 'NONE',  ( -109.6126816646767423, -286.2605644282862727, -255.9523365685023464 ) ) ;
#88152 = CARTESIAN_POINT ( 'NONE',  ( -77.38873885318605517, -281.2674942412294854, -208.0568696274944216 ) ) ;
#88153 = CARTESIAN_POINT ( 'NONE',  ( 38.76601831549815813, -288.8845994184816277, -262.9958655472564146 ) ) ;
#88154 = CARTESIAN_POINT ( 'NONE',  ( -10.22964350021393010, -284.6985922702266976, -340.3442601395365728 ) ) ;
#88155 = CARTESIAN_POINT ( 'NONE',  ( -28.59892865729863942, -277.1109960324056374, -346.9167453941711869 ) ) ;
#88156 = CARTESIAN_POINT ( 'NONE',  ( -108.9434146600346480, -270.8350489116736526, -248.4301281355177196 ) ) ;
#88157 = CARTESIAN_POINT ( 'NONE',  ( -22.56410032880094718, -280.0694853920627452, -194.7382011148541494 ) ) ;
#88159 = CARTESIAN_POINT ( 'NONE',  ( -47.49284973818976141, -299.8424327094240311, -196.5642795176598838 ) ) ;
#88158 = VECTOR ( 'NONE', #56850, 1000.000000000000000 ) ;
#88160 = CARTESIAN_POINT ( 'NONE',  ( 165.6062301568830435, 2.982529536179759688, 9.000000000000001776 ) ) ;
#88161 = CARTESIAN_POINT ( 'NONE',  ( 35.78497577281001440, -278.2662352645559167, -287.0191576251351080 ) ) ;
#88162 = CARTESIAN_POINT ( 'NONE',  ( 13.30597666025241388, -272.9885491447457753, -213.6446295069706025 ) ) ;
#88164 = CIRCLE ( 'NONE', #68525, 1.499999999999998446 ) ;
#88163 = CARTESIAN_POINT ( 'NONE',  ( 183.0442525570908288, 264.6571197653884155, -7.500000000000000000 ) ) ;
#88165 = CARTESIAN_POINT ( 'NONE',  ( -110.2195865913370199, -278.1280386710591870, -265.1840429234287058 ) ) ;
#88166 = AXIS2_PLACEMENT_3D ( 'NONE', #10891, #47808, #55877 ) ;
#88167 = CARTESIAN_POINT ( 'NONE',  ( 36.85797481993009228, -276.9966972091705770, -289.3983698169153627 ) ) ;
#88168 = CARTESIAN_POINT ( 'NONE',  ( 39.40591682538859430, -280.5697338323745385, -267.0794283067742185 ) ) ;
#88169 = CARTESIAN_POINT ( 'NONE',  ( -71.62246852129017327, -291.2716265218506919, -335.9711885992347788 ) ) ;
#88170 = CARTESIAN_POINT ( 'NONE',  ( -29.17167597755265973, -299.6727988630092341, -194.0523781336487446 ) ) ;
#88171 = CARTESIAN_POINT ( 'NONE',  ( -80.41450008066351529, -298.6880337901230291, -206.9511208581930362 ) ) ;
#88172 = CARTESIAN_POINT ( 'NONE',  ( -6.538296825703257653, -294.4577616521149821, -202.1615668486769550 ) ) ;
#88173 = CARTESIAN_POINT ( 'NONE',  ( 6.649781761084901710, -280.4522460333596996, -330.8985274488123878 ) ) ;
#88174 = AXIS2_PLACEMENT_3D ( 'NONE', #1273, #52846, #81723 ) ;
#88175 = CARTESIAN_POINT ( 'NONE',  ( 31.67866088699393501, -283.8384726241913540, -298.2448759950679573 ) ) ;
#88176 = CARTESIAN_POINT ( 'NONE',  ( -75.08374230413420491, -271.5672118961417709, -205.9010585980348935 ) ) ;
#88177 = CARTESIAN_POINT ( 'NONE',  ( -109.2293572722669097, -286.4744047880150788, -245.0904795891546541 ) ) ;
#88178 = CARTESIAN_POINT ( 'NONE',  ( -73.71021151142527117, -288.4674053433036534, -334.0274374160937896 ) ) ;
#88179 = CARTESIAN_POINT ( 'NONE',  ( 162.5749643528775152, 219.4908287816205927, -205.1158602168718232 ) ) ;
#88180 = ORIENTED_EDGE ( 'NONE', *, *, #20867, .T. ) ;
#88181 = CARTESIAN_POINT ( 'NONE',  ( -65.24886689772108639, -287.9844206219984812, -341.5492815931301038 ) ) ;
#88182 = CARTESIAN_POINT ( 'NONE',  ( 33.72068467352190169, -287.4404327710979032, -287.1606701546808722 ) ) ;
#88183 = ORIENTED_EDGE ( 'NONE', *, *, #15154, .T. ) ;
#88184 = CARTESIAN_POINT ( 'NONE',  ( -113.1838493221684701, -285.7790947585094727, -258.6324309697760100 ) ) ;
#88185 = TOROIDAL_SURFACE ( 'NONE', #70111, 4.500000000000002665, 0.5000000000000000000 ) ;
#88186 = CARTESIAN_POINT ( 'NONE',  ( 31.13667355107491019, -275.5474503757438356, -245.0076206895940061 ) ) ;
#88187 = CARTESIAN_POINT ( 'NONE',  ( 37.76200922093805445, -292.2767734184265009, -254.7749289271553721 ) ) ;
#88188 = CARTESIAN_POINT ( 'NONE',  ( 37.88321771028709861, -282.0029843431165659, -254.3443301455328651 ) ) ;
#88189 = CARTESIAN_POINT ( 'NONE',  ( 22.32098383612148496, -282.4293201077407502, -222.7685966366165928 ) ) ;
#88190 = CARTESIAN_POINT ( 'NONE',  ( -102.8978494873622935, -284.3579021650200502, -310.7112799730288657 ) ) ;
#88191 = CARTESIAN_POINT ( 'NONE',  ( 7.151849590232073339, -281.0104430209759698, -212.3971315885685840 ) ) ;
#88192 = CARTESIAN_POINT ( 'NONE',  ( 35.77081079830085031, -273.2666405000204009, -287.0812184334320705 ) ) ;
#88193 = CARTESIAN_POINT ( 'NONE',  ( -109.8947478827530375, -267.1952134479645338, -307.0630218189940024 ) ) ;
#88194 = VERTEX_POINT ( 'NONE', #25083 ) ;
#88195 = CARTESIAN_POINT ( 'NONE',  ( -62.37982150143177051, -279.3786325072121031, -340.9365589617439127 ) ) ;
#88196 = CARTESIAN_POINT ( 'NONE',  ( -90.89323871145485612, -229.7990343503469433, -347.2845633163808543 ) ) ;
#88197 = VECTOR ( 'NONE', #76145, 1000.000000000000000 ) ;
#88198 = CARTESIAN_POINT ( 'NONE',  ( -75.25642810133714988, -296.8812112239102134, -207.8015043505610322 ) ) ;
#88199 = CARTESIAN_POINT ( 'NONE',  ( 24.76848499883414689, -292.4564789224114065, -224.9534996033449090 ) ) ;
#88200 = CARTESIAN_POINT ( 'NONE',  ( -21.04059066054967531, -109.3119883923508127, -359.1154128302432582 ) ) ;
#88201 = EDGE_CURVE ( 'NONE', #47196, #38497, #17977, .T. ) ;
#88203 = CARTESIAN_POINT ( 'NONE',  ( -64.13008383981188842, -287.8072636360128627, -339.1823409630512174 ) ) ;
#88202 = CARTESIAN_POINT ( 'NONE',  ( -35.47146142439535765, -296.6498690183287863, -193.9507853632559886 ) ) ;
#88204 = CARTESIAN_POINT ( 'NONE',  ( -61.39129890479637908, -297.2281266454388629, -340.6472254639340917 ) ) ;
#88205 = EDGE_CURVE ( 'NONE', #47327, #33195, #93023, .T. ) ;
#88206 = CARTESIAN_POINT ( 'NONE',  ( -33.22768840996732820, -287.4200752050302867, -196.9330459988719610 ) ) ;
#88207 = ORIENTED_EDGE ( 'NONE', *, *, #28072, .T. ) ;
#88208 = CARTESIAN_POINT ( 'NONE',  ( 13.24979206168188739, -295.3064766873507665, -328.1665279788851421 ) ) ;
#88209 = CARTESIAN_POINT ( 'NONE',  ( -4.572576537063657298, -286.9884061336192644, -205.0604826033140569 ) ) ;
#88210 = CARTESIAN_POINT ( 'NONE',  ( 30.36740316544978313, -297.6770476619486772, -193.7716728435736115 ) ) ;
#88211 = AXIS2_PLACEMENT_3D ( 'NONE', #21817, #8054, #15169 ) ;
#88212 = CARTESIAN_POINT ( 'NONE',  ( 17.36743678325598950, -293.6117195791124459, -216.3318816005890426 ) ) ;
#88213 = CARTESIAN_POINT ( 'NONE',  ( 24.76107106019305704, -293.4410141854605740, -224.9433602868196260 ) ) ;
#88214 = CARTESIAN_POINT ( 'NONE',  ( -105.7113890414355666, -291.0618688374010503, -244.6327995941137488 ) ) ;
#88215 = ORIENTED_EDGE ( 'NONE', *, *, #53722, .T. ) ;
#88216 = CARTESIAN_POINT ( 'NONE',  ( 157.4851178187871312, 14.99999999999999645, 9.000000000000000000 ) ) ;
#88217 = CARTESIAN_POINT ( 'NONE',  ( -94.02277199248693762, -275.1617008243414944, -220.3954268340792453 ) ) ;
#88218 = CARTESIAN_POINT ( 'NONE',  ( 38.53300312435957409, -274.2146111393961974, -259.8236550624438337 ) ) ;
#88219 = EDGE_LOOP ( 'NONE', ( #52109, #88996, #442, #40316 ) ) ;
#88220 = CARTESIAN_POINT ( 'NONE',  ( -1.501958393290475868, -276.0975271653778691, -338.4422447049026346 ) ) ;
#88221 = CARTESIAN_POINT ( 'NONE',  ( -37.80765668215608599, -296.5260879245860224, -196.6692552082457723 ) ) ;
#88222 = CARTESIAN_POINT ( 'NONE',  ( -90.37227467274794890, -281.1526252709547293, -218.3399634613344062 ) ) ;
#88223 = CARTESIAN_POINT ( 'NONE',  ( 25.00918386538674554, -274.2413560981182172, -310.7452179939623989 ) ) ;
#88224 = CARTESIAN_POINT ( 'NONE',  ( -104.6690256188526433, -274.0214637798055151, -241.2279811572928452 ) ) ;
#88225 = CARTESIAN_POINT ( 'NONE',  ( -99.48645739836602786, -274.0264841938550830, -231.6127297359945487 ) ) ;
#88226 = CARTESIAN_POINT ( 'NONE',  ( -103.3603874442145667, -274.8086417971169340, -232.6322462306227692 ) ) ;
#88227 = CARTESIAN_POINT ( 'NONE',  ( -2.049027641403455391, -272.5372473450477173, -203.7815860377621675 ) ) ;
#88228 = CARTESIAN_POINT ( 'NONE',  ( -80.20785339970126415, -296.3015626653618142, -329.5758591503414436 ) ) ;
#88229 = CARTESIAN_POINT ( 'NONE',  ( 36.29751644544722211, -292.1323700913396237, -270.7812561167751824 ) ) ;
#88230 = DIRECTION ( 'NONE',  ( -0.000000000000000000, 1.000000000000000000, -0.000000000000000000 ) ) ;
#88231 = CARTESIAN_POINT ( 'NONE',  ( 8.209680046817211974, -276.9402793762799320, -332.4319108869291313 ) ) ;
#88232 = CARTESIAN_POINT ( 'NONE',  ( 7.329238533290764579, -274.8475358915682705, -212.6245849761958766 ) ) ;
#88233 = CARTESIAN_POINT ( 'NONE',  ( -111.2404638142247961, -283.4888356708507331, -250.3563378992984667 ) ) ;
#88234 = CARTESIAN_POINT ( 'NONE',  ( -109.0431402898783375, -298.2614116146913830, -292.9636715070546416 ) ) ;
#88235 = DIRECTION ( 'NONE',  ( -0.000000000000000000, 1.000000000000000000, -0.000000000000000000 ) ) ;
#88236 = VECTOR ( 'NONE', #56619, 1000.000000000000000 ) ;
#88237 = CARTESIAN_POINT ( 'NONE',  ( -74.79400943084030473, -284.7368200349844756, -207.5126792201695309 ) ) ;
#88238 = CARTESIAN_POINT ( 'NONE',  ( -67.17764200168213051, -281.4422543912177730, -339.3527479199831873 ) ) ;
#88239 = CARTESIAN_POINT ( 'NONE',  ( -76.91632690004914252, -275.8295661552189699, -332.9659714203622798 ) ) ;
#88240 = CARTESIAN_POINT ( 'NONE',  ( -37.83175530948163612, -275.6330981550337924, -343.9612703428771852 ) ) ;
#88241 = CARTESIAN_POINT ( 'NONE',  ( -75.70218864341489962, -281.5404255335116659, -205.8988260176669485 ) ) ;
#88242 = CARTESIAN_POINT ( 'NONE',  ( 32.43453334276953370, -276.4547975907180444, -247.4291587977991469 ) ) ;
#88243 = DIRECTION ( 'NONE',  ( -0.000000000000000000, -1.000000000000000000, -0.000000000000000000 ) ) ;
#88244 = CARTESIAN_POINT ( 'NONE',  ( 17.52784463452914565, -273.2197997895094659, -217.4102774602705210 ) ) ;
#88245 = AXIS2_PLACEMENT_3D ( 'NONE', #59961, #23947, #45703 ) ;
#88246 = CARTESIAN_POINT ( 'NONE',  ( -14.80236189110495992, -282.3435414651202109, -198.5987684119311041 ) ) ;
#88247 = CARTESIAN_POINT ( 'NONE',  ( 156.2461366866179731, 19.34073763602959772, -8.651974842892217410 ) ) ;
#88248 = CARTESIAN_POINT ( 'NONE',  ( -29.63459085964426265, -288.0691856621139664, -195.1952037397211939 ) ) ;
#88249 = AXIS2_PLACEMENT_3D ( 'NONE', #68229, #9985, #30856 ) ;
#88250 = CARTESIAN_POINT ( 'NONE',  ( 154.0561329571298756, 19.33057573605838186, -12.42898486165725203 ) ) ;
#88251 = CARTESIAN_POINT ( 'NONE',  ( -100.6896029239377839, -288.0107624497654797, -310.6061220982144278 ) ) ;
#88252 = PLANE ( 'NONE',  #49740 ) ;
#88253 = CARTESIAN_POINT ( 'NONE',  ( -110.3739708836756108, -271.3446501961809645, -262.1433989632457724 ) ) ;
#88254 = CARTESIAN_POINT ( 'NONE',  ( -91.64688067914313763, -289.4076309777720439, -219.7279759228227078 ) ) ;
#88255 = CARTESIAN_POINT ( 'NONE',  ( -92.83893396777953910, -239.1568807800618686, -338.3566629249717153 ) ) ;
#88256 = CARTESIAN_POINT ( 'NONE',  ( 196.0143093133017658, 19.33012701892200624, -12.49999999999967315 ) ) ;
#88257 = CARTESIAN_POINT ( 'NONE',  ( 5.154996196520969853, -286.9685562595444139, -333.7388629163718861 ) ) ;
#88258 = CARTESIAN_POINT ( 'NONE',  ( -98.51493802057321147, -283.3998819051982423, -225.1989825478488285 ) ) ;
#88259 = CARTESIAN_POINT ( 'NONE',  ( -62.80072885097423807, -291.7112716084420754, -201.9444690110785530 ) ) ;
#88260 = AXIS2_PLACEMENT_3D ( 'NONE', #80003, #29362, #49719 ) ;
#88261 = AXIS2_PLACEMENT_3D ( 'NONE', #35347, #34876, #63788 ) ;
#88262 = CARTESIAN_POINT ( 'NONE',  ( 33.67749910263282942, -282.7242310013076008, -251.0347712590880747 ) ) ;
#88263 = CARTESIAN_POINT ( 'NONE',  ( -26.70922734010413180, -283.7164235165128048, -342.7972835085058136 ) ) ;
#88264 = CARTESIAN_POINT ( 'NONE',  ( -10.13318631859390706, -290.6785981404049153, -340.6327593413762997 ) ) ;
#88265 = CARTESIAN_POINT ( 'NONE',  ( -108.0597576528298731, -273.2744170289830095, -239.8174048061563894 ) ) ;
#88266 = AXIS2_PLACEMENT_3D ( 'NONE', #26556, #34133, #11407 ) ;
#88267 = CARTESIAN_POINT ( 'NONE',  ( -62.31130467539001927, -287.4541316290829513, -341.7314815628662359 ) ) ;
#88268 = CARTESIAN_POINT ( 'NONE',  ( 28.50254742679922515, -275.0299209542463927, -230.3400805502313915 ) ) ;
#88269 = CARTESIAN_POINT ( 'NONE',  ( -65.98082745313099906, -293.6554764907412505, -201.4151042775787630 ) ) ;
#88270 = CARTESIAN_POINT ( 'NONE',  ( 165.2494399300530290, -11.64849832608277325, 13.00000000000000178 ) ) ;
#88271 = CARTESIAN_POINT ( 'NONE',  ( 31.98288692825981272, -278.4805209788417528, -303.7098442033569654 ) ) ;
#88272 = CARTESIAN_POINT ( 'NONE',  ( -90.06178684402692625, -275.7943570001564808, -324.0122077690716083 ) ) ;
#88273 = DIRECTION ( 'NONE',  ( 0.000000000000000000, 0.000000000000000000, 1.000000000000000000 ) ) ;
#88274 = CARTESIAN_POINT ( 'NONE',  ( -70.36372970944867689, -296.0240052075956214, -201.6880811971482501 ) ) ;
#88275 = CARTESIAN_POINT ( 'NONE',  ( 20.76760079737980647, -274.2776399992562233, -225.9873618624560550 ) ) ;
#88276 = CARTESIAN_POINT ( 'NONE',  ( -84.28544903622223217, -292.9126491713624318, -213.5544969866777478 ) ) ;
#88277 = TOROIDAL_SURFACE ( 'NONE', #38396, 24.50000000000000355, 0.5000000000000000000 ) ;
#88278 = CARTESIAN_POINT ( 'NONE',  ( -55.08091300432091941, -292.7596190403543801, -199.3067108432525743 ) ) ;
#88279 = CARTESIAN_POINT ( 'NONE',  ( -82.10906341364054128, -287.1921819900448440, -211.4216813088281697 ) ) ;
#88280 = CARTESIAN_POINT ( 'NONE',  ( 32.77644349308054217, -294.5874783100049399, -239.9958050992020162 ) ) ;
#88281 = CARTESIAN_POINT ( 'NONE',  ( 22.79450742641722272, -295.5040708867605304, -317.6783876256492931 ) ) ;
#88282 = CARTESIAN_POINT ( 'NONE',  ( 33.77494002578152532, -293.6034601427674033, -286.8911158114495947 ) ) ;
#88283 = CARTESIAN_POINT ( 'NONE',  ( 36.49503310685380342, -289.7212613075241734, -283.5192894324907797 ) ) ;
#88284 = CARTESIAN_POINT ( 'NONE',  ( 37.98422382833608424, -281.5183296025614936, -254.3291661651592790 ) ) ;
#88285 = CARTESIAN_POINT ( 'NONE',  ( 18.09568570091506245, -296.8208154810340034, -194.8190760047378944 ) ) ;
#88286 = CARTESIAN_POINT ( 'NONE',  ( -112.3592484580582038, -284.6025850455986870, -253.0011799902360110 ) ) ;
#88287 = CARTESIAN_POINT ( 'NONE',  ( 16.80804729660922447, -278.2562762511470851, -321.7386583726605522 ) ) ;
#88288 = CARTESIAN_POINT ( 'NONE',  ( -109.3721152509106815, -283.1621050999826252, -284.4589831772510706 ) ) ;
#88289 = CARTESIAN_POINT ( 'NONE',  ( 17.17313334427597482, -286.2742332373839531, -321.8696957180593472 ) ) ;
#88290 = CARTESIAN_POINT ( 'NONE',  ( -50.69822842785222150, -278.0228707726343487, -195.7829131917748384 ) ) ;
#88291 = CARTESIAN_POINT ( 'NONE',  ( -113.2098679957031493, -271.2709011634024137, -296.4525692007673570 ) ) ;
#88292 = CARTESIAN_POINT ( 'NONE',  ( -108.0866798844073884, -284.3005441183248649, -252.1090966943046965 ) ) ;
#88293 = CARTESIAN_POINT ( 'NONE',  ( 39.22341567150652963, -282.7874802799650524, -272.7677255736381312 ) ) ;
#88294 = CARTESIAN_POINT ( 'NONE',  ( -17.79583782615364385, -287.8647894742294397, -344.5957425130280285 ) ) ;
#88295 = CARTESIAN_POINT ( 'NONE',  ( -73.69704314321123206, -279.1265534951251084, -337.3440848844318225 ) ) ;
#88296 = CARTESIAN_POINT ( 'NONE',  ( -67.49870513076889722, -278.7547398457653571, -340.6736582788987562 ) ) ;
#88297 = CARTESIAN_POINT ( 'NONE',  ( -81.28618619858487193, -279.2693462062475760, -212.0062902534424722 ) ) ;
#88298 = CARTESIAN_POINT ( 'NONE',  ( -24.33404948908517795, -276.1987813615330651, -196.8056639094921820 ) ) ;
#88299 = CARTESIAN_POINT ( 'NONE',  ( 37.27791870291623866, -285.6330496396946046, -276.6603946458873224 ) ) ;
#88300 = CARTESIAN_POINT ( 'NONE',  ( -70.27467607839722064, -291.0789694156782161, -339.0912397889829890 ) ) ;
#88301 = CARTESIAN_POINT ( 'NONE',  ( -5.419282164645363942, -293.5423160424007278, -336.3688133059591792 ) ) ;
#88302 = ORIENTED_EDGE ( 'NONE', *, *, #17026, .F. ) ;
#88303 = CARTESIAN_POINT ( 'NONE',  ( -45.09719836104773094, -294.8196469527659929, -343.0197338190831147 ) ) ;
#88304 = CARTESIAN_POINT ( 'NONE',  ( -111.6191986383296495, -291.3913850031715924, -289.5014578736276576 ) ) ;
#88305 = CARTESIAN_POINT ( 'NONE',  ( -38.36360349920153112, -280.6904267470862919, -197.2539093970831914 ) ) ;
#88306 = CARTESIAN_POINT ( 'NONE',  ( 75.83355947227427407, -298.3581913397087533, -193.6903554288949749 ) ) ;
#88307 = CARTESIAN_POINT ( 'NONE',  ( 19.55442187814812272, -288.9077138713660702, -322.1121951704050730 ) ) ;
#88308 = CARTESIAN_POINT ( 'NONE',  ( -62.75266672728255202, -289.7072037028835894, -343.0812803795569721 ) ) ;
#88309 = CARTESIAN_POINT ( 'NONE',  ( -73.56980829239275010, -285.8904698062691523, -206.9462098343767593 ) ) ;
#88310 = CARTESIAN_POINT ( 'NONE',  ( 64.47034098757669085, 48.08436262820399776, -318.7852478018613169 ) ) ;
#88311 = CIRCLE ( 'NONE', #44452, 4.999999999999990230 ) ;
#88312 = CARTESIAN_POINT ( 'NONE',  ( 23.85667543695174686, -22.61630356684642962, -343.2597395675320513 ) ) ;
#88313 = CARTESIAN_POINT ( 'NONE',  ( -39.01470583219347077, -140.0999525806348345, -360.8708370586243177 ) ) ;
#88314 = CARTESIAN_POINT ( 'NONE',  ( -32.41988592551756199, -276.1858179835649025, -343.4069310343268739 ) ) ;
#88315 = CARTESIAN_POINT ( 'NONE',  ( -64.46022434401164958, -276.3348179571497099, -338.5238552467184832 ) ) ;
#88316 = CARTESIAN_POINT ( 'NONE',  ( -110.0804957009435014, -272.5366084470006740, -245.1656439823766505 ) ) ;
#88317 = CARTESIAN_POINT ( 'NONE',  ( -11.02755183398383210, -93.07797461907387060, -357.3970400885787058 ) ) ;
#88318 = EDGE_CURVE ( 'NONE', #74853, #49791, #36658, .T. ) ;
#88319 = CARTESIAN_POINT ( 'NONE',  ( -41.37530129399917200, -275.7867418359247722, -346.7746893807156425 ) ) ;
#88320 = AXIS2_PLACEMENT_3D ( 'NONE', #22245, #42129, #42605 ) ;
#88321 = CARTESIAN_POINT ( 'NONE',  ( -36.26601005852802473, -296.7990116537307586, -346.3531046861765503 ) ) ;
#88322 = ORIENTED_EDGE ( 'NONE', *, *, #75906, .T. ) ;
#88323 = CARTESIAN_POINT ( 'NONE',  ( -81.77143365266174158, -291.9209641106515392, -212.2972044397519369 ) ) ;
#88324 = CARTESIAN_POINT ( 'NONE',  ( 7.860778187331947109, -299.4074188288229834, -193.5166010588536096 ) ) ;
#88325 = CARTESIAN_POINT ( 'NONE',  ( 14.41890826709834172, -286.9900973570545943, -322.5347022575787150 ) ) ;
#88326 = CARTESIAN_POINT ( 'NONE',  ( -34.76829161298174853, -298.5759069919729427, -193.4224475131729548 ) ) ;
#88327 = CARTESIAN_POINT ( 'NONE',  ( -102.7672165908978172, -296.2785247921804057, -302.8559199959760804 ) ) ;
#88328 = EDGE_LOOP ( 'NONE', ( #83750, #35023, #79168, #42333 ) ) ;
#88329 = DIRECTION ( 'NONE',  ( -0.000000000000000000, -1.000000000000000000, -0.000000000000000000 ) ) ;
#88330 = AXIS2_PLACEMENT_3D ( 'NONE', #77277, #19507, #27556 ) ;
#88331 = CARTESIAN_POINT ( 'NONE',  ( -69.37457967765314493, -281.5541621010550557, -201.9130218495632789 ) ) ;
#88332 = CARTESIAN_POINT ( 'NONE',  ( 25.87618300709601726, -281.6398420643884037, -314.2366081631833481 ) ) ;
#88333 = AXIS2_PLACEMENT_3D ( 'NONE', #84271, #42113, #18477 ) ;
#88334 = CARTESIAN_POINT ( 'NONE',  ( -105.8078928284799218, -279.9819793890968640, -244.0156876919396609 ) ) ;
#88335 = CARTESIAN_POINT ( 'NONE',  ( -96.25434435633232511, -279.6594397931527283, -318.3739276372007225 ) ) ;
#88336 = CARTESIAN_POINT ( 'NONE',  ( -29.90079146808069765, -272.6279161110299469, -197.0444034459961529 ) ) ;
#88337 = DIRECTION ( 'NONE',  ( -0.000000000000000000, -0.000000000000000000, -1.000000000000000000 ) ) ;
#88338 = PLANE ( 'NONE',  #42628 ) ;
#88339 = CARTESIAN_POINT ( 'NONE',  ( 15.25790792428147746, -280.9872562388425195, -219.6699268078835132 ) ) ;
#88340 = CARTESIAN_POINT ( 'NONE',  ( 16.84861157140450061, -277.1073962702839140, -324.9108227841372241 ) ) ;
#88341 = AXIS2_PLACEMENT_3D ( 'NONE', #62342, #68504, #47162 ) ;
#88342 = CARTESIAN_POINT ( 'NONE',  ( 17.45970322547478304, -278.2692377983377696, -321.5647002748431191 ) ) ;
#88343 = CARTESIAN_POINT ( 'NONE',  ( -111.2620745014318118, -276.8822345962194618, -289.7615970377026429 ) ) ;
#88344 = ORIENTED_EDGE ( 'NONE', *, *, #92638, .T. ) ;
#88345 = CARTESIAN_POINT ( 'NONE',  ( 82.64890176555634582, -299.5541904835141622, -195.3611179825600175 ) ) ;
#88346 = CARTESIAN_POINT ( 'NONE',  ( 37.97662328196414450, -283.5621720336718568, -272.7184381945962173 ) ) ;
#88347 = CARTESIAN_POINT ( 'NONE',  ( -104.8481244732191584, -290.1283952248891183, -242.0249942809589072 ) ) ;
#88348 = CARTESIAN_POINT ( 'NONE',  ( -12.72847449836845257, -285.7125162726246685, -197.5085139762025221 ) ) ;
#88349 = CARTESIAN_POINT ( 'NONE',  ( -53.93840260113621099, -281.5078336105353856, -342.5424498482227591 ) ) ;
#88351 = CARTESIAN_POINT ( 'NONE',  ( 33.21308620789464783, -285.3228047815757691, -246.6264108556927681 ) ) ;
#88350 = CARTESIAN_POINT ( 'NONE',  ( -23.97614164480430077, -281.4527915258097437, -342.7264187973819958 ) ) ;
#88352 = CARTESIAN_POINT ( 'NONE',  ( 34.14364879179218804, -282.5388704208897934, -253.7185401766971609 ) ) ;
#88353 = CARTESIAN_POINT ( 'NONE',  ( -97.93575550138670849, -271.1552731541447088, -226.0781938378329983 ) ) ;
#88354 = CARTESIAN_POINT ( 'NONE',  ( 23.60288138149907056, -280.5672334012831470, -316.1016733135513732 ) ) ;
#88355 = CARTESIAN_POINT ( 'NONE',  ( 34.36708847235066600, -295.2690317615726485, -248.3872633632298346 ) ) ;
#88356 = ADVANCED_FACE ( 'NONE', ( #3291, #34063, #50118 ), #79015, .T. ) ;
#88357 = CARTESIAN_POINT ( 'NONE',  ( -10.66892226079047212, -288.3992486794542174, -200.0305657835561703 ) ) ;
#88358 = CARTESIAN_POINT ( 'NONE',  ( 184.7149167944524493, -12.49482340714361506, 10.00000000000000000 ) ) ;
#88359 = CARTESIAN_POINT ( 'NONE',  ( -81.11641203582675530, -293.3826606780352222, -208.7730607559209659 ) ) ;
#88360 = CARTESIAN_POINT ( 'NONE',  ( 36.82311238471707782, -273.4075654045568058, -259.1129180082863854 ) ) ;
#88361 = CARTESIAN_POINT ( 'NONE',  ( 31.53812641407240136, -287.1892287272665385, -304.5358678678690012 ) ) ;
#88362 = CARTESIAN_POINT ( 'NONE',  ( 33.40174502640356735, -291.6747861610853079, -249.1656847508699570 ) ) ;
#88363 = CARTESIAN_POINT ( 'NONE',  ( 152.4536156746142410, 275.5000000000000568, -14.50000000000000000 ) ) ;
#88364 = CARTESIAN_POINT ( 'NONE',  ( -108.7650005277292138, -277.4639510712643755, -253.0418905301113455 ) ) ;
#88365 = CARTESIAN_POINT ( 'NONE',  ( -90.92123764730045821, -295.4216403587806212, -218.9056892819436086 ) ) ;
#88366 = CARTESIAN_POINT ( 'NONE',  ( -76.11479323089244531, -290.8973399789280734, -332.7942079984620136 ) ) ;
#88367 = CARTESIAN_POINT ( 'NONE',  ( 219.8344101925596021, 3.000000000000000000, 9.000000000000001776 ) ) ;
#88368 = DIRECTION ( 'NONE',  ( -1.000000000000000000, 0.000000000000000000, -0.000000000000000000 ) ) ;
#88369 = CARTESIAN_POINT ( 'NONE',  ( 37.91921114877387566, -292.1919155545822946, -283.0299677060057206 ) ) ;
#88370 = CARTESIAN_POINT ( 'NONE',  ( 34.77345160926238066, -288.9476863410220062, -254.6816630359113844 ) ) ;
#88371 = CARTESIAN_POINT ( 'NONE',  ( -110.9461476636871708, -288.5520315873618529, -289.2907138257573365 ) ) ;
#88372 = CARTESIAN_POINT ( 'NONE',  ( 36.04098063235412752, -289.0579307670378171, -276.5126682850371367 ) ) ;
#88373 = DIRECTION ( 'NONE',  ( -0.000000000000000000, 1.000000000000000000, -0.000000000000000000 ) ) ;
#88374 = CARTESIAN_POINT ( 'NONE',  ( 13.24383515989090654, -287.5840732446478683, -217.4357199264438236 ) ) ;
#88375 = CARTESIAN_POINT ( 'NONE',  ( -36.27195443380546180, -297.0187270494103018, -345.7215522481367884 ) ) ;
#88376 = CARTESIAN_POINT ( 'NONE',  ( -74.94434090351494149, -285.8906705383787994, 54.50000000000000711 ) ) ;
#88377 = CARTESIAN_POINT ( 'NONE',  ( -77.91302123592927842, -290.7890664145993469, -335.3997267615584406 ) ) ;
#88378 = CARTESIAN_POINT ( 'NONE',  ( -20.10736608977926920, -278.2925059415758824, -196.9495921673949113 ) ) ;
#88379 = CARTESIAN_POINT ( 'NONE',  ( -70.28811465792983881, -277.8077659595787168, -339.9476580797378915 ) ) ;
#88380 = CARTESIAN_POINT ( 'NONE',  ( -74.99388626688092074, -279.2314462878293284, -203.2190509119599540 ) ) ;
#88381 = CARTESIAN_POINT ( 'NONE',  ( -78.43811258538219988, -299.4764012231978541, -207.9858187344139537 ) ) ;
#88382 = CARTESIAN_POINT ( 'NONE',  ( -104.0047476339076411, -283.0067381606190793, -235.9948737452589285 ) ) ;
#88383 = CARTESIAN_POINT ( 'NONE',  ( -110.5111785248877254, -273.3798195326398286, -270.3716561707263963 ) ) ;
#88384 = CARTESIAN_POINT ( 'NONE',  ( 16.16586465980358511, -278.9604871399368449, -218.8308210222380126 ) ) ;
#88385 = CARTESIAN_POINT ( 'NONE',  ( -84.85552501192522357, -281.7072597161362637, -328.3907405089061058 ) ) ;
#88386 = CARTESIAN_POINT ( 'NONE',  ( 175.2296996224750103, 154.6894116713782807, -20.15985230015483154 ) ) ;
#88387 = CARTESIAN_POINT ( 'NONE',  ( 27.05323622525508043, -274.5746043185469034, -311.3982767116811488 ) ) ;
#88388 = CARTESIAN_POINT ( 'NONE',  ( -34.46516265151763037, -299.6089241566747319, -196.6670189504422694 ) ) ;
#88389 = CARTESIAN_POINT ( 'NONE',  ( -111.5792251037152027, -283.2300863215691038, -289.6559415013193757 ) ) ;
#88390 = CARTESIAN_POINT ( 'NONE',  ( -84.23466017814951101, -298.3302029245483595, -214.0413749894937894 ) ) ;
#88391 = CARTESIAN_POINT ( 'NONE',  ( -110.4784897142456401, -274.2593736009206964, -248.0528316499418224 ) ) ;
#88392 = CARTESIAN_POINT ( 'NONE',  ( 15.61029072797740547, -275.9434760508664226, -320.6420701529017379 ) ) ;
#88393 = CARTESIAN_POINT ( 'NONE',  ( 35.58670770306607523, -295.3268785512871659, -252.8006764312624739 ) ) ;
#88394 = CARTESIAN_POINT ( 'NONE',  ( 7.936226338078881781, -288.6194067191822796, -332.7077613498963160 ) ) ;
#88395 = EDGE_CURVE ( 'NONE', #60489, #40992, #32540, .T. ) ;
#88396 = CARTESIAN_POINT ( 'NONE',  ( -74.28218145964285668, -277.6448296314165987, -204.4466655615579214 ) ) ;
#88397 = VECTOR ( 'NONE', #3317, 1000.000000000000000 ) ;
#88398 = CARTESIAN_POINT ( 'NONE',  ( -112.8684122999209620, -290.1971598758132700, -285.4184812480793880 ) ) ;
#88399 = CARTESIAN_POINT ( 'NONE',  ( -39.97852786529680458, -288.1447092853567824, -343.5986674098405729 ) ) ;
#88400 = CARTESIAN_POINT ( 'NONE',  ( 26.36727644629094414, -291.0193906694595967, -230.6881069424669306 ) ) ;
#88401 = ORIENTED_EDGE ( 'NONE', *, *, #70292, .F. ) ;
#88402 = CARTESIAN_POINT ( 'NONE',  ( 198.5952592410606314, 68.60901277742570414, 10.61452171551476198 ) ) ;
#88403 = CARTESIAN_POINT ( 'NONE',  ( -93.48310235590990658, -290.7228100030895348, -223.5855052179659879 ) ) ;
#88404 = CYLINDRICAL_SURFACE ( 'NONE', #29302, 5.000000000000004441 ) ;
#88405 = CARTESIAN_POINT ( 'NONE',  ( -75.99863040647869639, -286.4906103935792316, -203.9789989813614568 ) ) ;
#88406 = CARTESIAN_POINT ( 'NONE',  ( 34.45848030099739390, -290.0519495502701943, -270.3284710469131937 ) ) ;
#88407 = CARTESIAN_POINT ( 'NONE',  ( 35.25995479463410476, -292.9279873997329560, -295.4602537846284918 ) ) ;
#88408 = CARTESIAN_POINT ( 'NONE',  ( 1.855952159964453507, -283.8543508477170576, -336.0637992646063026 ) ) ;
#88409 = CARTESIAN_POINT ( 'NONE',  ( -89.66137462613536968, -285.1223172450450534, -219.3803136969849561 ) ) ;
#88410 = CARTESIAN_POINT ( 'NONE',  ( 34.06967216978969049, -277.0955781586472426, -287.7825261683270242 ) ) ;
#88411 = CARTESIAN_POINT ( 'NONE',  ( -27.87326942609925950, -290.1929268393409416, -196.2673747515878802 ) ) ;
#88412 = AXIS2_PLACEMENT_3D ( 'NONE', #62954, #34519, #90828 ) ;
#88413 = CARTESIAN_POINT ( 'NONE',  ( 17.59289884355095168, -273.6546396988354672, -221.6101244988556971 ) ) ;
#88414 = ORIENTED_EDGE ( 'NONE', *, *, #77975, .F. ) ;
#88415 = CARTESIAN_POINT ( 'NONE',  ( 24.80950920047307307, -22.49099280560490399, -345.4124233396505019 ) ) ;
#88416 = CARTESIAN_POINT ( 'NONE',  ( 38.79500651294415547, -293.3609267962822855, -281.7165657227873226 ) ) ;
#88417 = CARTESIAN_POINT ( 'NONE',  ( -80.15712208741508960, -287.3880858171455088, -209.4032094800290906 ) ) ;
#88418 = CARTESIAN_POINT ( 'NONE',  ( -93.45388892569485506, -296.9161152799579213, -322.6577427359322314 ) ) ;
#88419 = CARTESIAN_POINT ( 'NONE',  ( 35.78209718498725778, -288.1764353590843939, -268.3013227700150765 ) ) ;
#88420 = ADVANCED_FACE ( 'NONE', ( #42543 ), #6117, .T. ) ;
#88421 = CARTESIAN_POINT ( 'NONE',  ( -96.87952786620257939, -276.9584842756896137, -318.8385659375060754 ) ) ;
#88422 = CARTESIAN_POINT ( 'NONE',  ( 38.74979561751858625, -294.0599818243625805, -258.8956749405239748 ) ) ;
#88423 = CARTESIAN_POINT ( 'NONE',  ( 36.52085021038865875, -285.4766479620708992, -253.4325027342885903 ) ) ;
#88424 = CARTESIAN_POINT ( 'NONE',  ( -3.234333105599584979, -294.9473619252771073, -339.3860928775064281 ) ) ;
#88425 = CARTESIAN_POINT ( 'NONE',  ( -93.45881006288888670, -291.5483048053866355, -223.6194661385467555 ) ) ;
#88426 = DIRECTION ( 'NONE',  ( 0.000000000000000000, 0.000000000000000000, -1.000000000000000000 ) ) ;
#88427 = CARTESIAN_POINT ( 'NONE',  ( 175.2296996224750103, 161.0000000000000853, 0.000000000000000000 ) ) ;
#88428 = DIRECTION ( 'NONE',  ( -0.000000000000000000, 1.000000000000000000, -0.000000000000000000 ) ) ;
#88429 = CARTESIAN_POINT ( 'NONE',  ( -73.30353221983686751, -287.1046034826480309, -203.0013678776625738 ) ) ;
#88430 = CARTESIAN_POINT ( 'NONE',  ( -99.90806341382575795, -275.4094976428775681, -320.2154176792147382 ) ) ;
#88431 = EDGE_LOOP ( 'NONE', ( #55139, #24737, #5053, #27342 ) ) ;
#88432 = CARTESIAN_POINT ( 'NONE',  ( -108.7294473697317869, -283.2527957973595676, -287.0898107364959628 ) ) ;
#88433 = CARTESIAN_POINT ( 'NONE',  ( -110.5282576224401936, -278.5210733337091256, -246.3283510950774939 ) ) ;
#88434 = CARTESIAN_POINT ( 'NONE',  ( 37.34815239942914644, -283.4927118035662943, -265.7292335484566479 ) ) ;
#88435 = CARTESIAN_POINT ( 'NONE',  ( -46.01903522638156829, -156.0925041209123947, -363.9939798654107790 ) ) ;
#88436 = CARTESIAN_POINT ( 'NONE',  ( 25.43579381673064077, -280.7070675659978178, -313.9454875174558879 ) ) ;
#88437 = CARTESIAN_POINT ( 'NONE',  ( -38.62853349285001769, -284.0560806223729173, -195.7146434152016354 ) ) ;
#88438 = CARTESIAN_POINT ( 'NONE',  ( -55.06798076574337841, -275.6869646415621560, -196.6991572936201749 ) ) ;
#88439 = CARTESIAN_POINT ( 'NONE',  ( -60.54137627549009437, -298.2354512486919020, -201.0272768415937321 ) ) ;
#88440 = CARTESIAN_POINT ( 'NONE',  ( -38.36585319624217760, -293.7500796885653926, -343.8471342714623802 ) ) ;
#88441 = CARTESIAN_POINT ( 'NONE',  ( -91.25165161343427656, -278.4455034643027034, -325.2720703117487346 ) ) ;
#88442 = CARTESIAN_POINT ( 'NONE',  ( -66.80266182023279953, -277.4492729165524452, -337.1522232000482404 ) ) ;
#88443 = CARTESIAN_POINT ( 'NONE',  ( -43.28354042979076866, -298.9202365054322286, -193.7736677831919110 ) ) ;
#88444 = CARTESIAN_POINT ( 'NONE',  ( -51.27002410595544291, -276.1465561689792594, -345.7765958375545665 ) ) ;
#88445 = CARTESIAN_POINT ( 'NONE',  ( -64.04501568493247987, -182.5871740904552212, -362.3045948284940323 ) ) ;
#88446 = CARTESIAN_POINT ( 'NONE',  ( -29.56210322979992000, -274.9535946256202124, -345.0075661269856369 ) ) ;
#88447 = EDGE_CURVE ( 'NONE', #14856, #16112, #70047, .T. ) ;
#88448 = CARTESIAN_POINT ( 'NONE',  ( -86.00598603367318162, -297.1368840681679444, -329.2711643973815399 ) ) ;
#88449 = DIRECTION ( 'NONE',  ( 0.000000000000000000, -0.000000000000000000, 1.000000000000000000 ) ) ;
#88450 = CARTESIAN_POINT ( 'NONE',  ( -36.09237171215955442, -122.5496321078137356, -22.50000000000000000 ) ) ;
#88451 = CARTESIAN_POINT ( 'NONE',  ( -42.94287154574270460, -284.2040399720792720, -343.5062384627763095 ) ) ;
#88452 = CARTESIAN_POINT ( 'NONE',  ( -113.1952159813393735, -286.2450175381646886, -275.6696175899485866 ) ) ;
#88453 = CARTESIAN_POINT ( 'NONE',  ( -70.02056274128207747, -284.9585084809592672, -204.9561418139582258 ) ) ;
#88454 = CARTESIAN_POINT ( 'NONE',  ( -85.64406883759544087, -276.1331468154814388, -326.2259756062181850 ) ) ;
#88455 = CARTESIAN_POINT ( 'NONE',  ( -95.94654224486873773, -287.0440923702187774, -224.7736176087444449 ) ) ;
#88456 = CARTESIAN_POINT ( 'NONE',  ( -43.79267295890605993, -278.4491646523954387, -196.8999668992775298 ) ) ;
#88457 = CARTESIAN_POINT ( 'NONE',  ( -3.713473766556704803, -277.6771198893313795, -335.5022606361942508 ) ) ;
#88458 = DIRECTION ( 'NONE',  ( 0.000000000000000000, 0.000000000000000000, 1.000000000000000000 ) ) ;
#88459 = CARTESIAN_POINT ( 'NONE',  ( -109.1913906023498413, -273.2227359036598955, -256.8385640283184443 ) ) ;
#88460 = CARTESIAN_POINT ( 'NONE',  ( 36.01849478172940877, -282.0672323828374033, -247.5041579204160769 ) ) ;
#88461 = CARTESIAN_POINT ( 'NONE',  ( 39.34986729319370369, -281.9674126951711628, -264.2023527192749270 ) ) ;
#88462 = EDGE_LOOP ( 'NONE', ( #57058, #53131, #78752, #41365 ) ) ;
#88463 = ORIENTED_EDGE ( 'NONE', *, *, #70954, .F. ) ;
#88464 = EDGE_CURVE ( 'NONE', #30954, #15639, #22813, .T. ) ;
#88465 = CARTESIAN_POINT ( 'NONE',  ( 201.2104617360081704, 15.00000000000001421, -10.00000000000000178 ) ) ;
#88466 = CARTESIAN_POINT ( 'NONE',  ( 4.477828423660729307, -288.4698363977563531, -207.1208566238755679 ) ) ;
#88467 = CARTESIAN_POINT ( 'NONE',  ( -101.3509117173909857, -296.2325176133599598, -234.9291753567264038 ) ) ;
#88468 = CARTESIAN_POINT ( 'NONE',  ( -25.02957679759807874, -291.5538233017906009, -194.4550944704950837 ) ) ;
#88469 = CARTESIAN_POINT ( 'NONE',  ( 36.24623652190252443, -285.9692924546910149, -265.5606461922162680 ) ) ;
#88470 = CARTESIAN_POINT ( 'NONE',  ( 18.25889362138731542, -286.8091116780663583, -318.6447420614047132 ) ) ;
#88471 = CARTESIAN_POINT ( 'NONE',  ( -30.50952235267011403, -287.3454072453388903, -197.2316484089523954 ) ) ;
#88472 = CARTESIAN_POINT ( 'NONE',  ( -85.82230911780693816, -275.7228669224093096, -327.6534832507173860 ) ) ;
#88473 = CARTESIAN_POINT ( 'NONE',  ( -23.47770371204173401, -287.2777825434094439, -345.3428339857504739 ) ) ;
#88474 = CARTESIAN_POINT ( 'NONE',  ( 12.88802453970373740, -288.7529821478595977, -214.5960837472935054 ) ) ;
#88475 = CARTESIAN_POINT ( 'NONE',  ( -84.04596688189603526, -287.6916727221295673, -329.3235533382184599 ) ) ;
#88476 = CARTESIAN_POINT ( 'NONE',  ( 33.88178482580691053, -282.7182723827438053, -287.4621928760510627 ) ) ;
#88477 = CARTESIAN_POINT ( 'NONE',  ( -110.2233965358838788, -292.7886552872353718, -251.9166283540837981 ) ) ;
#88478 = CARTESIAN_POINT ( 'NONE',  ( 82.13009088781083733, -301.0284103969703438, -194.0088967232378536 ) ) ;
#88479 = DIRECTION ( 'NONE',  ( 0.000000000000000000, 1.000000000000000000, -1.224646799147353207E-16 ) ) ;
#88480 = CARTESIAN_POINT ( 'NONE',  ( -70.12677391686942485, -299.5437175786609600, -202.2843000516843119 ) ) ;
#88481 = AXIS2_PLACEMENT_3D ( 'NONE', #28365, #86557, #26950 ) ;
#88482 = CARTESIAN_POINT ( 'NONE',  ( 21.46485241405459021, -280.1401802729444626, -226.8154255989534249 ) ) ;
#88483 = CARTESIAN_POINT ( 'NONE',  ( 14.74183822126638432, -278.7850881649446251, -216.3229377038205996 ) ) ;
#88484 = CARTESIAN_POINT ( 'NONE',  ( 22.15509706543970125, -293.4035999149492682, -319.0057344757882447 ) ) ;
#88485 = CARTESIAN_POINT ( 'NONE',  ( -63.34244523359843271, -296.1076670961292052, -201.2389648726340283 ) ) ;
#88486 = CARTESIAN_POINT ( 'NONE',  ( -9.471482530709096181, -274.7649470605410897, -339.4007788391619442 ) ) ;
#88487 = CARTESIAN_POINT ( 'NONE',  ( 6.369606081040358525, -295.7598689177297615, -329.5055550071194830 ) ) ;
#88488 = DIRECTION ( 'NONE',  ( 0.000000000000000000, 0.000000000000000000, -1.000000000000000000 ) ) ;
#88489 = CARTESIAN_POINT ( 'NONE',  ( -113.7517970869267003, -271.1629708653914008, -267.4974886568448369 ) ) ;
#88490 = CARTESIAN_POINT ( 'NONE',  ( -111.6194279198050623, -294.5889328096234294, -286.3858854163530054 ) ) ;
#88491 = CARTESIAN_POINT ( 'NONE',  ( -55.17255378784323483, -293.2435614495827849, -198.9647905334667541 ) ) ;
#88492 = LINE ( 'NONE', #31219, #15749 ) ;
#88493 = CARTESIAN_POINT ( 'NONE',  ( 34.37274956735878106, -294.1644075634281990, -255.8821873482296496 ) ) ;
#88494 = CARTESIAN_POINT ( 'NONE',  ( 140.6539576904058606, 275.0000000000000568, 10.50000000000000000 ) ) ;
#88496 = CARTESIAN_POINT ( 'NONE',  ( -69.72406891981063382, -295.4908810974197877, -335.7857478358227468 ) ) ;
#88495 = CARTESIAN_POINT ( 'NONE',  ( -90.71972796632600478, -283.3198945101642039, -217.1709596275337901 ) ) ;
#88497 = CARTESIAN_POINT ( 'NONE',  ( -111.7212154822737062, -284.8037971640941350, -250.2436990138195370 ) ) ;
#88498 = CARTESIAN_POINT ( 'NONE',  ( 26.61912792095626301, -282.9343685800570256, -230.0346814948160556 ) ) ;
#88499 = CARTESIAN_POINT ( 'NONE',  ( -63.19033816739273846, -285.3911756945738034, -197.8518620009969311 ) ) ;
#88500 = CARTESIAN_POINT ( 'NONE',  ( -98.23879439052350904, -289.1458171233265944, -226.7812969986545966 ) ) ;
#88501 = CARTESIAN_POINT ( 'NONE',  ( -112.3381139276885108, -270.1608578419545665, -261.8788190812425682 ) ) ;
#88502 = CARTESIAN_POINT ( 'NONE',  ( -77.30325992398987012, -284.1891223428384023, -208.6215973698091091 ) ) ;
#88503 = CARTESIAN_POINT ( 'NONE',  ( -113.0570721683566546, -289.3193766518436973, -282.5543516298441205 ) ) ;
#88504 = FACE_OUTER_BOUND ( 'NONE', #92528, .T. ) ;
#88505 = CARTESIAN_POINT ( 'NONE',  ( -58.61963103197609115, -296.9320747185212781, -341.0271640727563067 ) ) ;
#88506 = CARTESIAN_POINT ( 'NONE',  ( -109.0594940703633000, -280.3149441631099990, -243.8422918023784973 ) ) ;
#88508 = CARTESIAN_POINT ( 'NONE',  ( 2.719130064279232872, -280.2722908003071893, -209.2495025191904290 ) ) ;
#88507 = CARTESIAN_POINT ( 'NONE',  ( 33.92249740727758933, -291.8895146090274579, -295.0121052964305477 ) ) ;
#88509 = CARTESIAN_POINT ( 'NONE',  ( -56.06822933098914064, -295.4535948077426042, -345.0492502961826062 ) ) ;
#88510 = CARTESIAN_POINT ( 'NONE',  ( -69.16367997142182844, -283.7167501598232775, -201.8147253816856335 ) ) ;
#88511 = CARTESIAN_POINT ( 'NONE',  ( -112.2157321526965745, -280.6081071514298628, -266.0160087148465209 ) ) ;
#88512 = CARTESIAN_POINT ( 'NONE',  ( -45.12762775168771157, -294.2117741372102842, -343.2320005252281021 ) ) ;
#88513 = CARTESIAN_POINT ( 'NONE',  ( -23.78527057963961866, -296.2216931636220920, -195.3657311741189631 ) ) ;
#88514 = EDGE_LOOP ( 'NONE', ( #9939, #76068, #4782, #14204 ) ) ;
#88515 = CARTESIAN_POINT ( 'NONE',  ( 82.64890176555634582, -299.5541904835138780, -192.9651424135223863 ) ) ;
#88516 = CARTESIAN_POINT ( 'NONE',  ( -8.637638259825131115, -282.4095485859864425, -201.4559393924883466 ) ) ;
#88517 = CARTESIAN_POINT ( 'NONE',  ( -108.5355912949711694, -296.2761499308048201, -253.9471512955446713 ) ) ;
#88518 = FACE_OUTER_BOUND ( 'NONE', #25441, .T. ) ;
#88519 = CARTESIAN_POINT ( 'NONE',  ( -20.25526795762938548, -274.3380690714490697, -345.3683826091709648 ) ) ;
#88520 = CARTESIAN_POINT ( 'NONE',  ( -10.39464456842249618, -273.5920247200083963, -198.3460847391739605 ) ) ;
#88521 = CARTESIAN_POINT ( 'NONE',  ( 0.4901084896368336219, -289.8745069564153596, -336.9195063054415300 ) ) ;
#88522 = CARTESIAN_POINT ( 'NONE',  ( -108.6631783807477944, -290.1794428326551838, -285.9835141821380944 ) ) ;
#88523 = CARTESIAN_POINT ( 'NONE',  ( -46.56222053103841318, -281.4532781753128461, -197.1953051579458531 ) ) ;
#88524 = CARTESIAN_POINT ( 'NONE',  ( 14.03918459206960456, -276.3883281344809575, -217.3852263004769156 ) ) ;
#88525 = CARTESIAN_POINT ( 'NONE',  ( -43.77065947555172443, -278.7641600716794414, -197.1956397570254467 ) ) ;
#88526 = CARTESIAN_POINT ( 'NONE',  ( 28.53534170143589677, -278.0298666276397057, -306.3196615243484189 ) ) ;
#88527 = ORIENTED_EDGE ( 'NONE', *, *, #57879, .T. ) ;
#88528 = CARTESIAN_POINT ( 'NONE',  ( -73.94299285587297277, -273.4134409584095806, -202.5571389455984956 ) ) ;
#88529 = CARTESIAN_POINT ( 'NONE',  ( -9.205429504363960902, -294.3429056573678508, -201.3884716815977356 ) ) ;
#88530 = FACE_OUTER_BOUND ( 'NONE', #15625, .T. ) ;
#88531 = CARTESIAN_POINT ( 'NONE',  ( 205.7381008070598227, 0.000000000000000000, 7.000000000000000000 ) ) ;
#88532 = EDGE_CURVE ( 'NONE', #6460, #16264, #28020, .T. ) ;
#88533 = CARTESIAN_POINT ( 'NONE',  ( 16.62666955183015105, -290.9489003618078868, -217.1109015138176233 ) ) ;
#88534 = CARTESIAN_POINT ( 'NONE',  ( -100.7680774266537753, -272.5575023856835628, -233.9953221529800658 ) ) ;
#88535 = FACE_OUTER_BOUND ( 'NONE', #79624, .T. ) ;
#88536 = CARTESIAN_POINT ( 'NONE',  ( 24.24333332018625242, -294.4686228622493331, -225.3056920149629434 ) ) ;
#88537 = CARTESIAN_POINT ( 'NONE',  ( -37.37352853689063181, -300.5519495502701375, -190.3611179825600175 ) ) ;
#88538 = CARTESIAN_POINT ( 'NONE',  ( -24.86050574439200744, -288.2117554192093394, -196.5233848264242340 ) ) ;
#88539 = CARTESIAN_POINT ( 'NONE',  ( 23.95320766709258820, -274.1370893526035388, -313.3797822893422449 ) ) ;
#88540 = CARTESIAN_POINT ( 'NONE',  ( 16.47118851754191482, -276.7439802151927211, -218.8522281758815780 ) ) ;
#88541 = CARTESIAN_POINT ( 'NONE',  ( -67.11806428619449605, -289.7385636203684385, -202.1358855703558675 ) ) ;
#88542 = CARTESIAN_POINT ( 'NONE',  ( -36.78579942146701853, -281.9194800908829279, -194.5855178512138650 ) ) ;
#88543 = VECTOR ( 'NONE', #43839, 1000.000000000000000 ) ;
#88544 = EDGE_LOOP ( 'NONE', ( #40272, #62020, #56075 ) ) ;
#88545 = CARTESIAN_POINT ( 'NONE',  ( -71.46380203444815038, -282.8640336087179321, -335.0107493035188782 ) ) ;
#88546 = CARTESIAN_POINT ( 'NONE',  ( -103.3327688262298665, -279.1195643356890059, -309.5378694227637766 ) ) ;
#88547 = CARTESIAN_POINT ( 'NONE',  ( -69.03624981959376328, -282.2546929003748346, -340.1140013045026080 ) ) ;
#88548 = CARTESIAN_POINT ( 'NONE',  ( -73.97398428856054409, -278.4677835439621845, -337.8364018855518793 ) ) ;
#88549 = ADVANCED_FACE ( 'NONE', ( #34528 ), #55839, .F. ) ;
#88550 = CARTESIAN_POINT ( 'NONE',  ( 21.21116831999255581, -277.7366993535750908, -319.2923896937128347 ) ) ;
#88551 = CARTESIAN_POINT ( 'NONE',  ( -82.13390479932378696, -287.9090924074130839, -214.2458315076590907 ) ) ;
#88552 = ORIENTED_EDGE ( 'NONE', *, *, #37852, .T. ) ;
#88553 = CARTESIAN_POINT ( 'NONE',  ( -100.4014615540004627, -298.0042605503799109, -311.0575292080845884 ) ) ;
#88554 = CARTESIAN_POINT ( 'NONE',  ( -109.9270766119712164, -291.4956652911773745, -280.7267191666221606 ) ) ;
#88555 = CARTESIAN_POINT ( 'NONE',  ( -69.99315480742112072, -275.5044141797649218, -337.4999981691831294 ) ) ;
#88556 = CARTESIAN_POINT ( 'NONE',  ( -26.26977446216316281, -290.6732074012569456, -345.5368219965002936 ) ) ;
#88557 = CARTESIAN_POINT ( 'NONE',  ( -96.83949755286823802, -290.4943465611121383, -227.8031088026038731 ) ) ;
#88558 = CARTESIAN_POINT ( 'NONE',  ( 33.98292406371783869, -287.4279761727746632, -299.3530377534742115 ) ) ;
#88559 = CARTESIAN_POINT ( 'NONE',  ( 208.4306832106270804, -148.7221692137691491, -7.500000000000012434 ) ) ;
#88560 = CARTESIAN_POINT ( 'NONE',  ( -104.8532600564601722, -282.5552102055612522, -300.1710104541108990 ) ) ;
#88561 = CARTESIAN_POINT ( 'NONE',  ( -61.63727555923826174, -291.2316389326693979, -340.5080387541444793 ) ) ;
#88562 = CARTESIAN_POINT ( 'NONE',  ( -97.12606839542758053, -283.6291752243014912, -227.2520467831803614 ) ) ;
#88563 = CARTESIAN_POINT ( 'NONE',  ( -2.932933465215186164, -281.8320255687440863, -205.4062556964880741 ) ) ;
#88564 = CARTESIAN_POINT ( 'NONE',  ( 21.31699990451652482, -289.1625275061616662, -319.8785606080607522 ) ) ;
#88565 = CARTESIAN_POINT ( 'NONE',  ( -105.3227668628072564, -278.6868174819926480, -297.1298125180252896 ) ) ;
#88566 = CARTESIAN_POINT ( 'NONE',  ( 27.72324783100738443, -291.8143472972927270, -229.8311499959664843 ) ) ;
#88567 = CARTESIAN_POINT ( 'NONE',  ( -33.74513533688882205, -286.8991606241152681, -193.6068116376738431 ) ) ;
#88568 = CARTESIAN_POINT ( 'NONE',  ( 39.54315984231079284, -288.0952187408752820, -274.4134374820295648 ) ) ;
#88569 = CARTESIAN_POINT ( 'NONE',  ( -51.01581621922784393, -283.3983365598688806, -342.1205637136178552 ) ) ;
#88570 = ORIENTED_EDGE ( 'NONE', *, *, #16793, .T. ) ;
#88571 = DIRECTION ( 'NONE',  ( 0.000000000000000000, 0.000000000000000000, 1.000000000000000000 ) ) ;
#88572 = CARTESIAN_POINT ( 'NONE',  ( 36.21693448439535246, -295.1818018899278968, -252.2108353981194000 ) ) ;
#88573 = CARTESIAN_POINT ( 'NONE',  ( 36.61553010370923289, -292.4837718926271464, -289.9475002516084601 ) ) ;
#88574 = CARTESIAN_POINT ( 'NONE',  ( 25.57159628898023129, -275.1246497180182473, -307.8487903784329660 ) ) ;
#88575 = CARTESIAN_POINT ( 'NONE',  ( -62.80346509521832132, -297.0777911781560761, -197.8007203044634537 ) ) ;
#88576 = CARTESIAN_POINT ( 'NONE',  ( -2.090914190285290353, -291.0076424977363558, -205.6313333339709288 ) ) ;
#88577 = CARTESIAN_POINT ( 'NONE',  ( -92.58653704136588658, -295.4867382466309209, -221.1068591912486454 ) ) ;
#88578 = CARTESIAN_POINT ( 'NONE',  ( -90.11241298346455153, -292.4903711764793570, -219.3475671408286019 ) ) ;
#88579 = CARTESIAN_POINT ( 'NONE',  ( 21.58309136429705433, -295.2407226535077598, -313.9741323465929099 ) ) ;
#88580 = CARTESIAN_POINT ( 'NONE',  ( 199.0061125298537377, 250.5000000000000568, -7.725424859374024678 ) ) ;
#88581 = CARTESIAN_POINT ( 'NONE',  ( -2.832400743315037328, -292.5968778718313956, -337.1378855418639660 ) ) ;
#88582 = CARTESIAN_POINT ( 'NONE',  ( -109.7411779152843962, -298.8045916485828002, -250.7344950078710895 ) ) ;
#88583 = CARTESIAN_POINT ( 'NONE',  ( 34.79706119545801357, -288.3236311210037570, -257.4496525727625453 ) ) ;
#88584 = CARTESIAN_POINT ( 'NONE',  ( 31.52699331031440266, -277.9309207650316580, -300.9472237163761292 ) ) ;
#88585 = CARTESIAN_POINT ( 'NONE',  ( -113.7175655017542653, -277.2933064376213679, -265.8861364156356899 ) ) ;
#88586 = CARTESIAN_POINT ( 'NONE',  ( -10.37557693812024873, -273.7434196691516490, -198.2896006618775004 ) ) ;
#88587 = CARTESIAN_POINT ( 'NONE',  ( 36.56650901000911347, -279.7523137793989463, -279.6619491718978452 ) ) ;
#88588 = CARTESIAN_POINT ( 'NONE',  ( -99.58364084687843842, -277.5398315875208937, -226.4022595844365924 ) ) ;
#88589 = CARTESIAN_POINT ( 'NONE',  ( -96.00804401660965937, -294.6191045367037873, -314.6481352243256424 ) ) ;
#88590 = CARTESIAN_POINT ( 'NONE',  ( 157.7277585059063938, 1.242640687119284992, 9.999999999999998224 ) ) ;
#88591 = CARTESIAN_POINT ( 'NONE',  ( -19.25441361073336211, -274.9423732675803080, -199.4796509324681040 ) ) ;
#88592 = FACE_OUTER_BOUND ( 'NONE', #36050, .T. ) ;
#88593 = CARTESIAN_POINT ( 'NONE',  ( -112.5447354075375870, -288.6334258410384450, -265.5746490239581021 ) ) ;
#88594 = CARTESIAN_POINT ( 'NONE',  ( -68.05387736649520036, -289.4444033109572274, -340.9710476615807124 ) ) ;
#88595 = CARTESIAN_POINT ( 'NONE',  ( -36.93397297826390258, -300.0371189401193419, -195.0057727177184290 ) ) ;
#88596 = CARTESIAN_POINT ( 'NONE',  ( -111.8738659412356071, -294.6454663210720923, -263.0969798992497317 ) ) ;
#88597 = CARTESIAN_POINT ( 'NONE',  ( -106.8638966795725196, -283.3292937786462744, -303.0845500557905439 ) ) ;
#88598 = FACE_OUTER_BOUND ( 'NONE', #42517, .T. ) ;
#88599 = CARTESIAN_POINT ( 'NONE',  ( -76.07019371423882603, -281.5689830938668479, -334.6472283539877139 ) ) ;
#88600 = VECTOR ( 'NONE', #68059, 1000.000000000000000 ) ;
#88601 = CARTESIAN_POINT ( 'NONE',  ( 204.6539576904058606, 293.9636489450775230, 0.000000000000000000 ) ) ;
#88602 = CARTESIAN_POINT ( 'NONE',  ( -81.95831902828879834, -290.2238142994540908, -212.0174204110471692 ) ) ;
#88603 = CARTESIAN_POINT ( 'NONE',  ( -111.1028298048073850, -282.5773051127588928, -279.1819974564393760 ) ) ;
#88604 = LINE ( 'NONE', #1978, #92581 ) ;
#88605 = DIRECTION ( 'NONE',  ( 1.000000000000000000, 0.000000000000000000, -0.000000000000000000 ) ) ;
#88606 = CARTESIAN_POINT ( 'NONE',  ( -16.86267289465900276, -290.3163318994787119, -198.1571647211805782 ) ) ;
#88607 = CARTESIAN_POINT ( 'NONE',  ( -35.07284752423389307, -278.6233188190329315, -344.1262366008237450 ) ) ;
#88608 = CARTESIAN_POINT ( 'NONE',  ( -38.70998809155816645, -284.2740262467856383, -346.9518256965196201 ) ) ;
#88610 = CARTESIAN_POINT ( 'NONE',  ( -96.57482485779813430, -285.1490515983921910, -227.6732145155041280 ) ) ;
#88609 = CARTESIAN_POINT ( 'NONE',  ( 6.421262212874594866, -272.7209496839143412, -208.7004858517199750 ) ) ;
#88611 = CARTESIAN_POINT ( 'NONE',  ( 30.83068632654069674, -277.3472483584012593, -298.2078099481626623 ) ) ;
#88612 = CARTESIAN_POINT ( 'NONE',  ( 24.12559479006556984, -276.9041752298854817, -310.1329236667493205 ) ) ;
#88613 = EDGE_CURVE ( 'NONE', #56036, #74598, #58302, .T. ) ;
#88614 = CARTESIAN_POINT ( 'NONE',  ( -104.8891900616303161, -286.9816329611392121, -237.7676025340173283 ) ) ;
#88615 = ORIENTED_EDGE ( 'NONE', *, *, #57514, .F. ) ;
#88616 = CARTESIAN_POINT ( 'NONE',  ( 165.7865175155837676, 3.000000000000000000, 10.00000000000000000 ) ) ;
#88617 = CARTESIAN_POINT ( 'NONE',  ( -58.85335605541897053, -295.1561378050164990, -344.3507737423693129 ) ) ;
#88618 = CARTESIAN_POINT ( 'NONE',  ( 16.19194048292264299, -288.7964429797792150, -218.3419280124267914 ) ) ;
#88619 = CARTESIAN_POINT ( 'NONE',  ( 195.5192339169639979, 26.76774044649046758, 14.92136003405341249 ) ) ;
#88620 = CARTESIAN_POINT ( 'NONE',  ( -19.11405058567864046, -292.3380690714489560, -350.3683826091709648 ) ) ;
#88621 = CARTESIAN_POINT ( 'NONE',  ( -96.56989684997603263, -278.1297716425290218, -221.6219857666048085 ) ) ;
#88622 = CARTESIAN_POINT ( 'NONE',  ( -95.04166692484002965, -289.6313911323829302, -220.5701624605165989 ) ) ;
#88623 = CARTESIAN_POINT ( 'NONE',  ( -111.0029261204034441, -286.1007063871209084, -268.1859085910183467 ) ) ;
#88624 = CARTESIAN_POINT ( 'NONE',  ( -109.1498422221659013, -280.0782778267928848, -288.3455259190778861 ) ) ;
#88625 = CARTESIAN_POINT ( 'NONE',  ( -2.507841784823749531, -287.9289932179920584, -202.3375934870531694 ) ) ;
#88626 = CARTESIAN_POINT ( 'NONE',  ( -18.20129406809804351, -284.8057763877874322, -342.9314820245442661 ) ) ;
#88627 = CARTESIAN_POINT ( 'NONE',  ( -3.992928659201691044, -276.7911157575695711, -339.7792152245206125 ) ) ;
#88628 = CARTESIAN_POINT ( 'NONE',  ( -76.04232596691096546, -295.5529464540472873, -206.4724589168351656 ) ) ;
#88629 = CARTESIAN_POINT ( 'NONE',  ( -97.69557331558651470, -279.0253341055908436, -222.5446982524696296 ) ) ;
#88630 = CARTESIAN_POINT ( 'NONE',  ( -111.5322523117048519, -298.3857429496532063, -277.0529540730821623 ) ) ;
#88631 = CARTESIAN_POINT ( 'NONE',  ( 156.4972887742121088, 15.41695093167224861, 9.987829044572988479 ) ) ;
#88632 = CARTESIAN_POINT ( 'NONE',  ( -4.829096099716510437, -276.9805209788416391, -202.7746430608542312 ) ) ;
#88633 = CARTESIAN_POINT ( 'NONE',  ( -36.18366026708313399, -296.2060932151273960, -194.5966729150893286 ) ) ;
#88634 = CARTESIAN_POINT ( 'NONE',  ( 175.2296996224750103, 134.0000000000000284, -24.00000000000001066 ) ) ;
#88635 = CARTESIAN_POINT ( 'NONE',  ( -109.1049129487920766, -277.8781946815134916, -284.1396437672756861 ) ) ;
#88636 = CARTESIAN_POINT ( 'NONE',  ( -4.012810972172158763, -275.6870059649224345, -201.3742721965190299 ) ) ;
#88637 = CARTESIAN_POINT ( 'NONE',  ( 19.60089435919962852, -281.3128338431170050, -321.9205309625331211 ) ) ;
#88638 = CARTESIAN_POINT ( 'NONE',  ( -64.16755264160346428, -291.1669910849859662, -339.3968251634083799 ) ) ;
#88639 = CARTESIAN_POINT ( 'NONE',  ( -100.1907017475590465, -298.6490109233980093, -227.0633194431830191 ) ) ;
#88640 = CARTESIAN_POINT ( 'NONE',  ( -35.85324569180153276, -299.2754672156734159, -193.7578905500841415 ) ) ;
#88641 = CARTESIAN_POINT ( 'NONE',  ( 35.73471441455897235, -295.3441041765839259, -254.1815934477064047 ) ) ;
#88642 = CARTESIAN_POINT ( 'NONE',  ( 35.72509246231228275, -279.7599993724422234, -286.5250361817040243 ) ) ;
#88643 = CARTESIAN_POINT ( 'NONE',  ( 1.123503733920095282, -282.4896834319559389, -206.5696595108736631 ) ) ;
#88644 = CARTESIAN_POINT ( 'NONE',  ( -82.80461748053576798, -295.5052736394017643, -211.3514467006139057 ) ) ;
#88645 = CARTESIAN_POINT ( 'NONE',  ( -112.3458192515958984, -285.9786807552464438, -284.0974308917863596 ) ) ;
#88646 = CARTESIAN_POINT ( 'NONE',  ( 18.05009668379463861, -287.1546567275788107, -318.4576719984431179 ) ) ;
#88647 = CARTESIAN_POINT ( 'NONE',  ( -69.68305041046212978, -196.9792667690914243, -360.2536513082256420 ) ) ;
#88648 = VERTEX_POINT ( 'NONE', #12764 ) ;
#88649 = CARTESIAN_POINT ( 'NONE',  ( 12.02124675044623991, -286.9559458369145659, -328.6869764571741257 ) ) ;
#88650 = CARTESIAN_POINT ( 'NONE',  ( 25.71216626638022262, -287.7254179250531365, -307.2890142064944712 ) ) ;
#88651 = ORIENTED_EDGE ( 'NONE', *, *, #25921, .T. ) ;
#88652 = CARTESIAN_POINT ( 'NONE',  ( -65.12732393649616824, -284.4864900801344447, -341.8556918332768646 ) ) ;
#88653 = CARTESIAN_POINT ( 'NONE',  ( 32.53785859821213222, -276.1664245850197972, -291.5925520920281997 ) ) ;
#88654 = CARTESIAN_POINT ( 'NONE',  ( -22.24114255554162511, -291.1613865355294024, -195.1174766504721561 ) ) ;
#88655 = CARTESIAN_POINT ( 'NONE',  ( -4.200242670873950424, -283.2780560982531028, -339.7654770284050301 ) ) ;
#88656 = CARTESIAN_POINT ( 'NONE',  ( 24.02254911227997880, -282.4639998806835024, -225.0054494358969919 ) ) ;
#88657 = CARTESIAN_POINT ( 'NONE',  ( -34.47550785935203521, -283.3503265921961543, -347.2865964241582333 ) ) ;
#88658 = CARTESIAN_POINT ( 'NONE',  ( -87.53062500017432512, -279.3282393588016248, -217.2811494362988753 ) ) ;
#88659 = CARTESIAN_POINT ( 'NONE',  ( 10.64812456238590777, -278.1952119285918457, -210.2361428286349110 ) ) ;
#88660 = CARTESIAN_POINT ( 'NONE',  ( -109.6919961625490885, -267.3296139387366566, -307.0733402615499017 ) ) ;
#88661 = ORIENTED_EDGE ( 'NONE', *, *, #31412, .F. ) ;
#88662 = CARTESIAN_POINT ( 'NONE',  ( -3.004098830780497664, -278.5974601216422570, -336.8513997296727780 ) ) ;
#88663 = CARTESIAN_POINT ( 'NONE',  ( -13.73103683141038900, -91.22335786429552229, -359.5740944199137061 ) ) ;
#88664 = CARTESIAN_POINT ( 'NONE',  ( -34.46657808638739340, -297.4376651245657399, -197.2595125645529492 ) ) ;
#88665 = CARTESIAN_POINT ( 'NONE',  ( 17.45018901237726539, -292.3167485788576414, -216.2733541137505426 ) ) ;
#88666 = CARTESIAN_POINT ( 'NONE',  ( -29.80965390781157964, -125.3617451572103505, -360.7801904132562640 ) ) ;
#88668 = CARTESIAN_POINT ( 'NONE',  ( -70.34836896605899881, -287.8945034334603861, -336.3827083876683446 ) ) ;
#88667 = CARTESIAN_POINT ( 'NONE',  ( -3.714752801233152546, -297.0401022983633084, -193.9583019553880092 ) ) ;
#88669 = CARTESIAN_POINT ( 'NONE',  ( -15.20223488990918526, -296.6229829561627866, -341.2721600963799347 ) ) ;
#88670 = CARTESIAN_POINT ( 'NONE',  ( -72.62538878706820356, -286.8898222516241958, -205.8773942066183338 ) ) ;
#88671 = ORIENTED_EDGE ( 'NONE', *, *, #88447, .T. ) ;
#88672 = CARTESIAN_POINT ( 'NONE',  ( -95.39567499708275022, -296.8128067305437980, -320.5861736359397014 ) ) ;
#88673 = CARTESIAN_POINT ( 'NONE',  ( -73.82208542625367897, -284.0426006330703785, -333.7209790299020824 ) ) ;
#88674 = CARTESIAN_POINT ( 'NONE',  ( -9.275710232668592070, -297.1911152518655399, -193.7637831632354164 ) ) ;
#88675 = CARTESIAN_POINT ( 'NONE',  ( 21.18080603953344365, -293.6820332346684381, -220.5487007733434552 ) ) ;
#88676 = ADVANCED_FACE ( 'NONE', ( #57256 ), #92739, .F. ) ;
#88677 = CARTESIAN_POINT ( 'NONE',  ( 22.15767862449141035, -293.3889368381479699, -221.5825280933508736 ) ) ;
#88678 = CARTESIAN_POINT ( 'NONE',  ( -89.81779553026244400, -291.4521429466844324, -219.6141041212159166 ) ) ;
#88679 = ORIENTED_EDGE ( 'NONE', *, *, #45323, .F. ) ;
#88680 = CARTESIAN_POINT ( 'NONE',  ( 18.23474450399076829, -300.6012835206878435, -194.5789127208665263 ) ) ;
#88681 = CARTESIAN_POINT ( 'NONE',  ( -18.63202222213688586, -273.0827206845700630, -196.0234190324801489 ) ) ;
#88682 = EDGE_CURVE ( 'NONE', #62086, #54214, #32511, .T. ) ;
#88683 = EDGE_LOOP ( 'NONE', ( #73349, #72571, #175, #20986 ) ) ;
#88684 = CARTESIAN_POINT ( 'NONE',  ( 24.31458164941571098, -275.6725296414787181, -316.3831759634095420 ) ) ;
#88685 = CARTESIAN_POINT ( 'NONE',  ( -109.9126507882185138, -271.1305985069589042, -256.6755721001413235 ) ) ;
#88686 = CARTESIAN_POINT ( 'NONE',  ( -108.4164675602245040, -280.6915679219507638, -248.9311642852750595 ) ) ;
#88687 = CARTESIAN_POINT ( 'NONE',  ( 21.80698654469597386, -274.3116796373132615, -315.2197665118432610 ) ) ;
#88688 = CARTESIAN_POINT ( 'NONE',  ( -107.0889004431211049, -298.0608581902636729, -247.3425335915484595 ) ) ;
#88689 = CARTESIAN_POINT ( 'NONE',  ( -35.39605138937105977, -275.0183882440737761, -197.1391267947627455 ) ) ;
#88690 = CARTESIAN_POINT ( 'NONE',  ( 7.383749154418845606, -300.2033872413640552, -194.1491647012940405 ) ) ;
#88691 = CARTESIAN_POINT ( 'NONE',  ( -90.98020256241385084, -271.3151992230797305, -217.4336406336886398 ) ) ;
#88692 = CARTESIAN_POINT ( 'NONE',  ( 24.51793458218403288, -294.7420128473718250, -309.4084772319353647 ) ) ;
#88693 = CARTESIAN_POINT ( 'NONE',  ( -70.46985088808011710, -290.1812180999034467, -204.6503841103993580 ) ) ;
#88694 = DIRECTION ( 'NONE',  ( 0.9998346970812742596, 0.000000000000000000, 0.01818181818181330636 ) ) ;
#88695 = CARTESIAN_POINT ( 'NONE',  ( 24.32209758158868596, -276.6570648336410727, -316.3731050667935847 ) ) ;
#88696 = CARTESIAN_POINT ( 'NONE',  ( -43.48424047368110479, -274.1392232603014918, -197.5692963520713192 ) ) ;
#88697 = DIRECTION ( 'NONE',  ( -0.000000000000000000, -1.000000000000000000, -0.000000000000000000 ) ) ;
#88698 = CARTESIAN_POINT ( 'NONE',  ( -99.39836246933839448, -282.6388667859432076, -315.1963967523564065 ) ) ;
#88699 = CARTESIAN_POINT ( 'NONE',  ( -60.99002866002962264, -297.3584137180978928, -341.7652595139043115 ) ) ;
#88700 = DIRECTION ( 'NONE',  ( 0.000000000000000000, 0.000000000000000000, 1.000000000000000000 ) ) ;
#88701 = CARTESIAN_POINT ( 'NONE',  ( -72.44252079047399207, -284.7721578009734458, -206.1554842894346677 ) ) ;
#88702 = CARTESIAN_POINT ( 'NONE',  ( -27.63470881315206995, -280.9291011480655698, -344.9504649272167285 ) ) ;
#88703 = CARTESIAN_POINT ( 'NONE',  ( -37.83875424500602946, -275.2982834352270629, -344.3854110489194795 ) ) ;
#88704 = CARTESIAN_POINT ( 'NONE',  ( -3.613444594755383932, -275.1725813218038184, -335.7658555576074946 ) ) ;
#88705 = CARTESIAN_POINT ( 'NONE',  ( 37.33900201408090425, -283.4567204032774157, -262.9159391563083545 ) ) ;
#88706 = CARTESIAN_POINT ( 'NONE',  ( 33.28410932529845212, -277.0204580825899825, -290.3852732630734295 ) ) ;
#88707 = CARTESIAN_POINT ( 'NONE',  ( 175.2296996224750103, 134.0000000000000284, -24.00000000000001066 ) ) ;
#88708 = CARTESIAN_POINT ( 'NONE',  ( -110.2655024081480519, -271.2344611497756546, -248.0775304768255296 ) ) ;
#88709 = CARTESIAN_POINT ( 'NONE',  ( -66.67116884272201105, -281.6689944626465945, -201.1526597322445298 ) ) ;
#88710 = DIRECTION ( 'NONE',  ( -0.000000000000000000, -0.000000000000000000, 1.000000000000000000 ) ) ;
#88711 = CARTESIAN_POINT ( 'NONE',  ( 24.35490971149054573, -288.8837527053555050, -226.7172366229177953 ) ) ;
#88712 = DIRECTION ( 'NONE',  ( -1.000000000000000000, 0.000000000000000000, 0.000000000000000000 ) ) ;
#88713 = CARTESIAN_POINT ( 'NONE',  ( -57.23126370594855672, -287.3084849448018758, -342.7288532995590344 ) ) ;
#88714 = DIRECTION ( 'NONE',  ( -0.000000000000000000, -1.000000000000000000, -0.000000000000000000 ) ) ;
#88715 = CARTESIAN_POINT ( 'NONE',  ( -102.8800179669123338, -295.7944932136568923, -237.2047042443511202 ) ) ;
#88716 = CARTESIAN_POINT ( 'NONE',  ( -110.8493334174409313, -288.5560522963962171, -280.8204182715599018 ) ) ;
#88717 = CARTESIAN_POINT ( 'NONE',  ( 192.3098639061998369, 281.3337059592261085, -109.1536320133224081 ) ) ;
#88718 = CARTESIAN_POINT ( 'NONE',  ( -55.76085204751009883, -295.8150078359686290, -197.6043155704055323 ) ) ;
#88719 = CARTESIAN_POINT ( 'NONE',  ( 34.21087566743413788, -285.6937967938679321, -243.8481655141461033 ) ) ;
#88720 = CARTESIAN_POINT ( 'NONE',  ( 1.539924987887209884, -284.1235777564119758, -333.1476651281887484 ) ) ;
#88721 = CARTESIAN_POINT ( 'NONE',  ( -98.97982171020632336, -282.1939714606062353, -314.8868599312997389 ) ) ;
#88722 = CARTESIAN_POINT ( 'NONE',  ( -72.62694873940402829, -291.5714589620088191, -206.3985147042467361 ) ) ;
#88723 = CARTESIAN_POINT ( 'NONE',  ( 31.91525809091074706, -283.3078502666593295, -295.3885569268322797 ) ) ;
#88724 = CARTESIAN_POINT ( 'NONE',  ( -34.83078023047895755, -283.8226762067649815, -343.4919586218937297 ) ) ;
#88725 = CARTESIAN_POINT ( 'NONE',  ( -7.546561547507297796, -290.6434032765839675, -339.5896251119744989 ) ) ;
#88726 = CARTESIAN_POINT ( 'NONE',  ( -3.412640926239523864, -298.6326408371829757, -193.3601811988871759 ) ) ;
#88727 = CARTESIAN_POINT ( 'NONE',  ( -56.94140100180641895, -287.3827073712763536, -343.3889323613226452 ) ) ;
#88728 = CARTESIAN_POINT ( 'NONE',  ( 25.32690061152271710, -274.9592647916398391, -225.5987980341190848 ) ) ;
#88729 = CARTESIAN_POINT ( 'NONE',  ( 9.870087361923538083, -294.6855003705708782, -212.4763284423190726 ) ) ;
#88730 = DIRECTION ( 'NONE',  ( 0.000000000000000000, 0.000000000000000000, 1.000000000000000000 ) ) ;
#88731 = CARTESIAN_POINT ( 'NONE',  ( 21.31550574532285580, -278.6948066931273615, -317.0979686699210447 ) ) ;
#88732 = EDGE_CURVE ( 'NONE', #5311, #16264, #48711, .T. ) ;
#88733 = CARTESIAN_POINT ( 'NONE',  ( -100.5690000889176190, -276.0045833875395260, -311.1050903652580359 ) ) ;
#88734 = EDGE_CURVE ( 'NONE', #39273, #59550, #22003, .T. ) ;
#88735 = CARTESIAN_POINT ( 'NONE',  ( 209.8616357346614905, 36.89613957940296274, 12.09245862095555601 ) ) ;
#88736 = CARTESIAN_POINT ( 'NONE',  ( -37.23404748048368162, -296.4533593876205941, -194.1603856226311393 ) ) ;
#88737 = CARTESIAN_POINT ( 'NONE',  ( -63.09882464049199058, -293.3111419126308874, -201.2018022552746288 ) ) ;
#88738 = CARTESIAN_POINT ( 'NONE',  ( -100.8021405173969072, -272.3984619785289283, -233.9734640488737796 ) ) ;
#88739 = CARTESIAN_POINT ( 'NONE',  ( -110.4752277977036385, -291.9538077196464201, -279.4272573322683684 ) ) ;
#88740 = CARTESIAN_POINT ( 'NONE',  ( -41.61852452990174100, -292.9383613026943181, -197.2008026460582641 ) ) ;
#88741 = CARTESIAN_POINT ( 'NONE',  ( -109.9270887052928032, -286.5005448722459960, -255.8926909489524633 ) ) ;
#88742 = CARTESIAN_POINT ( 'NONE',  ( -8.748681435394530581, -293.8443066618533521, -199.5017814399394354 ) ) ;
#88743 = CARTESIAN_POINT ( 'NONE',  ( -71.96417182753269515, -292.9192771186878304, -202.1221085807098348 ) ) ;
#88744 = CARTESIAN_POINT ( 'NONE',  ( -4.338558376371498326, -294.4378979190326504, -335.4888061185869219 ) ) ;
#88745 = CARTESIAN_POINT ( 'NONE',  ( 11.43478354180057366, -290.3764556504684720, -327.4022150936784783 ) ) ;
#88746 = CARTESIAN_POINT ( 'NONE',  ( -0.3735736698964021163, -282.7413115413122568, -337.9212838089801494 ) ) ;
#88747 = CARTESIAN_POINT ( 'NONE',  ( -82.09758680927073726, -295.5274530081582043, -209.4173530677898043 ) ) ;
#88748 = CARTESIAN_POINT ( 'NONE',  ( -54.96254782434196073, -285.6649382813969851, -195.4044256132371231 ) ) ;
#88749 = CARTESIAN_POINT ( 'NONE',  ( 21.97353265476693807, -276.9085197259813071, -225.0239758228853475 ) ) ;
#88750 = CARTESIAN_POINT ( 'NONE',  ( -98.42908645621132280, -283.9088561867778253, -229.6737521732676157 ) ) ;
#88751 = CARTESIAN_POINT ( 'NONE',  ( 8.972371408197739484, -286.4169884481055419, -329.4187574834333532 ) ) ;
#88752 = CARTESIAN_POINT ( 'NONE',  ( -94.02173817196339201, -277.3840602148842436, -220.0850921930528443 ) ) ;
#88753 = DIRECTION ( 'NONE',  ( 0.000000000000000000, -0.7071067811865584529, -0.7071067811865364705 ) ) ;
#88754 = CARTESIAN_POINT ( 'NONE',  ( -18.72600364087714908, -282.3136698140316980, -341.0637190268167842 ) ) ;
#88755 = CARTESIAN_POINT ( 'NONE',  ( -88.67677829477563023, -280.5554650065419082, -213.5041178221238454 ) ) ;
#88756 = CARTESIAN_POINT ( 'NONE',  ( 26.16945513870148332, -286.0404186542038474, -227.2197303735168532 ) ) ;
#88757 = CARTESIAN_POINT ( 'NONE',  ( 33.72942454330158313, -295.5823839753542188, -291.0675335834604311 ) ) ;
#88758 = CARTESIAN_POINT ( 'NONE',  ( -8.171833738087050492, -278.2765967397771192, -340.7709896753364092 ) ) ;
#88759 = CARTESIAN_POINT ( 'NONE',  ( -72.59843053132563284, -278.8241603653879679, -338.2746307413582372 ) ) ;
#88760 = CARTESIAN_POINT ( 'NONE',  ( -74.01511229425355509, -277.3874166576804896, -333.4805353166745476 ) ) ;
#88761 = CARTESIAN_POINT ( 'NONE',  ( -96.75990922141069461, -299.1768040539963067, -224.8484192260559098 ) ) ;
#88762 = CARTESIAN_POINT ( 'NONE',  ( 35.50061173354132649, -285.3306234450449210, -253.1584722225344706 ) ) ;
#88763 = CARTESIAN_POINT ( 'NONE',  ( -77.69528309073278649, -291.1840553925446784, -335.0603328796804590 ) ) ;
#88764 = CARTESIAN_POINT ( 'NONE',  ( 8.410403692695748390, -293.3294014244271466, -327.7061099492979110 ) ) ;
#88765 = ORIENTED_EDGE ( 'NONE', *, *, #86805, .F. ) ;
#88766 = CARTESIAN_POINT ( 'NONE',  ( 17.09349828530620030, -293.9151031917704131, -319.0512809942784997 ) ) ;
#88767 = ORIENTED_EDGE ( 'NONE', *, *, #19699, .F. ) ;
#88768 = CARTESIAN_POINT ( 'NONE',  ( -107.4432116647920026, -291.2318458041945632, -301.5926517945230216 ) ) ;
#88769 = CARTESIAN_POINT ( 'NONE',  ( -51.85570246182746246, -280.5130522989530277, -198.6627064667482045 ) ) ;
#88770 = CARTESIAN_POINT ( 'NONE',  ( -87.87244703221172415, -272.4249887969959900, -212.5023609096001280 ) ) ;
#88771 = CARTESIAN_POINT ( 'NONE',  ( 33.76200359271922480, -287.8293561675691308, -240.9376454224967858 ) ) ;
#88772 = CARTESIAN_POINT ( 'NONE',  ( -46.01917088447714121, -289.4924822420450141, -346.9024369035943778 ) ) ;
#88773 = CARTESIAN_POINT ( 'NONE',  ( -95.78541391206661615, -285.4997418526264710, -226.5841856324762773 ) ) ;
#88774 = CARTESIAN_POINT ( 'NONE',  ( 199.3883137936588241, 289.5528945228473958, -97.47147507470964456 ) ) ;
#88775 = CARTESIAN_POINT ( 'NONE',  ( 101.5141839819154939, 116.5281249055354067, -281.5031478140604122 ) ) ;
#88776 = CARTESIAN_POINT ( 'NONE',  ( -22.13763408965488111, -108.7303330413373033, -358.8740908389603987 ) ) ;
#88777 = CARTESIAN_POINT ( 'NONE',  ( -3.802529560586211499, -275.7949203730356658, -335.3820820254225623 ) ) ;
#88778 = CARTESIAN_POINT ( 'NONE',  ( -106.7328798081358059, -277.7872383363808240, -246.5602281572855645 ) ) ;
#88779 = CARTESIAN_POINT ( 'NONE',  ( -109.1453431151094549, -272.5721129784340064, -242.4658784311463080 ) ) ;
#88780 = CARTESIAN_POINT ( 'NONE',  ( -68.85798215598981642, -196.8429261930088217, -357.5647156207587045 ) ) ;
#88781 = CARTESIAN_POINT ( 'NONE',  ( -104.5504101214728081, -276.7609001001441129, -306.9163853536769011 ) ) ;
#88782 = CARTESIAN_POINT ( 'NONE',  ( -95.81380582698589876, -290.4298608113135742, -314.1884012829152084 ) ) ;
#88783 = CARTESIAN_POINT ( 'NONE',  ( -43.28748383492704477, -298.7818394282464283, -193.6998833367696307 ) ) ;
#88784 = CARTESIAN_POINT ( 'NONE',  ( -104.1450966862234679, -273.7000923003124058, -232.1672439187108807 ) ) ;
#88785 = CARTESIAN_POINT ( 'NONE',  ( -108.4775168079284953, -296.9350704301849646, -253.9691812503791937 ) ) ;
#88786 = ORIENTED_EDGE ( 'NONE', *, *, #57795, .T. ) ;
#88787 = LINE ( 'NONE', #74599, #19011 ) ;
#88788 = CARTESIAN_POINT ( 'NONE',  ( -108.3745125533995406, -280.1389628304403914, -296.2755176332486258 ) ) ;
#88789 = CARTESIAN_POINT ( 'NONE',  ( -10.72920906819971876, -282.2219963164582737, -342.6070668509094617 ) ) ;
#88790 = CARTESIAN_POINT ( 'NONE',  ( -104.7316011881508757, -280.0178595349979673, -241.5023704723153628 ) ) ;
#88791 = CARTESIAN_POINT ( 'NONE',  ( -110.3696597728734616, -280.5790546171008373, -249.3637104083806264 ) ) ;
#88792 = CARTESIAN_POINT ( 'NONE',  ( -110.2660113002767304, -271.1753318438110227, -259.3945063485154492 ) ) ;
#88793 = DIRECTION ( 'NONE',  ( -0.000000000000000000, 1.000000000000000000, 1.224646799147353207E-16 ) ) ;
#88794 = CARTESIAN_POINT ( 'NONE',  ( 23.68136368143023773, -281.1622719052827506, -230.2051932776869876 ) ) ;
#88795 = CARTESIAN_POINT ( 'NONE',  ( 14.78116627594697974, -277.1431220494483227, -326.8903026726130747 ) ) ;
#88796 = ADVANCED_FACE ( 'NONE', ( #79494 ), #27910, .T. ) ;
#88797 = CARTESIAN_POINT ( 'NONE',  ( 26.77908828348659753, -277.0297592129062423, -231.3578373895293225 ) ) ;
#88798 = CARTESIAN_POINT ( 'NONE',  ( 10.14556184085752832, -274.9870356540658918, -330.2915646690205449 ) ) ;
#88799 = VERTEX_POINT ( 'NONE', #71934 ) ;
#88800 = CARTESIAN_POINT ( 'NONE',  ( 60.30377782462291947, -249.1633071459562245, 21.50000000000000000 ) ) ;
#88801 = CARTESIAN_POINT ( 'NONE',  ( -32.13561320798089582, -291.3166295403516415, -197.3724573444179100 ) ) ;
#88802 = CARTESIAN_POINT ( 'NONE',  ( 38.68605035028986094, -286.7551698687362887, -258.7367498470847522 ) ) ;
#88803 = CARTESIAN_POINT ( 'NONE',  ( -34.83435733095612363, -281.2601167594040135, -344.3445815098483536 ) ) ;
#88804 = CARTESIAN_POINT ( 'NONE',  ( -3.365341808700972770, -281.1691091737433226, -335.6514324568581173 ) ) ;
#88805 = CARTESIAN_POINT ( 'NONE',  ( -92.24966424918525831, -291.8367808080635086, -321.5245189587901677 ) ) ;
#88806 = CARTESIAN_POINT ( 'NONE',  ( -2.976694331570231444, -281.7219450825382410, -205.4918192799668759 ) ) ;
#88807 = CARTESIAN_POINT ( 'NONE',  ( -90.72710357316371699, -271.2949341972904449, -217.6828554168711207 ) ) ;
#88808 = CARTESIAN_POINT ( 'NONE',  ( 27.61229810922933581, -280.4792259117083404, -310.3034920856416079 ) ) ;
#88809 = CARTESIAN_POINT ( 'NONE',  ( 22.45035533668827199, -296.1715466596770625, -315.6370581208966541 ) ) ;
#88810 = CARTESIAN_POINT ( 'NONE',  ( -96.88864188962460844, -277.4321309260640191, -223.1579851984146501 ) ) ;
#88811 = CARTESIAN_POINT ( 'NONE',  ( -76.40328641052035152, -278.2407319730143627, -332.2113035366778604 ) ) ;
#88812 = CARTESIAN_POINT ( 'NONE',  ( -112.5075799967929555, -286.5567343998617389, -270.0162600337060326 ) ) ;
#88813 = EDGE_CURVE ( 'NONE', #52100, #72640, #46314, .T. ) ;
#88814 = DIRECTION ( 'NONE',  ( 1.000000000000000000, 0.000000000000000000, 0.000000000000000000 ) ) ;
#88815 = CARTESIAN_POINT ( 'NONE',  ( -7.776612193814562701, -294.3566996850324813, -200.8113218426642561 ) ) ;
#88816 = CARTESIAN_POINT ( 'NONE',  ( 34.42289870611392644, -273.8333595626176020, -292.1964794839659021 ) ) ;
#88817 = CARTESIAN_POINT ( 'NONE',  ( -1.884345576160738389, -287.7917070601843079, -338.5295478394768907 ) ) ;
#88818 = CARTESIAN_POINT ( 'NONE',  ( -4.458513102168510933, -290.8927144961657518, -204.2778600655711898 ) ) ;
#88819 = CARTESIAN_POINT ( 'NONE',  ( -48.18343439339133027, -260.4846106489175668, -445.8398854946390202 ) ) ;
#88820 = CARTESIAN_POINT ( 'NONE',  ( -110.3961455498839968, -277.1260015906198078, -278.8301244749800958 ) ) ;
#88821 = CARTESIAN_POINT ( 'NONE',  ( -103.8857275989354463, -294.2517549774662484, -303.3826423662424645 ) ) ;
#88822 = CARTESIAN_POINT ( 'NONE',  ( -96.94884573334296363, -291.2701075784368641, -313.3521830034268305 ) ) ;
#88823 = PLANE ( 'NONE',  #50351 ) ;
#88824 = CARTESIAN_POINT ( 'NONE',  ( 36.41743059376401703, -291.7844510921906362, -250.7582041716827064 ) ) ;
#88825 = CARTESIAN_POINT ( 'NONE',  ( 32.59225633426358115, -288.8425195977143289, -246.7882066578738431 ) ) ;
#88826 = CARTESIAN_POINT ( 'NONE',  ( -81.32535161787092193, -289.7029579151109715, -208.3981256949737713 ) ) ;
#88827 = CARTESIAN_POINT ( 'NONE',  ( -42.73528288598976133, -287.4080790934755214, -196.9570818155519021 ) ) ;
#88828 = CARTESIAN_POINT ( 'NONE',  ( 140.0681712527789671, 131.0000000000000568, 11.50000000000000000 ) ) ;
#88829 = CARTESIAN_POINT ( 'NONE',  ( 34.92032093507009449, -288.5065782651537347, -281.8778965209361900 ) ) ;
#88830 = CARTESIAN_POINT ( 'NONE',  ( 0.9556996232091388155, -296.5236380136504408, -335.2588527279069694 ) ) ;
#88831 = PLANE ( 'NONE',  #17108 ) ;
#88832 = CARTESIAN_POINT ( 'NONE',  ( 37.32910831592712952, -288.5416432545086423, -253.2067829069811182 ) ) ;
#88833 = CARTESIAN_POINT ( 'NONE',  ( -100.4986056809782298, -277.1250017337118834, -229.1618528082989030 ) ) ;
#88834 = CARTESIAN_POINT ( 'NONE',  ( -35.70770212432291402, -277.3654913112496274, -347.3357499808114994 ) ) ;
#88835 = CARTESIAN_POINT ( 'NONE',  ( 26.26554225215162930, -280.6458210426333721, -226.9107153838555178 ) ) ;
#88836 = CARTESIAN_POINT ( 'NONE',  ( -87.21761982640481392, -299.3328348492395321, -214.8251887621781577 ) ) ;
#88837 = CARTESIAN_POINT ( 'NONE',  ( -87.03269670789117640, -283.3605800741293592, -214.1151700481287321 ) ) ;
#88838 = LINE ( 'NONE', #11181, #38320 ) ;
#88839 = CARTESIAN_POINT ( 'NONE',  ( -54.76000988218859078, -277.9656118216776122, -198.1452542113970594 ) ) ;
#88840 = EDGE_CURVE ( 'NONE', #92631, #9616, #64844, .T. ) ;
#88841 = CARTESIAN_POINT ( 'NONE',  ( -27.65628795172891330, -280.9291011470268131, -344.7850856453721917 ) ) ;
#88842 = DIRECTION ( 'NONE',  ( -1.000000000000000000, -0.000000000000000000, -0.000000000000000000 ) ) ;
#88843 = CARTESIAN_POINT ( 'NONE',  ( -56.76639348319081080, -275.7779308852479971, -344.2085583223964704 ) ) ;
#88844 = CARTESIAN_POINT ( 'NONE',  ( -76.00549486343447825, -297.0985246431054634, -333.1567060886927152 ) ) ;
#88845 = CARTESIAN_POINT ( 'NONE',  ( 21.36448908002214253, -281.1396278516211851, -319.7076057951762778 ) ) ;
#88846 = CARTESIAN_POINT ( 'NONE',  ( -108.8189047686954609, -297.2836689099028149, -286.3115933893948295 ) ) ;
#88847 = CARTESIAN_POINT ( 'NONE',  ( -46.82599045170345420, -275.3592330692728183, -194.5412358340066135 ) ) ;
#88848 = CARTESIAN_POINT ( 'NONE',  ( 11.56383214535435933, -274.4195517779341458, -216.0681613957420950 ) ) ;
#88849 = CARTESIAN_POINT ( 'NONE',  ( 31.33128783158213437, -295.9470949734134138, -300.5110992514311192 ) ) ;
#88850 = CARTESIAN_POINT ( 'NONE',  ( 31.42084141081734927, -287.2729416256747754, -235.7098137416566601 ) ) ;
#88851 = CARTESIAN_POINT ( 'NONE',  ( -100.6707060825276869, -277.1847302277274707, -229.0505764741986638 ) ) ;
#88852 = CARTESIAN_POINT ( 'NONE',  ( -111.2315664910461948, -290.6571907444517251, -248.6980698734735142 ) ) ;
#88853 = CARTESIAN_POINT ( 'NONE',  ( -101.8560815859694912, -289.1385020599338986, -305.1284889189296337 ) ) ;
#88854 = CARTESIAN_POINT ( 'NONE',  ( 35.51102487947743924, -291.7814474102494273, -288.2327787385098645 ) ) ;
#88855 = ORIENTED_EDGE ( 'NONE', *, *, #29222, .F. ) ;
#88856 = CARTESIAN_POINT ( 'NONE',  ( 199.8307606272909993, 66.96248882677818415, 8.111107179099439790 ) ) ;
#88857 = CARTESIAN_POINT ( 'NONE',  ( -110.3067169247177617, -290.1209022522170926, -265.7254710942496558 ) ) ;
#88858 = CARTESIAN_POINT ( 'NONE',  ( 165.2494399300530290, -11.64849832608277325, 13.00000000000000178 ) ) ;
#88859 = CARTESIAN_POINT ( 'NONE',  ( -93.75499265852629094, -286.2050562525767532, -218.2220763943071233 ) ) ;
#88860 = CARTESIAN_POINT ( 'NONE',  ( 22.93080827219366569, -291.9729086501291135, -222.8001783812340761 ) ) ;
#88861 = CARTESIAN_POINT ( 'NONE',  ( 37.07265087823328287, -283.0916572806831937, -288.1878883651515366 ) ) ;
#88862 = CARTESIAN_POINT ( 'NONE',  ( -2.430530605334753957, -282.4099737776977008, -334.4863285145546570 ) ) ;
#88863 = CARTESIAN_POINT ( 'NONE',  ( -98.23397174162738565, -297.1815556975413415, -223.2109593512317645 ) ) ;
#88864 = CARTESIAN_POINT ( 'NONE',  ( 13.82809076201679410, -276.1034196780390744, -217.6079571519227329 ) ) ;
#88865 = CARTESIAN_POINT ( 'NONE',  ( 9.909078090675439654, -290.7263531353383996, -212.5081523982934186 ) ) ;
#88866 = CARTESIAN_POINT ( 'NONE',  ( 9.751543461422579995, -273.5119272719235823, -213.9975088387745075 ) ) ;
#88867 = EDGE_LOOP ( 'NONE', ( #81868, #37216, #46734, #21267 ) ) ;
#88868 = DIRECTION ( 'NONE',  ( -1.000000000000000000, -0.000000000000000000, -0.000000000000000000 ) ) ;
#88869 = CARTESIAN_POINT ( 'NONE',  ( 18.84738437295753499, -288.7896401982644079, -221.5338614257992447 ) ) ;
#88870 = CARTESIAN_POINT ( 'NONE',  ( -113.8137513682103048, -297.7128243467723792, -263.9102007318877554 ) ) ;
#88871 = CARTESIAN_POINT ( 'NONE',  ( -97.44446937599246894, -285.7827541865613625, -228.7270930540353220 ) ) ;
#88872 = CARTESIAN_POINT ( 'NONE',  ( -71.47702456065704268, -276.5507692157809174, -339.1186618588110946 ) ) ;
#88873 = CARTESIAN_POINT ( 'NONE',  ( -25.04592317527918865, -292.8564399407803762, -194.4524448585611083 ) ) ;
#88874 = CARTESIAN_POINT ( 'NONE',  ( 32.88831327036422181, -286.0601276719452244, -298.9269845772616918 ) ) ;
#88875 = CARTESIAN_POINT ( 'NONE',  ( 37.07721418950464454, -294.1319605999963755, -290.0479024683017428 ) ) ;
#88876 = CARTESIAN_POINT ( 'NONE',  ( -3.630268338155516528, -292.8432786772083887, -205.5874593432622248 ) ) ;
#88877 = DIRECTION ( 'NONE',  ( -0.000000000000000000, -0.000000000000000000, 1.000000000000000000 ) ) ;
#88878 = CARTESIAN_POINT ( 'NONE',  ( 194.5881128153457098, -26.00396092263537540, 10.00000000000000178 ) ) ;
#88879 = CARTESIAN_POINT ( 'NONE',  ( 179.9264549738192045, 251.0413663519439638, -164.3140871016692302 ) ) ;
#88880 = VECTOR ( 'NONE', #80975, 1000.000000000000000 ) ;
#88881 = CARTESIAN_POINT ( 'NONE',  ( -113.4617613181934104, -286.1484793220961933, -264.3225573714302641 ) ) ;
#88882 = CARTESIAN_POINT ( 'NONE',  ( -119.3990491898856732, -276.0523547857346784, -270.3284710469131937 ) ) ;
#88883 = VERTEX_POINT ( 'NONE', #44408 ) ;
#88884 = CARTESIAN_POINT ( 'NONE',  ( -64.18128941018478884, -282.3310806301104776, -338.5803419666793275 ) ) ;
#88885 = CARTESIAN_POINT ( 'NONE',  ( -99.63515215918701529, -277.6184400750412351, -315.6081964417838890 ) ) ;
#88886 = CARTESIAN_POINT ( 'NONE',  ( 30.62744788623446013, -283.1388142597120918, -238.9285078651561207 ) ) ;
#88887 = CARTESIAN_POINT ( 'NONE',  ( 195.4986669975991163, 276.4997496711473559, -124.9842105939577550 ) ) ;
#88888 = CARTESIAN_POINT ( 'NONE',  ( -27.46637479669298187, -281.5038967305731603, -346.1840128394300109 ) ) ;
#88889 = CARTESIAN_POINT ( 'NONE',  ( 37.08994003297814146, -285.6533146669509620, -276.6443312285128400 ) ) ;
#88890 = CARTESIAN_POINT ( 'NONE',  ( -10.80283907500293239, -276.2548437375539265, -199.3405717903672212 ) ) ;
#88891 = CARTESIAN_POINT ( 'NONE',  ( -82.39283207028553591, -296.1783962990252235, -327.9441698562145575 ) ) ;
#88892 = CARTESIAN_POINT ( 'NONE',  ( 18.86448784015252400, -291.5687922042390596, -223.0102160551004999 ) ) ;
#88893 = CARTESIAN_POINT ( 'NONE',  ( -107.4797216441901497, -278.7989106373614732, -302.0179575458226964 ) ) ;
#88894 = CARTESIAN_POINT ( 'NONE',  ( -7.507651691420418771, -276.6497464500808405, -336.9864101311050035 ) ) ;
#88895 = CARTESIAN_POINT ( 'NONE',  ( -96.70558283186353776, -274.2864917608053474, -221.7873316402643979 ) ) ;
#88896 = CARTESIAN_POINT ( 'NONE',  ( -97.69419777710729136, -276.8373959859873139, -317.6799148689655112 ) ) ;
#88897 = CARTESIAN_POINT ( 'NONE',  ( -112.7898643569077706, -271.0197764341763218, -296.3298465391314949 ) ) ;
#88898 = CARTESIAN_POINT ( 'NONE',  ( 35.34119778660562616, -273.7902327606373092, -288.9104785550536576 ) ) ;
#88899 = CARTESIAN_POINT ( 'NONE',  ( 26.03326136535111957, -295.5441535339220422, -313.0485932946843377 ) ) ;
#88900 = CARTESIAN_POINT ( 'NONE',  ( 161.2494399300530290, 8.542400036368780647, 9.974999999999996092 ) ) ;
#88901 = CARTESIAN_POINT ( 'NONE',  ( 6.757860130087521178, -59.91093500391586701, -350.7441993381422094 ) ) ;
#88902 = CARTESIAN_POINT ( 'NONE',  ( -108.6694543714356342, -285.8548569264742696, -253.3784093648953046 ) ) ;
#88903 = CARTESIAN_POINT ( 'NONE',  ( -76.21990380771146079, -285.3240072837634784, -335.7096263600781754 ) ) ;
#88904 = CARTESIAN_POINT ( 'NONE',  ( -67.58230202556876520, -284.9931624474995715, -203.8073903229725374 ) ) ;
#88905 = CARTESIAN_POINT ( 'NONE',  ( -107.1954135973051478, -277.2668652467139054, -246.3946725530375090 ) ) ;
#88906 = CARTESIAN_POINT ( 'NONE',  ( -48.49120873738111470, -285.0560121238178226, -343.7542643658638326 ) ) ;
#88907 = CARTESIAN_POINT ( 'NONE',  ( -11.48188368726873421, -278.8749462662771066, -201.3000623646655356 ) ) ;
#88908 = CARTESIAN_POINT ( 'NONE',  ( 15.83151367117474884, -277.3562006887751750, -320.8272988161273247 ) ) ;
#88909 = PLANE ( 'NONE',  #79091 ) ;
#88910 = CARTESIAN_POINT ( 'NONE',  ( -69.52371186195338737, -274.1090396393505557, -204.7691477221953846 ) ) ;
#88911 = CARTESIAN_POINT ( 'NONE',  ( 36.44179548098264831, -282.0848744854619667, -248.8627559860956922 ) ) ;
#88912 = CARTESIAN_POINT ( 'NONE',  ( 36.92396448756610283, -281.7919726319168490, -250.2079891368959466 ) ) ;
#88913 = ORIENTED_EDGE ( 'NONE', *, *, #43587, .T. ) ;
#88914 = EDGE_LOOP ( 'NONE', ( #71494, #8660, #81104, #49398 ) ) ;
#88915 = CARTESIAN_POINT ( 'NONE',  ( 201.2104617360081704, 15.00000000000001421, -10.00000000000000178 ) ) ;
#88916 = CARTESIAN_POINT ( 'NONE',  ( 27.62696303721163460, -288.8947537111146744, -231.2807827248599608 ) ) ;
#88917 = CARTESIAN_POINT ( 'NONE',  ( -108.3291417091857483, -295.9830231565314875, -252.6071791420796444 ) ) ;
#88918 = CARTESIAN_POINT ( 'NONE',  ( -79.53155137547516063, -290.8472859879211114, -206.0064973715321912 ) ) ;
#88919 = CARTESIAN_POINT ( 'NONE',  ( 3.987589279887013394, -286.9645246735206001, -331.4357337758737003 ) ) ;
#88921 = CARTESIAN_POINT ( 'NONE',  ( -27.95593153036177014, -290.4126423992381660, -196.8938529580860290 ) ) ;
#88920 = CARTESIAN_POINT ( 'NONE',  ( -23.69355535698458937, -287.4491842155395602, -342.7257690642406374 ) ) ;
#88922 = VECTOR ( 'NONE', #57815, 1000.000000000000000 ) ;
#88923 = CARTESIAN_POINT ( 'NONE',  ( 7.155533116394992454, -287.8785201098037305, -211.9263149023260837 ) ) ;
#88924 = CARTESIAN_POINT ( 'NONE',  ( -101.8976323444736067, -276.0402284905114243, -308.6406606397787868 ) ) ;
#88925 = CARTESIAN_POINT ( 'NONE',  ( -12.50395016080192079, -287.1344564334690972, -342.4547717811892653 ) ) ;
#88926 = CARTESIAN_POINT ( 'NONE',  ( 1.678163828981969585, -288.5741197337143262, -206.3107404273475822 ) ) ;
#88927 = CARTESIAN_POINT ( 'NONE',  ( -8.949799626988914625, -286.6815371351957538, -339.9733785600924989 ) ) ;
#88928 = CARTESIAN_POINT ( 'NONE',  ( 22.78477784429863817, -283.0742888330206597, -312.1727801715958321 ) ) ;
#88929 = CARTESIAN_POINT ( 'NONE',  ( -111.9896770885892892, -292.4338905133129742, -279.6047144693898758 ) ) ;
#88930 = CARTESIAN_POINT ( 'NONE',  ( 82.14611277039779225, -299.7700546811713593, -193.3686474501289752 ) ) ;
#88931 = CARTESIAN_POINT ( 'NONE',  ( 156.1711927057158960, 19.99999999999999645, -14.66327707482027343 ) ) ;
#88932 = CARTESIAN_POINT ( 'NONE',  ( -67.62325405607694506, -299.5782460777497249, -201.0786314493083466 ) ) ;
#88933 = CARTESIAN_POINT ( 'NONE',  ( -3.064406095733742230, -279.7143613247351368, -205.7120192547222075 ) ) ;
#88934 = CARTESIAN_POINT ( 'NONE',  ( 34.66163133151410136, -279.2817490396534481, -249.3725280162958313 ) ) ;
#88935 = CARTESIAN_POINT ( 'NONE',  ( 38.19662078253288939, -292.9266175371049030, -284.5077044167479130 ) ) ;
#88936 = CARTESIAN_POINT ( 'NONE',  ( -110.8902728777928104, -270.8997547113571613, -262.0797256406096949 ) ) ;
#88937 = CARTESIAN_POINT ( 'NONE',  ( -43.34716752544354534, -275.2084350363414273, -344.5584801961832113 ) ) ;
#88938 = CARTESIAN_POINT ( 'NONE',  ( -101.8925294664317818, -297.3909674363411568, -305.4956296271776637 ) ) ;
#88939 = CARTESIAN_POINT ( 'NONE',  ( 211.1232656141943949, 0.000000000000000000, -7.000000000000000000 ) ) ;
#88940 = CARTESIAN_POINT ( 'NONE',  ( -105.0781370570270212, -271.5878690097644039, -234.8860797186684977 ) ) ;
#88941 = CARTESIAN_POINT ( 'NONE',  ( -109.3920874496307505, -294.4839957000004347, -294.5006229458841744 ) ) ;
#88942 = CARTESIAN_POINT ( 'NONE',  ( 28.00148218434232206, -294.5208031388833092, -236.5137629783081081 ) ) ;
#88943 = EDGE_CURVE ( 'NONE', #32344, #59329, #1792, .T. ) ;
#88944 = CARTESIAN_POINT ( 'NONE',  ( 0.000000000000000000, 0.000000000000000000, -7.500000000000000000 ) ) ;
#88945 = CARTESIAN_POINT ( 'NONE',  ( 22.71465362648927666, -293.7736288401085289, -228.5558450256074252 ) ) ;
#88946 = CYLINDRICAL_SURFACE ( 'NONE', #92863, 4.999999999999993783 ) ;
#88948 = CARTESIAN_POINT ( 'NONE',  ( -70.93079939629407704, -295.5082394444463034, -335.1884683187761880 ) ) ;
#88947 = CARTESIAN_POINT ( 'NONE',  ( -110.1257916780892288, -282.8242249227566845, -250.6490328987756584 ) ) ;
#88949 = CARTESIAN_POINT ( 'NONE',  ( -0.3754383079739446183, -282.5746584240786774, -337.9223040882120017 ) ) ;
#88950 = CARTESIAN_POINT ( 'NONE',  ( 25.07699156534556195, -282.8988926531994252, -227.6879300705891751 ) ) ;
#88951 = CARTESIAN_POINT ( 'NONE',  ( -0.9757982256029431589, -286.1882168460589355, -202.5137490549639665 ) ) ;
#88952 = CARTESIAN_POINT ( 'NONE',  ( -104.5017180638011780, -288.1156943239396355, -303.3696080153376897 ) ) ;
#88953 = CARTESIAN_POINT ( 'NONE',  ( 37.46200943825348162, -280.2222228821135559, -285.4313797505948287 ) ) ;
#88954 = CARTESIAN_POINT ( 'NONE',  ( 7.239277753003735327, -285.3586758794743332, -211.8692464614710218 ) ) ;
#88955 = CARTESIAN_POINT ( 'NONE',  ( 34.77707165466368622, -286.8049805708795930, -296.5995496413343631 ) ) ;
#88956 = DIRECTION ( 'NONE',  ( -1.000000000000000000, 0.000000000000000000, 0.000000000000000000 ) ) ;
#88957 = CARTESIAN_POINT ( 'NONE',  ( -55.98594972239119727, -296.8962684004010839, -341.8201798380377454 ) ) ;
#88958 = CARTESIAN_POINT ( 'NONE',  ( -98.32213417274323319, -279.3592432990945440, -316.4259674619277121 ) ) ;
#88960 = CARTESIAN_POINT ( 'NONE',  ( -14.29818105165613851, -280.0259368854701165, -201.0178091678392320 ) ) ;
#88959 = CARTESIAN_POINT ( 'NONE',  ( 14.33207142501330189, -292.3501251635682934, -325.2084345463456998 ) ) ;
#88961 = CARTESIAN_POINT ( 'NONE',  ( 38.06147555064014654, -293.5229232442350735, -254.6964678723220743 ) ) ;
#88962 = CARTESIAN_POINT ( 'NONE',  ( -98.17016135182011283, -283.2398949312868126, -225.4508232507635910 ) ) ;
#88963 = ADVANCED_FACE ( 'NONE', ( #16465 ), #11069, .F. ) ;
#88964 = CARTESIAN_POINT ( 'NONE',  ( -23.28802108270996385, -278.8727487968201331, -344.0854311336198066 ) ) ;
#88965 = CARTESIAN_POINT ( 'NONE',  ( -55.87439129982982422, -294.3552969704064139, -341.2652627127403662 ) ) ;
#88966 = CARTESIAN_POINT ( 'NONE',  ( -112.0379053944801768, -270.6595642647937439, -261.9643719324537869 ) ) ;
#88967 = VERTEX_POINT ( 'NONE', #28035 ) ;
#88968 = CARTESIAN_POINT ( 'NONE',  ( 189.9243309297870610, 249.5000000000000568, 25.22542485937348644 ) ) ;
#88969 = CARTESIAN_POINT ( 'NONE',  ( 29.23731304862225144, -283.0825329258510692, -236.4962975892529187 ) ) ;
#88970 = CARTESIAN_POINT ( 'NONE',  ( -90.45628115878515985, -295.3371272909204208, -320.6019992849436449 ) ) ;
#88971 = FACE_OUTER_BOUND ( 'NONE', #54804, .T. ) ;
#88972 = CARTESIAN_POINT ( 'NONE',  ( -4.771743288812454686, -271.9809262143061233, -202.8022627189028810 ) ) ;
#88973 = CARTESIAN_POINT ( 'NONE',  ( 17.98045540647651208, -274.0169670309741150, -216.9591437254168227 ) ) ;
#88974 = CARTESIAN_POINT ( 'NONE',  ( 37.80264608039183116, -288.6863896394444282, -255.9866438424649004 ) ) ;
#88975 = CARTESIAN_POINT ( 'NONE',  ( -95.76959809118696398, -289.7709401463851009, -314.1447577236851885 ) ) ;
#88976 = CARTESIAN_POINT ( 'NONE',  ( -49.27304965492940880, -281.4174497217426278, -197.6400711708310780 ) ) ;
#88977 = CARTESIAN_POINT ( 'NONE',  ( -33.77295167291392630, -299.8575643442301839, -196.3466902990889480 ) ) ;
#88978 = CARTESIAN_POINT ( 'NONE',  ( -1.760218938713778103, -279.3297746532766155, -206.1654117262181387 ) ) ;
#88979 = VERTEX_POINT ( 'NONE', #58657 ) ;
#88980 = CARTESIAN_POINT ( 'NONE',  ( -95.08507037260577022, -273.0752038527181185, -219.4228887502702889 ) ) ;
#88981 = CARTESIAN_POINT ( 'NONE',  ( -88.94613321542732365, -293.2408207419115342, -216.6400982332671958 ) ) ;
#88982 = CARTESIAN_POINT ( 'NONE',  ( 210.3152560301384142, 38.32590481451376263, 10.50000000000000000 ) ) ;
#88983 = CARTESIAN_POINT ( 'NONE',  ( -92.63903346802047167, -291.8838965779881391, -222.5479650440476576 ) ) ;
#88984 = CARTESIAN_POINT ( 'NONE',  ( 204.6539576904058606, 293.9636489450775230, 7.999911143031724237 ) ) ;
#88985 = CARTESIAN_POINT ( 'NONE',  ( 38.47558134905143135, -291.6913957687910397, -270.3344259365086373 ) ) ;
#88986 = AXIS2_PLACEMENT_3D ( 'NONE', #73138, #8264, #79770 ) ;
#88987 = CARTESIAN_POINT ( 'NONE',  ( -88.13740443269240643, -296.9841929698825425, -217.8321256704426787 ) ) ;
#88988 = CARTESIAN_POINT ( 'NONE',  ( -23.40286736638519471, -135.2391364535880882, 21.50000000000000000 ) ) ;
#88989 = CARTESIAN_POINT ( 'NONE',  ( -113.4971117055489458, -292.1328764332700416, -265.5589269568019404 ) ) ;
#88990 = CARTESIAN_POINT ( 'NONE',  ( -37.30987171927208124, -291.5519495502701375, -350.3611179825600175 ) ) ;
#88991 = CARTESIAN_POINT ( 'NONE',  ( 36.80929706736761631, -289.4177090014545115, -259.9010040630292337 ) ) ;
#88992 = CARTESIAN_POINT ( 'NONE',  ( 16.90987495324426249, -274.2768656518007901, -321.9052255770073430 ) ) ;
#88993 = CARTESIAN_POINT ( 'NONE',  ( -5.943406564085075949, -276.3882997010356917, -202.8669599930505854 ) ) ;
#88994 = CARTESIAN_POINT ( 'NONE',  ( 20.47947571497060082, -290.9813570680049111, -223.4578407859972629 ) ) ;
#88995 = CARTESIAN_POINT ( 'NONE',  ( -68.19162427447430730, -281.5117552822066500, -201.1473388294926394 ) ) ;
#88996 = ORIENTED_EDGE ( 'NONE', *, *, #68227, .F. ) ;
#88997 = CARTESIAN_POINT ( 'NONE',  ( -37.54913156659663542, -282.4034372162573732, -343.4752039615685248 ) ) ;
#88998 = CARTESIAN_POINT ( 'NONE',  ( -112.4879710563360646, -279.4387047987073061, -285.7403489314895637 ) ) ;
#88999 = CARTESIAN_POINT ( 'NONE',  ( -58.39244300135827359, -282.1131718468973304, -344.0700837830037244 ) ) ;
#89000 = CARTESIAN_POINT ( 'NONE',  ( -25.79349925096121154, -277.8497269309163471, -346.2522193642396928 ) ) ;
#89001 =( NAMED_UNIT ( * ) PLANE_ANGLE_UNIT ( ) SI_UNIT ( $, .RADIAN. ) );
#89002 = CARTESIAN_POINT ( 'NONE',  ( 4.466951834050296277, -276.1248781915052177, -206.4647109676793661 ) ) ;
#89003 = CARTESIAN_POINT ( 'NONE',  ( -82.13390479932378696, -275.9090924074130271, -214.2458315076590907 ) ) ;
#89004 = ORIENTED_EDGE ( 'NONE', *, *, #11508, .T. ) ;
#89005 = CARTESIAN_POINT ( 'NONE',  ( -111.3319384704930144, -298.3948235769625512, -282.6267317070384024 ) ) ;
#89006 = CARTESIAN_POINT ( 'NONE',  ( -96.80131151909365883, -291.0346430138194478, -313.2421241204754097 ) ) ;
#89007 = CARTESIAN_POINT ( 'NONE',  ( -8.117444987741034623, -274.6876243966412972, -339.0611314265431702 ) ) ;
#89008 = CARTESIAN_POINT ( 'NONE',  ( -90.86859175108209286, -291.5587617839245809, -324.3688312723742797 ) ) ;
#89009 = CARTESIAN_POINT ( 'NONE',  ( 8.919751889117721433, -292.0546183495225705, -213.6935933227010196 ) ) ;
#89010 = CARTESIAN_POINT ( 'NONE',  ( 39.57866391366307113, -287.0389200822090174, -268.6924362445642487 ) ) ;
#89011 = LINE ( 'NONE', #61113, #88397 ) ;
#89012 = CARTESIAN_POINT ( 'NONE',  ( -106.9348766131871002, -282.6269174695443667, -295.0741621083533346 ) ) ;
#89013 = CARTESIAN_POINT ( 'NONE',  ( -74.13695478333539768, -291.4070181083353077, -334.8503762310150478 ) ) ;
#89014 = CARTESIAN_POINT ( 'NONE',  ( -88.15874389209710671, -283.8048174201608731, -216.9913155242664118 ) ) ;
#89015 = CARTESIAN_POINT ( 'NONE',  ( -16.79981573297656183, -281.6382884988377100, -199.7971437296610304 ) ) ;
#89016 = CARTESIAN_POINT ( 'NONE',  ( -7.001856394474613943, -289.6049309251496311, -340.8899532228931548 ) ) ;
#89017 = CARTESIAN_POINT ( 'NONE',  ( -93.99221414101330652, -279.6970203542263107, -224.2231975272558486 ) ) ;
#89018 = CARTESIAN_POINT ( 'NONE',  ( -33.54362477606380111, -290.8938937194533878, -193.8524038200291102 ) ) ;
#89019 = CARTESIAN_POINT ( 'NONE',  ( 7.441504646455879168, -287.4482362903297599, -207.8566342549276271 ) ) ;
#89020 = CARTESIAN_POINT ( 'NONE',  ( -35.15627248501470348, -286.5712146376627629, -193.4405678638204620 ) ) ;
#89021 = CARTESIAN_POINT ( 'NONE',  ( -56.31685506482937598, -283.4702369714810288, -340.8518514133517670 ) ) ;
#89022 = ORIENTED_EDGE ( 'NONE', *, *, #81029, .T. ) ;
#89023 = DIRECTION ( 'NONE',  ( 0.000000000000000000, 0.9681751575201845705, -0.2502735790305594121 ) ) ;
#89024 = CARTESIAN_POINT ( 'NONE',  ( -14.26557690012690571, -294.2085436395337865, -198.1409721019649908 ) ) ;
#89025 = CARTESIAN_POINT ( 'NONE',  ( 36.97693710062746675, -292.4663230252966173, -288.5828449617946490 ) ) ;
#89026 = CARTESIAN_POINT ( 'NONE',  ( -40.52796209958852103, -276.1519098718168834, -343.5395719886201960 ) ) ;
#89027 = CARTESIAN_POINT ( 'NONE',  ( -111.5215286208136831, -296.1571202498999469, -249.8995459237500825 ) ) ;
#89028 = CARTESIAN_POINT ( 'NONE',  ( 33.29921152532156015, -291.7547796665170949, -249.1953707357953647 ) ) ;
#89029 = CARTESIAN_POINT ( 'NONE',  ( -98.02690410923855779, -294.2093275297238506, -312.7318629853191965 ) ) ;
#89030 = CARTESIAN_POINT ( 'NONE',  ( -57.78015008514533690, -292.9874789368114989, -199.8139769177015523 ) ) ;
#89031 = CARTESIAN_POINT ( 'NONE',  ( 34.63046150111802035, -294.8149008589218170, -284.2979047282708507 ) ) ;
#89032 = DIRECTION ( 'NONE',  ( 1.124465274301078034E-16, 1.000000000000000000, 0.000000000000000000 ) ) ;
#89033 = CARTESIAN_POINT ( 'NONE',  ( -0.3836499478214713266, -292.5618946530282187, -335.8292066949369428 ) ) ;
#89034 = CARTESIAN_POINT ( 'NONE',  ( -111.8716590566565827, -298.6656906885456237, -261.5311516812699892 ) ) ;
#89035 = CARTESIAN_POINT ( 'NONE',  ( 35.19508572739544405, -288.6272964308869291, -280.5432750523608547 ) ) ;
#89036 = CARTESIAN_POINT ( 'NONE',  ( -8.490545543306549092, -278.6562992066666880, -339.9884439290153750 ) ) ;
#89037 = CARTESIAN_POINT ( 'NONE',  ( -80.01777561677815243, -276.4102706235498772, -334.0391402479016847 ) ) ;
#89038 = CARTESIAN_POINT ( 'NONE',  ( -21.36785844198816520, -273.6004387738561832, -195.1404481632973216 ) ) ;
#89039 = CARTESIAN_POINT ( 'NONE',  ( 35.47889646411434228, -279.4314672105670638, -254.8576533790206611 ) ) ;
#89040 = CARTESIAN_POINT ( 'NONE',  ( -94.62301593661122467, -276.2648946786512738, -320.6133943071902195 ) ) ;
#89041 = EDGE_CURVE ( 'NONE', #64853, #63422, #87049, .T. ) ;
#89042 = CARTESIAN_POINT ( 'NONE',  ( -86.83435579610332411, -294.4429971548641447, -324.6908567253473166 ) ) ;
#89043 = CARTESIAN_POINT ( 'NONE',  ( -80.48561767965726688, -275.4679794506541270, -208.9504190740165654 ) ) ;
#89044 = CARTESIAN_POINT ( 'NONE',  ( 94.76649097485585571, -300.5504365972934124, -197.1811787442501895 ) ) ;
#89045 = AXIS2_PLACEMENT_3D ( 'NONE', #45614, #82077, #75002 ) ;
#89046 = CARTESIAN_POINT ( 'NONE',  ( 152.4536156746142410, 250.5000000000000568, 14.50000000000000000 ) ) ;
#89048 = CARTESIAN_POINT ( 'NONE',  ( 23.05352618220267757, -274.8149576618262699, -229.3336146960308213 ) ) ;
#89047 = CARTESIAN_POINT ( 'NONE',  ( -97.72655729366621813, -287.9592395543290877, -315.4610167626807424 ) ) ;
#89049 = CARTESIAN_POINT ( 'NONE',  ( 21.48902162509775948, -288.2214277197815022, -320.0395456750707126 ) ) ;
#89050 = CARTESIAN_POINT ( 'NONE',  ( -112.3534138238100581, -274.6237131139723715, -264.7881570981465416 ) ) ;
#89051 = CARTESIAN_POINT ( 'NONE',  ( -87.74309054937427277, -293.7581209913942075, -325.6759285460489082 ) ) ;
#89052 = CARTESIAN_POINT ( 'NONE',  ( -16.19611019935852525, -281.9828348384396008, -344.2879501172409960 ) ) ;
#89053 = DIRECTION ( 'NONE',  ( 0.000000000000000000, 0.000000000000000000, 1.000000000000000000 ) ) ;
#89054 = CARTESIAN_POINT ( 'NONE',  ( -31.07612613150118008, -280.9729540490905606, -345.1496949390449913 ) ) ;
#89055 = LINE ( 'NONE', #66840, #72528 ) ;
#89056 = CARTESIAN_POINT ( 'NONE',  ( -105.0635442129329249, -289.7262168134909075, -241.9290601960868798 ) ) ;
#89057 = CARTESIAN_POINT ( 'NONE',  ( -105.2526652636348388, -282.2949645513912174, -300.3438845652318037 ) ) ;
#89058 = CARTESIAN_POINT ( 'NONE',  ( 160.5350683151633291, 275.0000000000000568, 20.22542485937379908 ) ) ;
#89059 = CYLINDRICAL_SURFACE ( 'NONE', #86631, 28.04691768583012035 ) ;
#89060 = CARTESIAN_POINT ( 'NONE',  ( -111.7775110829350496, -288.4340928881269406, -279.5432035619452904 ) ) ;
#89061 = CARTESIAN_POINT ( 'NONE',  ( -76.95306132551249334, -275.0310312293645438, -208.2189598626128770 ) ) ;
#89062 = CARTESIAN_POINT ( 'NONE',  ( -18.99852665487965453, -284.0263308966909790, -344.7900962463539827 ) ) ;
#89064 = CARTESIAN_POINT ( 'NONE',  ( -49.42152875011135649, -285.8939914235181163, -198.3160243476656035 ) ) ;
#89063 = CARTESIAN_POINT ( 'NONE',  ( -52.23736057404353517, -271.9428611369167470, -196.2304855949892897 ) ) ;
#89065 = CARTESIAN_POINT ( 'NONE',  ( 34.47224366850698374, -277.1884237229274959, -286.4849789586215252 ) ) ;
#89066 = CARTESIAN_POINT ( 'NONE',  ( -3.784312916378991254, -277.4003258414024344, -335.3726822687901290 ) ) ;
#89067 = EDGE_CURVE ( 'NONE', #88967, #31159, #8329, .T. ) ;
#89068 = CARTESIAN_POINT ( 'NONE',  ( 18.31685722878774669, -284.2537714571871561, -320.7076551815846415 ) ) ;
#89069 = ORIENTED_EDGE ( 'NONE', *, *, #34302, .T. ) ;
#89070 = CARTESIAN_POINT ( 'NONE',  ( 82.18044315312610593, -297.0737527268180997, -195.3611179825600175 ) ) ;
#89071 = CARTESIAN_POINT ( 'NONE',  ( -96.51278045906006753, -295.7225305243627531, -319.6541610964886218 ) ) ;
#89072 = CARTESIAN_POINT ( 'NONE',  ( 19.90738172459068522, -288.8668893720492292, -222.4414281454273237 ) ) ;
#89073 = DIRECTION ( 'NONE',  ( 0.000000000000000000, 1.000000000000000000, 0.000000000000000000 ) ) ;
#89074 = CARTESIAN_POINT ( 'NONE',  ( -2.659677404128736544, -292.1237833571632336, -342.4524372437778652 ) ) ;
#89075 = CARTESIAN_POINT ( 'NONE',  ( -110.3765361387372508, -277.1751910412162374, -293.9288914978216667 ) ) ;
#89076 = CARTESIAN_POINT ( 'NONE',  ( -19.55353988847230085, -290.6769569888583078, -196.2121803957554675 ) ) ;
#89077 = CARTESIAN_POINT ( 'NONE',  ( -108.7048720136494637, -286.3126878066204881, -251.9761933834853664 ) ) ;
#89078 = CARTESIAN_POINT ( 'NONE',  ( -66.48912589719131461, -281.4252898030412666, -202.3149305971311378 ) ) ;
#89079 = CARTESIAN_POINT ( 'NONE',  ( -87.37790602093332382, -286.7958743964533710, -212.5417322798815292 ) ) ;
#89080 = CARTESIAN_POINT ( 'NONE',  ( 9.050542965701078302, -284.4160441822205030, -329.3575937758101873 ) ) ;
#89081 = CARTESIAN_POINT ( 'NONE',  ( 14.88473760354887077, -276.5070719399959103, -327.0145973572528533 ) ) ;
#89082 = CARTESIAN_POINT ( 'NONE',  ( -36.43375537722128854, -296.0836820433624439, -195.7166176068193693 ) ) ;
#89083 = CARTESIAN_POINT ( 'NONE',  ( -96.81607964772888408, -279.0426150368054437, -221.4346015617686589 ) ) ;
#89084 = CARTESIAN_POINT ( 'NONE',  ( -33.74903269729592381, -300.0176166704152365, -195.9199233160248070 ) ) ;
#89085 = FACE_BOUND ( 'NONE', #93090, .T. ) ;
#89086 = FACE_OUTER_BOUND ( 'NONE', #19815, .T. ) ;
#89087 = CARTESIAN_POINT ( 'NONE',  ( -34.78709695009811753, -296.2233993800615508, -194.5971099260036681 ) ) ;
#89088 = DIRECTION ( 'NONE',  ( -1.000000000000000000, -0.000000000000000000, -0.000000000000000000 ) ) ;
#89089 = CARTESIAN_POINT ( 'NONE',  ( -59.21939297366914445, -276.8507648694993009, -340.0701919779118612 ) ) ;
#89090 = CARTESIAN_POINT ( 'NONE',  ( -78.64046109227615489, -274.7141447982739919, -205.8442902490384085 ) ) ;
#89091 = CARTESIAN_POINT ( 'NONE',  ( -3.008861917010193121, -281.6684481228682557, -339.0348577077450045 ) ) ;
#89092 = CARTESIAN_POINT ( 'NONE',  ( 18.60604968294815720, -289.9940104596424817, -318.8922244758015268 ) ) ;
#89093 = CARTESIAN_POINT ( 'NONE',  ( -110.9583840544445792, -298.3283046013095259, -250.0835621705315646 ) ) ;
#89094 = CARTESIAN_POINT ( 'NONE',  ( -94.34577856536363072, -297.0591112527845894, -321.5523650232364616 ) ) ;
#89095 = CARTESIAN_POINT ( 'NONE',  ( -14.30564727747010245, -294.3517285953693658, -199.1616187305430969 ) ) ;
#89096 = CARTESIAN_POINT ( 'NONE',  ( 35.86385932082201577, -279.3514737473630021, -254.7766081567943672 ) ) ;
#89097 = CARTESIAN_POINT ( 'NONE',  ( -39.77227371968641023, -281.9415748106957267, -195.9480388870738068 ) ) ;
#89098 = CARTESIAN_POINT ( 'NONE',  ( -80.54429421823286361, -295.5411283990863467, -209.7405764209321148 ) ) ;
#89099 = CARTESIAN_POINT ( 'NONE',  ( -104.7341832124922121, -286.6175268055682750, -234.6855518047958640 ) ) ;
#89100 = CARTESIAN_POINT ( 'NONE',  ( 25.95603822349596612, -286.9791478944686673, -307.4428225247563660 ) ) ;
#89101 = CARTESIAN_POINT ( 'NONE',  ( -111.9029649914729987, -274.3533271841375836, -284.1314302805552643 ) ) ;
#89102 = ORIENTED_EDGE ( 'NONE', *, *, #12755, .T. ) ;
#89103 = CARTESIAN_POINT ( 'NONE',  ( -7.169427026500634348, -287.2387890439902662, -340.5766734897804326 ) ) ;
#89104 = CARTESIAN_POINT ( 'NONE',  ( 15.99281042147283927, -286.5013927213132661, -220.4676463104188997 ) ) ;
#89105 = ORIENTED_EDGE ( 'NONE', *, *, #48291, .T. ) ;
#89106 = CARTESIAN_POINT ( 'NONE',  ( -13.50490926704745220, -283.8293986118143266, -343.2535038032067973 ) ) ;
#89107 = CARTESIAN_POINT ( 'NONE',  ( -16.63873118405083673, -274.6602557992504217, -200.2835814982489637 ) ) ;
#89108 = CARTESIAN_POINT ( 'NONE',  ( -39.19040363413979833, -290.9498279827822671, -193.6795311270805939 ) ) ;
#89109 = CARTESIAN_POINT ( 'NONE',  ( 39.42797708798034506, -282.2697415680290760, -275.6456175562059343 ) ) ;
#89110 = CARTESIAN_POINT ( 'NONE',  ( 31.38848345220755220, -282.6417463983408993, -237.0904182216780214 ) ) ;
#89111 = CARTESIAN_POINT ( 'NONE',  ( 29.74555639785409866, -282.3765678172347293, -308.2195247415301083 ) ) ;
#89113 = CARTESIAN_POINT ( 'NONE',  ( -39.70123265173319993, -280.0217311979517376, -197.3867410028045697 ) ) ;
#89112 = AXIS2_PLACEMENT_3D ( 'NONE', #59296, #15742, #44602 ) ;
#89114 = CARTESIAN_POINT ( 'NONE',  ( 17.36665895637873192, -291.6952119285918457, -314.0302885647153062 ) ) ;
#89115 = CARTESIAN_POINT ( 'NONE',  ( 204.1738562182569865, 295.5636489450776594, -54.00000000003635847 ) ) ;
#89116 = ORIENTED_EDGE ( 'NONE', *, *, #66220, .T. ) ;
#89117 = CARTESIAN_POINT ( 'NONE',  ( 37.47532963158331398, -277.5322144758942500, -268.7989139723576955 ) ) ;
#89118 = CARTESIAN_POINT ( 'NONE',  ( 193.2878968112678706, 279.2590251747096772, -125.7166890413514722 ) ) ;
#89119 = CARTESIAN_POINT ( 'NONE',  ( 26.55706396811117642, -279.0517069514310720, -231.6759935962187740 ) ) ;
#89120 = CARTESIAN_POINT ( 'NONE',  ( -108.2718346551197897, -296.1344180275618214, -252.6234966121301966 ) ) ;
#89121 = CARTESIAN_POINT ( 'NONE',  ( 8.819018865565656284, -292.1735131886179602, -208.7420833378092482 ) ) ;
#89122 = CARTESIAN_POINT ( 'NONE',  ( 122.1069166415481675, 147.2784711292074746, -260.4370888795256178 ) ) ;
#89124 = CARTESIAN_POINT ( 'NONE',  ( -66.66544725388411052, -287.8425458187088566, -338.1398679533321570 ) ) ;
#89123 = CARTESIAN_POINT ( 'NONE',  ( -29.12011971014949907, -296.7279165062974471, -193.9522893961830619 ) ) ;
#89125 = CARTESIAN_POINT ( 'NONE',  ( -101.2174250889782883, -297.9002549988333044, -308.2876331127136496 ) ) ;
#89126 = CARTESIAN_POINT ( 'NONE',  ( -77.33135434598976587, -286.8190466279287421, -208.6397927785881734 ) ) ;
#89127 = ORIENTED_EDGE ( 'NONE', *, *, #78996, .F. ) ;
#89128 = CARTESIAN_POINT ( 'NONE',  ( 26.29112085824403522, -293.9248192799931303, -227.3294859851417300 ) ) ;
#89129 = CARTESIAN_POINT ( 'NONE',  ( -96.62842956409112105, -285.6413192482182239, -227.6423237980168324 ) ) ;
#89130 = CARTESIAN_POINT ( 'NONE',  ( -70.54299056466236095, -296.4189938815864593, -201.3271912938886601 ) ) ;
#89131 = CARTESIAN_POINT ( 'NONE',  ( 6.395908296376385138, -293.4327452979607074, -207.1853280833397832 ) ) ;
#89132 = CARTESIAN_POINT ( 'NONE',  ( 39.37923181266253891, -293.9721349783073379, -264.5796384800373175 ) ) ;
#89133 = CARTESIAN_POINT ( 'NONE',  ( -31.86923610701748188, -289.1479977434713646, -343.2063299429950121 ) ) ;
#89134 = ORIENTED_EDGE ( 'NONE', *, *, #36204, .T. ) ;
#89135 = CARTESIAN_POINT ( 'NONE',  ( 157.4787282879766508, 15.38390992556648484, 9.006389530800610999 ) ) ;
#89136 = CARTESIAN_POINT ( 'NONE',  ( -37.62717321976086282, -299.9090227726960620, -194.5968520648300739 ) ) ;
#89137 = CARTESIAN_POINT ( 'NONE',  ( -85.54640313737958479, -272.1970675487955305, -210.8269653872123115 ) ) ;
#89138 = EDGE_CURVE ( 'NONE', #93327, #2870, #43146, .T. ) ;
#89139 = CARTESIAN_POINT ( 'NONE',  ( 35.58783707006125496, -280.5159429295842415, -263.1400257029466729 ) ) ;
#89140 = ORIENTED_EDGE ( 'NONE', *, *, #41260, .T. ) ;
#89141 = VERTEX_POINT ( 'NONE', #81335 ) ;
#89142 = CARTESIAN_POINT ( 'NONE',  ( -39.96713745691275221, -276.5919328570835205, -347.2678273719408821 ) ) ;
#89143 = B_SPLINE_CURVE_WITH_KNOTS ( 'NONE', 3,
 ( #74724, #31633, #87965, #900, #1814, #9365 ),
 .UNSPECIFIED., .F., .F.,
 ( 4, 2, 4 ),
 ( 0.002739916521960775175, 0.004109700271224535004, 0.005479484020488295699 ),
 .UNSPECIFIED. ) ;
#89144 = CARTESIAN_POINT ( 'NONE',  ( -51.69734273985348949, -272.2654494168249926, -197.9184609823952599 ) ) ;
#89145 = CARTESIAN_POINT ( 'NONE',  ( -65.30296695795047413, -281.5431656365564095, -201.5931527769666900 ) ) ;
#89146 = CARTESIAN_POINT ( 'NONE',  ( -35.10373894340448686, -275.1633340817014641, -344.5625803161958061 ) ) ;
#89147 = CARTESIAN_POINT ( 'NONE',  ( -58.03132532065379934, -298.9838966303013308, -199.9404540175274576 ) ) ;
#89148 = CARTESIAN_POINT ( 'NONE',  ( -107.4251961852876036, -273.7759867085004544, -248.9337898722736497 ) ) ;
#89149 = CARTESIAN_POINT ( 'NONE',  ( -107.6291489229502787, -297.7724677766868240, -299.9274261750562687 ) ) ;
#89150 = CARTESIAN_POINT ( 'NONE',  ( 14.90517502534841654, -272.8044653843860488, -216.0594528355629222 ) ) ;
#89151 = CARTESIAN_POINT ( 'NONE',  ( 31.63899721509572061, -294.5268713193605095, -294.7110019337296762 ) ) ;
#89152 = CARTESIAN_POINT ( 'NONE',  ( -28.01381287923609520, -290.7474573783241567, -197.3143058046228759 ) ) ;
#89153 = DIRECTION ( 'NONE',  ( -0.000000000000000000, -1.000000000000000000, -0.000000000000000000 ) ) ;
#89154 = CARTESIAN_POINT ( 'NONE',  ( -87.05065085714393547, -278.2149734987142438, -329.1551525006119050 ) ) ;
#89155 = CARTESIAN_POINT ( 'NONE',  ( -110.1889313985378891, -272.7906691278161588, -264.9155664882928249 ) ) ;
#89156 = CARTESIAN_POINT ( 'NONE',  ( -81.29204363170602221, -282.3203840553159694, -333.0487810411650003 ) ) ;
#89157 = CARTESIAN_POINT ( 'NONE',  ( -33.50238207237256916, -297.0041143795465359, -345.4424805667892997 ) ) ;
#89158 = DIRECTION ( 'NONE',  ( 0.000000000000000000, 1.000000000000000000, 0.000000000000000000 ) ) ;
#89159 = CARTESIAN_POINT ( 'NONE',  ( -78.47583977116995868, -282.8189502839505849, -330.8638805842288662 ) ) ;
#89160 = CARTESIAN_POINT ( 'NONE',  ( -37.34047897176560582, -281.0519445899233233, -345.5405427088986698 ) ) ;
#89161 = CARTESIAN_POINT ( 'NONE',  ( 27.27552746444510134, -274.6049851869653935, -305.6810719347033114 ) ) ;
#89162 = CARTESIAN_POINT ( 'NONE',  ( 22.28025937386015798, -282.9292973018240787, -224.8406054699628385 ) ) ;
#89163 = FACE_OUTER_BOUND ( 'NONE', #64106, .T. ) ;
#89164 = CARTESIAN_POINT ( 'NONE',  ( 160.5350683151633291, 275.0000000000000568, 15.22542485937381329 ) ) ;
#89165 = CARTESIAN_POINT ( 'NONE',  ( -69.77257422985915980, -272.0321742184402183, -201.3926766148003082 ) ) ;
#89166 = CARTESIAN_POINT ( 'NONE',  ( -98.94795921592940147, -279.9690896066185246, -313.4273143414797573 ) ) ;
#89167 = DIRECTION ( 'NONE',  ( 1.000000000000000000, 0.000000000000000000, 0.000000000000000000 ) ) ;
#89168 = CARTESIAN_POINT ( 'NONE',  ( -36.60451131642521716, -287.9814853994026294, -194.7919155840614280 ) ) ;
#89169 = CARTESIAN_POINT ( 'NONE',  ( -112.1113976243086512, -288.4685871173598457, -276.8565991352125479 ) ) ;
#89170 = DIRECTION ( 'NONE',  ( -0.000000000000000000, -0.000000000000000000, 1.000000000000000000 ) ) ;
#89171 = CARTESIAN_POINT ( 'NONE',  ( -96.41080045292979150, -295.9546228856151515, -226.7741858827006638 ) ) ;
#89172 = CARTESIAN_POINT ( 'NONE',  ( 16.89752369082219374, -286.4093274500694406, -321.1213341725231771 ) ) ;
#89173 = CARTESIAN_POINT ( 'NONE',  ( 164.1991770243031681, 231.0496910105122765, -188.4318802409405009 ) ) ;
#89174 = CARTESIAN_POINT ( 'NONE',  ( -104.3069074748270424, -294.9995364145539725, -236.4718762833143728 ) ) ;
#89175 = CARTESIAN_POINT ( 'NONE',  ( 37.42503783968690811, -286.2245244606437495, -285.6137455731060868 ) ) ;
#89176 = CARTESIAN_POINT ( 'NONE',  ( 27.14814136406135958, -282.6669905289319331, -234.4793571876790281 ) ) ;
#89177 = CARTESIAN_POINT ( 'NONE',  ( -85.47797780271102397, -281.9472403570058532, -329.1562945102817821 ) ) ;
#89178 = CARTESIAN_POINT ( 'NONE',  ( -110.3062927386186090, -290.5053502780018562, -273.9089570091852011 ) ) ;
#89179 = CARTESIAN_POINT ( 'NONE',  ( 36.27639718255356627, -282.9537464046198352, -268.5511185908077323 ) ) ;
#89180 = CARTESIAN_POINT ( 'NONE',  ( 27.00190924546948423, -282.8290374801839562, -305.1821125013399865 ) ) ;
#89181 = CARTESIAN_POINT ( 'NONE',  ( -81.86019147425703579, -291.6352680838302831, -331.1600548831598871 ) ) ;
#89182 = CIRCLE ( 'NONE', #7564, 1.000000000000000888 ) ;
#89183 = CARTESIAN_POINT ( 'NONE',  ( -51.80269555526009384, -298.0388498572103799, -194.6768926596968754 ) ) ;
#89184 = CARTESIAN_POINT ( 'NONE',  ( -23.59831476659382332, -286.9578083656605259, -344.7138382283853275 ) ) ;
#89185 = CARTESIAN_POINT ( 'NONE',  ( 37.94539020592240064, -275.3493823729453425, -254.1478096292735813 ) ) ;
#89186 = CARTESIAN_POINT ( 'NONE',  ( 17.93970792771565215, -294.8284324881998373, -220.1274613679968297 ) ) ;
#89187 = LINE ( 'NONE', #38066, #27311 ) ;
#89188 = CARTESIAN_POINT ( 'NONE',  ( -4.771743288812468897, -285.1233781216987495, -337.9199732462171255 ) ) ;
#89189 = CARTESIAN_POINT ( 'NONE',  ( 27.50124386707673096, -274.0589582039850711, -308.3798112600483137 ) ) ;
#89190 = LINE ( 'NONE', #86060, #82103 ) ;
#89191 = CARTESIAN_POINT ( 'NONE',  ( -112.5962212367760884, -295.1042994807838227, -258.3120809002741112 ) ) ;
#89192 = CARTESIAN_POINT ( 'NONE',  ( -95.76001158828768212, -292.7802930512403350, -225.2640969777207545 ) ) ;
#89193 = CARTESIAN_POINT ( 'NONE',  ( 17.36735049440609302, -274.2082127979599591, -221.8009234343717537 ) ) ;
#89194 = CARTESIAN_POINT ( 'NONE',  ( -109.6149368061015394, -291.8832950641826756, -284.8230446680153705 ) ) ;
#89195 = CARTESIAN_POINT ( 'NONE',  ( -60.34420535741542579, -292.6878378045312843, -200.7788218554516675 ) ) ;
#89197 = EDGE_CURVE ( 'NONE', #55580, #64501, #20440, .T. ) ;
#89196 = CARTESIAN_POINT ( 'NONE',  ( -96.59041443171668107, -286.9263711691420440, -226.0038878054861300 ) ) ;
#89198 = CARTESIAN_POINT ( 'NONE',  ( -58.79080470984933271, -293.2052653879501349, -197.0225728364294184 ) ) ;
#89199 = CARTESIAN_POINT ( 'NONE',  ( -16.77538196780092150, -293.6275899025542913, -196.6703802411635706 ) ) ;
#89200 = CARTESIAN_POINT ( 'NONE',  ( -6.766841554349227295, -294.4725500585760756, -336.6497144960601418 ) ) ;
#89201 = CARTESIAN_POINT ( 'NONE',  ( 20.17971498485812631, -288.8871543923269769, -222.2132946541026683 ) ) ;
#89202 = CARTESIAN_POINT ( 'NONE',  ( 39.71043018815907999, -281.7134170121874490, -269.9281493017942921 ) ) ;
#89203 = CARTESIAN_POINT ( 'NONE',  ( -113.1056199888904246, -270.7278972505659453, -267.5160169140336848 ) ) ;
#89204 = CARTESIAN_POINT ( 'NONE',  ( -113.8193925979152823, -284.4974467066709281, -261.4077633604953235 ) ) ;
#89205 = CARTESIAN_POINT ( 'NONE',  ( -6.812378358426629532, -278.6293184499240851, -338.4772490969438650 ) ) ;
#89206 = EDGE_CURVE ( 'NONE', #19058, #25647, #1344, .T. ) ;
#89207 = CARTESIAN_POINT ( 'NONE',  ( -100.7518526126499268, -282.8425306519972082, -307.3243844230472064 ) ) ;
#89208 = CARTESIAN_POINT ( 'NONE',  ( 12.92580990593084955, -284.7533051498782015, -214.6301393697086439 ) ) ;
#89209 = CARTESIAN_POINT ( 'NONE',  ( -97.83179356605262456, -276.0740864099831242, -316.0031827095970129 ) ) ;
#89210 = CARTESIAN_POINT ( 'NONE',  ( 144.2857639756989272, -299.5541904835127980, -195.3611179825600175 ) ) ;
#89211 = CARTESIAN_POINT ( 'NONE',  ( -94.33695462814144150, -283.4141784266712421, -316.0923928214343164 ) ) ;
#89212 = CARTESIAN_POINT ( 'NONE',  ( -112.6089210739956172, -279.9371536216752929, -256.0482047769293104 ) ) ;
#89213 = CARTESIAN_POINT ( 'NONE',  ( 14.09812876186115460, -285.8120431873110192, -213.3094072744691232 ) ) ;
#89214 = CARTESIAN_POINT ( 'NONE',  ( -7.560276213182880234, -296.4164503735974563, -338.1321056981893207 ) ) ;
#89215 = CARTESIAN_POINT ( 'NONE',  ( -98.15255043508705057, -279.5340711093290906, -316.3007241443307862 ) ) ;
#89216 = CARTESIAN_POINT ( 'NONE',  ( -4.055898082227022527, -275.7970864155691970, -201.4601768748777602 ) ) ;
#89217 = CARTESIAN_POINT ( 'NONE',  ( -97.65002509215020154, -277.8132089877212252, -311.4939022858058593 ) ) ;
#89218 = CARTESIAN_POINT ( 'NONE',  ( -104.6999236257464929, -274.9574716888434978, -238.1941080688048089 ) ) ;
#89219 = CARTESIAN_POINT ( 'NONE',  ( 36.07802732820382374, -285.7391356277951786, -284.9038503817458263 ) ) ;
#89220 = CARTESIAN_POINT ( 'NONE',  ( -54.30350269748556258, -290.8664875480821479, -344.7034651329357757 ) ) ;
#89221 = CARTESIAN_POINT ( 'NONE',  ( 19.92665673810715887, -293.1164649939644846, -316.1475025698185277 ) ) ;
#89222 = EDGE_LOOP ( 'NONE', ( #35187, #29901, #66247 ) ) ;
#89223 = CARTESIAN_POINT ( 'NONE',  ( -57.65675450785669653, -291.4493696423519964, -200.1698916260998544 ) ) ;
#89224 = ORIENTED_EDGE ( 'NONE', *, *, #41709, .T. ) ;
#89225 = CARTESIAN_POINT ( 'NONE',  ( -9.662020185674874639, -289.7785226143348041, -341.8826380169214190 ) ) ;
#89226 = CARTESIAN_POINT ( 'NONE',  ( -104.5390227901078077, -279.5896702800640128, -241.5789621403748981 ) ) ;
#89227 = CARTESIAN_POINT ( 'NONE',  ( -113.0820860847279334, -295.6246724429631740, -258.2411397662218064 ) ) ;
#89228 = CARTESIAN_POINT ( 'NONE',  ( 30.03823944251314515, -287.7217438255673301, -233.1931772616851788 ) ) ;
#89229 = CARTESIAN_POINT ( 'NONE',  ( 20.26810290458961461, -287.1928976206273774, -219.2250679843489820 ) ) ;
#89230 = CARTESIAN_POINT ( 'NONE',  ( -110.1164926366131880, -284.8063995113890883, -276.3542025018491586 ) ) ;
#89231 = CARTESIAN_POINT ( 'NONE',  ( 153.5330400557857899, 207.2306735197480521, -217.2871232403230408 ) ) ;
#89232 = CARTESIAN_POINT ( 'NONE',  ( -114.2273710279701078, -271.6425061313379388, -283.9426671196157486 ) ) ;
#89233 = CARTESIAN_POINT ( 'NONE',  ( 160.2329485493519883, 218.0567712857002505, -202.3360275596398310 ) ) ;
#89234 = CARTESIAN_POINT ( 'NONE',  ( -70.53517925836121094, -276.6987027068850011, -335.5592365956222807 ) ) ;
#89235 = CARTESIAN_POINT ( 'NONE',  ( -78.81816936395172490, -276.5457176553536556, -330.8706733254643382 ) ) ;
#89236 = CARTESIAN_POINT ( 'NONE',  ( -58.11182902165122499, -273.4577624967550946, -196.1818530974302064 ) ) ;
#89237 = CARTESIAN_POINT ( 'NONE',  ( -46.06860329632770146, -156.0334151122670789, -362.4947484422432353 ) ) ;
#89238 = CARTESIAN_POINT ( 'NONE',  ( -23.04756887807354104, -275.5579478501494464, -345.5746246977481633 ) ) ;
#89239 = ORIENTED_EDGE ( 'NONE', *, *, #37291, .F. ) ;
#89240 = CARTESIAN_POINT ( 'NONE',  ( -71.19570957382865117, -290.0040374636821525, -335.1200932830141710 ) ) ;
#89241 = CARTESIAN_POINT ( 'NONE',  ( -3.509142013160955198, -299.2684613794370989, -193.5181099910766420 ) ) ;
#89242 = CARTESIAN_POINT ( 'NONE',  ( 35.05613052537813701, -286.0675696423022600, -257.4325782390631048 ) ) ;
#89243 = CARTESIAN_POINT ( 'NONE',  ( -31.92121794078451558, -298.6106578659084789, -193.4222168341995598 ) ) ;
#89244 = CARTESIAN_POINT ( 'NONE',  ( -3.141877431436876922, -294.7536983832067676, -334.8543124455514430 ) ) ;
#89245 = VERTEX_POINT ( 'NONE', #10296 ) ;
#89246 = CARTESIAN_POINT ( 'NONE',  ( -12.31953985451911571, -278.6494661464399201, -341.7126099922298295 ) ) ;
#89247 = AXIS2_PLACEMENT_3D ( 'NONE', #44381, #58616, #87457 ) ;
#89248 = CARTESIAN_POINT ( 'NONE',  ( 37.80406799353948344, -281.2672373653826980, -286.9337652042881928 ) ) ;
#89249 = CARTESIAN_POINT ( 'NONE',  ( -96.33360121650478902, -279.0241393913663046, -313.9043519444060735 ) ) ;
#89250 = CARTESIAN_POINT ( 'NONE',  ( -67.28834189182781245, -279.1996351473921436, -340.1978752268828430 ) ) ;
#89251 = AXIS2_PLACEMENT_3D ( 'NONE', #28671, #21555, #65612 ) ;
#89252 = CARTESIAN_POINT ( 'NONE',  ( -50.03788076293803755, -296.4616822065447650, -197.8753820549776208 ) ) ;
#89253 = DIRECTION ( 'NONE',  ( 0.000000000000000000, 0.000000000000000000, 1.000000000000000000 ) ) ;
#89254 = CARTESIAN_POINT ( 'NONE',  ( -11.74513701306266533, -280.5614762424342530, -201.9423488261171826 ) ) ;
#89255 = CARTESIAN_POINT ( 'NONE',  ( -15.83238294099916565, -275.1262065567587456, -196.5393191141591274 ) ) ;
#89256 = CARTESIAN_POINT ( 'NONE',  ( -75.43933256193851378, -275.5446726038809970, -205.6979167472532879 ) ) ;
#89257 = CARTESIAN_POINT ( 'NONE',  ( 28.57838494012721142, -274.6337537995642037, -309.0024000047148434 ) ) ;
#89258 = DIRECTION ( 'NONE',  ( -0.000000000000000000, -1.000000000000000000, -0.000000000000000000 ) ) ;
#89259 = CARTESIAN_POINT ( 'NONE',  ( -108.2624889632463407, -289.9865443180370335, -252.3423510929827671 ) ) ;
#89260 = CARTESIAN_POINT ( 'NONE',  ( -113.0381311379151441, -283.7275029288752535, -284.1948195845827740 ) ) ;
#89261 = CARTESIAN_POINT ( 'NONE',  ( 26.01516603460677146, -279.2714225129893180, -232.0010455128486626 ) ) ;
#89262 = EDGE_CURVE ( 'NONE', #82501, #33611, #14447, .T. ) ;
#89264 = CARTESIAN_POINT ( 'NONE',  ( -105.9147152372098617, -283.0148254242084249, -241.2622719470993218 ) ) ;
#89263 = CARTESIAN_POINT ( 'NONE',  ( -1.664645030088065525, -279.1096136531650700, -205.9986859479635939 ) ) ;
#89265 = CARTESIAN_POINT ( 'NONE',  ( 8.326975155597839517, -290.4277979600607296, -329.9184816361126877 ) ) ;
#89266 = CARTESIAN_POINT ( 'NONE',  ( -41.08670985611363591, -281.2090489958015382, -197.0596486410636601 ) ) ;
#89267 = CARTESIAN_POINT ( 'NONE',  ( -78.32198314248179827, -208.3160119463293540, -357.0358029796702226 ) ) ;
#89268 = CARTESIAN_POINT ( 'NONE',  ( -85.61149910830741305, -282.1072274449032307, -329.3226895339803946 ) ) ;
#89269 = CARTESIAN_POINT ( 'NONE',  ( 5.493186313578874547, -296.4728186258708433, -331.9887953628137893 ) ) ;
#89270 = CARTESIAN_POINT ( 'NONE',  ( -113.1979372780986495, -276.8484108683283011, -265.9108037149667894 ) ) ;
#89271 = CARTESIAN_POINT ( 'NONE',  ( -92.07860617456877605, -285.8317855451488185, -321.8959928985557326 ) ) ;
#89272 = CARTESIAN_POINT ( 'NONE',  ( 113.5000000000000568, -296.0521521680024080, -537.7509286889328450 ) ) ;
#89273 = CARTESIAN_POINT ( 'NONE',  ( -14.32873870440845998, -294.2682721463203848, -198.3359395594098373 ) ) ;
#89274 = CARTESIAN_POINT ( 'NONE',  ( 34.81526441261742377, -273.8157396195682622, -290.8622293634348352 ) ) ;
#89275 = CARTESIAN_POINT ( 'NONE',  ( -15.44965522456295304, -285.5255348815132947, -196.6519379049713336 ) ) ;
#89276 = CARTESIAN_POINT ( 'NONE',  ( -77.67552561989909066, -289.9004922040765564, -208.5580198783569870 ) ) ;
#89277 = CARTESIAN_POINT ( 'NONE',  ( -43.32131299890800591, -270.7287516391538134, -432.8764281593785199 ) ) ;
#89278 = CARTESIAN_POINT ( 'NONE',  ( 27.19182294630997987, -274.7150657474394393, -305.6337505060192825 ) ) ;
#89279 = CARTESIAN_POINT ( 'NONE',  ( -26.04238081450513320, -293.0463313764469149, -343.7313494206164819 ) ) ;
#89280 = CARTESIAN_POINT ( 'NONE',  ( -110.1912367172305238, -291.9994528402514220, -260.2779411251291890 ) ) ;
#89281 = DIRECTION ( 'NONE',  ( -0.000000000000000000, -0.000000000000000000, -1.000000000000000000 ) ) ;
#89282 = CARTESIAN_POINT ( 'NONE',  ( 36.78184658245078253, -292.2614082364067940, -288.5377528565972511 ) ) ;
#89283 = CARTESIAN_POINT ( 'NONE',  ( 20.12544109847344487, -288.5044723385692578, -224.0380988027518754 ) ) ;
#89284 = CARTESIAN_POINT ( 'NONE',  ( -7.340910553020178142, -286.9039742318146864, -340.1886818209501939 ) ) ;
#89285 = CARTESIAN_POINT ( 'NONE',  ( 25.44407166193702352, -288.4527954958793430, -231.9772440623835905 ) ) ;
#89286 = CARTESIAN_POINT ( 'NONE',  ( 139.6539576904058606, 131.4142135623731633, 11.08578643762690596 ) ) ;
#89287 = CARTESIAN_POINT ( 'NONE',  ( 12.27279899838196719, -289.1433789065411588, -324.1980180626495667 ) ) ;
#89288 = CARTESIAN_POINT ( 'NONE',  ( -11.59497176040268585, -296.6985292006157238, -341.2367715873217549 ) ) ;
#89289 = DIRECTION ( 'NONE',  ( -0.000000000000000000, 0.000000000000000000, -1.000000000000000000 ) ) ;
#89290 = CARTESIAN_POINT ( 'NONE',  ( 35.57452106130069325, -289.0540008635130107, -293.8394783572065876 ) ) ;
#89291 = CARTESIAN_POINT ( 'NONE',  ( -48.30959273996408854, -275.2703946139339450, -345.1737519845937641 ) ) ;
#89292 = CARTESIAN_POINT ( 'NONE',  ( -37.12276323269292533, -277.3827256421054699, -347.3527179268110672 ) ) ;
#89293 = CARTESIAN_POINT ( 'NONE',  ( -95.88696434765996912, -278.8934138845136204, -220.3589133636309896 ) ) ;
#89294 = CARTESIAN_POINT ( 'NONE',  ( -67.50663542476954149, -299.6344075758300391, -202.0688476716320849 ) ) ;
#89295 = CARTESIAN_POINT ( 'NONE',  ( -101.3019709135993196, -283.0784820380062570, -231.0948318536653687 ) ) ;
#89296 = CARTESIAN_POINT ( 'NONE',  ( -48.18343439339133027, -253.0206516614774728, -472.6442049081569508 ) ) ;
#89297 = CARTESIAN_POINT ( 'NONE',  ( -92.19379891267740845, -277.3971346584839353, -220.3399950438537473 ) ) ;
#89298 = CARTESIAN_POINT ( 'NONE',  ( -11.41787826056794941, -280.7144261537449097, -340.7935265535185749 ) ) ;
#89299 = FACE_OUTER_BOUND ( 'NONE', #61232, .T. ) ;
#89300 = CARTESIAN_POINT ( 'NONE',  ( -71.28003470809869668, -275.9719929266736358, -338.7050804172317271 ) ) ;
#89301 = CARTESIAN_POINT ( 'NONE',  ( -108.8524076124180624, -298.3056018870816501, -252.5069712928713557 ) ) ;
#89302 = CARTESIAN_POINT ( 'NONE',  ( -50.05585669711159369, -282.1309440562471877, -346.0444198705970962 ) ) ;
#89303 = CARTESIAN_POINT ( 'NONE',  ( -90.22404417707016933, -298.2228564754190643, -219.6242813242226930 ) ) ;
#89304 = CARTESIAN_POINT ( 'NONE',  ( -89.28585022951898509, -298.6546698380873295, -214.1190290492262420 ) ) ;
#89305 = CARTESIAN_POINT ( 'NONE',  ( -83.20057052580550305, -273.0704165689758156, -213.5363743181828227 ) ) ;
#89306 = CARTESIAN_POINT ( 'NONE',  ( 36.02931961972848285, -295.7527175194100550, -285.9693311777512008 ) ) ;
#89307 = CARTESIAN_POINT ( 'NONE',  ( 27.44594658703308099, -288.2658312085144985, -312.0714616590236687 ) ) ;
#89308 = CARTESIAN_POINT ( 'NONE',  ( -14.63671863922444416, -278.4238582371012285, -198.2382476489446219 ) ) ;
#89309 = CARTESIAN_POINT ( 'NONE',  ( -88.64790453915287571, -291.1886615846689210, -212.9444532116343396 ) ) ;
#89310 = ADVANCED_FACE ( 'NONE', ( #46739 ), #4606, .T. ) ;
#89311 = CARTESIAN_POINT ( 'NONE',  ( -8.135642908902326553, -287.7188683449310815, -337.5749475652958154 ) ) ;
#89312 = CARTESIAN_POINT ( 'NONE',  ( -11.80951754809005827, -290.3842436653737877, -199.7862589130446622 ) ) ;
#89313 = ORIENTED_EDGE ( 'NONE', *, *, #57049, .F. ) ;
#89314 = CARTESIAN_POINT ( 'NONE',  ( -90.78337343436103879, -230.3218577325732781, -348.1307343985224634 ) ) ;
#89315 = CARTESIAN_POINT ( 'NONE',  ( 29.47880164817205895, -287.4586038427289054, -300.0333400375871520 ) ) ;
#89316 = DIRECTION ( 'NONE',  ( -0.9437085149785860994, 0.3307782319877048405, 0.000000000000000000 ) ) ;
#89317 = TOROIDAL_SURFACE ( 'NONE', #137, 24.50000000000000355, 0.5000000000000000000 ) ;
#89318 = CARTESIAN_POINT ( 'NONE',  ( -101.2166761104080450, -284.9301972209697169, -313.0335533777206365 ) ) ;
#89319 = CARTESIAN_POINT ( 'NONE',  ( 37.83771883147780812, -292.8056006635608810, -285.8812719355368017 ) ) ;
#89320 = CARTESIAN_POINT ( 'NONE',  ( 37.38747727860152992, -283.0744659985058433, -286.8182728805620059 ) ) ;
#89321 = CARTESIAN_POINT ( 'NONE',  ( -42.93503437815949297, -282.9578896327762436, -343.1966056410627743 ) ) ;
#89322 = CARTESIAN_POINT ( 'NONE',  ( -112.6051595215457297, -296.3487891690641618, -286.6218584370516282 ) ) ;
#89323 = CARTESIAN_POINT ( 'NONE',  ( 9.788588059070718828, -276.0317715011957489, -213.9031813598016356 ) ) ;
#89324 = CARTESIAN_POINT ( 'NONE',  ( 36.10603311812947425, -291.3995699396595001, -256.9753611624163909 ) ) ;
#89325 = CARTESIAN_POINT ( 'NONE',  ( 11.82382920683898675, -273.5478975554822227, -215.7960532026001204 ) ) ;
#89326 = ORIENTED_EDGE ( 'NONE', *, *, #48099, .F. ) ;
#89327 = DIRECTION ( 'NONE',  ( 0.000000000000000000, 0.000000000000000000, 1.000000000000000000 ) ) ;
#89328 = CARTESIAN_POINT ( 'NONE',  ( 17.94401428159016021, -288.7721194915838510, -220.4942875993742177 ) ) ;
#89329 = CARTESIAN_POINT ( 'NONE',  ( -65.47724550899314977, -296.4911564513986946, -341.7187018202444619 ) ) ;
#89330 = CARTESIAN_POINT ( 'NONE',  ( -100.4850125505834768, -284.6987206026236663, -307.1960845805738245 ) ) ;
#89331 = CARTESIAN_POINT ( 'NONE',  ( 37.00785565434606639, -274.8507165745961629, -289.4651429160776388 ) ) ;
#89332 = CARTESIAN_POINT ( 'NONE',  ( 38.50711987932479019, -294.3631000611373452, -283.1007048759943814 ) ) ;
#89333 = CARTESIAN_POINT ( 'NONE',  ( 33.90274207322666911, -286.0243618211891885, -296.2921983274355853 ) ) ;
#89334 = CARTESIAN_POINT ( 'NONE',  ( 38.83034196164573615, -293.7419011236542019, -258.8876476171137710 ) ) ;
#89335 = CARTESIAN_POINT ( 'NONE',  ( -84.69551565326854359, -290.0589458497315718, -326.0129575035743983 ) ) ;
#89336 = CARTESIAN_POINT ( 'NONE',  ( 113.5000000000000568, -298.0521521680024080, -540.3336712212508246 ) ) ;
#89337 = LINE ( 'NONE', #52902, #72030 ) ;
#89338 = CARTESIAN_POINT ( 'NONE',  ( 184.9457000461858911, 260.3766601266518137, -151.0449398723506818 ) ) ;
#89339 = CARTESIAN_POINT ( 'NONE',  ( -89.42725907388245332, -286.8548561084268158, -214.5236326855343805 ) ) ;
#89340 = CARTESIAN_POINT ( 'NONE',  ( -2.602324593224659921, -277.9809262143061233, -198.2974183793908196 ) ) ;
#89341 = VERTEX_POINT ( 'NONE', #45811 ) ;
#89342 = CARTESIAN_POINT ( 'NONE',  ( -70.36643853568060081, -282.4183491188379662, -335.8243182341236093 ) ) ;
#89343 = CARTESIAN_POINT ( 'NONE',  ( -84.85666301551164281, -277.3535353680069875, -330.9934676387686068 ) ) ;
#89344 = CARTESIAN_POINT ( 'NONE',  ( 37.52081958642644111, -283.5285420719779381, -268.5135187135390993 ) ) ;
#89345 = CARTESIAN_POINT ( 'NONE',  ( -97.16215191512969795, -248.5819615950344144, -333.1096569481321126 ) ) ;
#89346 = CARTESIAN_POINT ( 'NONE',  ( -30.28749668335335343, -281.5392940485725717, -346.4455743865487989 ) ) ;
#89347 = CARTESIAN_POINT ( 'NONE',  ( 36.91312325076634693, -285.4739472930680222, -262.7408813532246086 ) ) ;
#89348 = CARTESIAN_POINT ( 'NONE',  ( -91.30617101582433293, -275.1548882005277505, -217.1808456871632131 ) ) ;
#89349 = CARTESIAN_POINT ( 'NONE',  ( -67.31472652107376575, -295.9484789945013858, -337.0052044219577851 ) ) ;
#89350 = EDGE_LOOP ( 'NONE', ( #35911, #53883, #60868, #79741, #40856 ) ) ;
#89351 = CARTESIAN_POINT ( 'NONE',  ( -38.89129835274776781, -290.7171322168924235, -196.8843037843466846 ) ) ;
#89352 = CARTESIAN_POINT ( 'NONE',  ( -75.27868253275025268, -278.1955923387690177, -337.2498177208484549 ) ) ;
#89353 = CARTESIAN_POINT ( 'NONE',  ( 34.37350040502551707, -275.3722757485521129, -256.7255023933661278 ) ) ;
#89354 = CARTESIAN_POINT ( 'NONE',  ( 30.98117113246196297, -274.0220486065021532, -235.5261101369746370 ) ) ;
#89355 = FACE_OUTER_BOUND ( 'NONE', #49464, .T. ) ;
#89356 = CARTESIAN_POINT ( 'NONE',  ( -0.5964661703469381626, -272.5401866390137116, -204.9646677080317545 ) ) ;
#89357 = CARTESIAN_POINT ( 'NONE',  ( -50.34922146392676723, -296.6402220358645536, -345.7101376294679085 ) ) ;
#89358 = CARTESIAN_POINT ( 'NONE',  ( 222.8344101925596306, 35.72494958537217968, 10.00000000000000000 ) ) ;
#89359 = CARTESIAN_POINT ( 'NONE',  ( 200.4551663812866025, 64.49084098423909950, 2.633798379907748455 ) ) ;
#89360 = CARTESIAN_POINT ( 'NONE',  ( -109.4997218494661837, -285.8027373141791827, -257.3503336445327818 ) ) ;
#89361 = CARTESIAN_POINT ( 'NONE',  ( -98.95351071658519970, -285.7136852403548346, -314.9232657090777820 ) ) ;
#89362 = CARTESIAN_POINT ( 'NONE',  ( -102.3252208087818644, -284.3552683475984963, -236.8792615856718555 ) ) ;
#89363 = CARTESIAN_POINT ( 'NONE',  ( -48.75141068166987424, -275.5995907636105926, -343.3257522533755264 ) ) ;
#89364 = CARTESIAN_POINT ( 'NONE',  ( 22.01152033341270808, -284.0284413453724142, -314.9698065617142220 ) ) ;
#89365 = CARTESIAN_POINT ( 'NONE',  ( -109.1663451174775474, -276.8158102312803521, -286.9073476630500750 ) ) ;
#89366 = ADVANCED_FACE ( 'NONE', ( #33020 ), #18346, .T. ) ;
#89367 = CARTESIAN_POINT ( 'NONE',  ( 13.95741670306516902, -277.3916214387619448, -322.8019233444435372 ) ) ;
#89368 = EDGE_CURVE ( 'NONE', #50728, #20922, #5380, .T. ) ;
#89369 = CARTESIAN_POINT ( 'NONE',  ( 207.8643778022844231, 35.72636131987244568, 15.02863188060211641 ) ) ;
#89370 = CARTESIAN_POINT ( 'NONE',  ( -45.26690633183829249, -280.7571534642659685, -193.8795140799045100 ) ) ;
#89371 = CARTESIAN_POINT ( 'NONE',  ( 8.504836755616295818, -281.1533043670194161, -208.5079879935735789 ) ) ;
#89372 = EDGE_LOOP ( 'NONE', ( #5455, #44062, #72870, #30662 ) ) ;
#89373 = ORIENTED_EDGE ( 'NONE', *, *, #85025, .F. ) ;
#89374 = DIRECTION ( 'NONE',  ( 0.000000000000000000, 0.000000000000000000, -1.000000000000000000 ) ) ;
#89375 = CARTESIAN_POINT ( 'NONE',  ( 38.11935580131428480, -289.4987117615590364, -277.1386187615212862 ) ) ;
#89376 = CARTESIAN_POINT ( 'NONE',  ( -109.9660671430326886, -295.6274957326057802, -279.6161511934201940 ) ) ;
#89377 = CARTESIAN_POINT ( 'NONE',  ( -111.5322591558799417, -290.1549628184417315, -250.0856013454351796 ) ) ;
#89378 = CARTESIAN_POINT ( 'NONE',  ( 5.327607962648773565, -284.8778091894870954, -209.8227397338502556 ) ) ;
#89380 = CARTESIAN_POINT ( 'NONE',  ( -108.7088430292875216, -288.5341825606834618, -290.1640951390168652 ) ) ;
#89379 = CARTESIAN_POINT ( 'NONE',  ( 28.19106208172495798, -285.6743395057474686, -236.7698823458048594 ) ) ;
#89381 = CARTESIAN_POINT ( 'NONE',  ( -62.71446410875797284, -286.9196287641611889, -201.4349049733087043 ) ) ;
#89382 = CARTESIAN_POINT ( 'NONE',  ( -109.5228071251508055, -276.2899097199914422, -290.7299285319364799 ) ) ;
#89383 = CARTESIAN_POINT ( 'NONE',  ( -48.76935568181369263, -287.5950964036263713, -345.7527351328146779 ) ) ;
#89384 = CARTESIAN_POINT ( 'NONE',  ( -32.46264471921647043, -288.1138060280721334, -195.5071587187340185 ) ) ;
#89385 = CARTESIAN_POINT ( 'NONE',  ( -31.98351722481240245, -286.9846679679006911, -345.3878743078071807 ) ) ;
#89386 = CIRCLE ( 'NONE', #7767, 16.36528803885689598 ) ;
#89387 = CARTESIAN_POINT ( 'NONE',  ( -24.01094357624661413, -283.8189348993204817, -342.3729182461612481 ) ) ;
#89388 = CARTESIAN_POINT ( 'NONE',  ( -103.5293050178018603, -292.0804366665715293, -305.9873636831243289 ) ) ;
#89389 = LINE ( 'NONE', #24543, #62481 ) ;
#89390 = CARTESIAN_POINT ( 'NONE',  ( 155.2899061951603983, 19.82375796246930477, -13.63853015639874577 ) ) ;
#89391 = CARTESIAN_POINT ( 'NONE',  ( -102.6183485460080647, -298.9780851594219939, -232.2017639280127526 ) ) ;
#89392 = CARTESIAN_POINT ( 'NONE',  ( -1.878874007633794418, -279.7319528412278373, -206.3690115102664038 ) ) ;
#89393 = CARTESIAN_POINT ( 'NONE',  ( 27.26939882073375543, -280.0623675382756801, -308.5478871368379714 ) ) ;
#89394 = CARTESIAN_POINT ( 'NONE',  ( -19.33506313426462242, -294.0234935300373991, -345.1147478915953002 ) ) ;
#89395 = CARTESIAN_POINT ( 'NONE',  ( 52.91742506675634417, -297.6002664758410674, -196.5862250154463027 ) ) ;
#89396 = CARTESIAN_POINT ( 'NONE',  ( 32.69620998941175571, -280.5322213171500607, -292.7963291489726316 ) ) ;
#89397 = CARTESIAN_POINT ( 'NONE',  ( -0.7839563394423398890, -274.6428808302404718, -335.2642193749258013 ) ) ;
#89398 = CARTESIAN_POINT ( 'NONE',  ( -80.43046367778833883, -296.9652166222387564, -329.8976776119802139 ) ) ;
#89399 = CARTESIAN_POINT ( 'NONE',  ( 180.7149167944524493, 8.542400036368780647, 10.00000000000000178 ) ) ;
#89400 = CARTESIAN_POINT ( 'NONE',  ( -108.6104089258873415, -271.4802977088584157, -242.6587614327106905 ) ) ;
#89401 = CARTESIAN_POINT ( 'NONE',  ( -22.32008223769805255, -293.1021836508136857, -344.8481974480610006 ) ) ;
#89402 = CARTESIAN_POINT ( 'NONE',  ( -25.33065611174975018, -293.6333903884172400, -197.7068171634307703 ) ) ;
#89403 = CARTESIAN_POINT ( 'NONE',  ( 194.7510731661265595, -164.3527196417747405, 21.50000000000000000 ) ) ;
#89404 = CARTESIAN_POINT ( 'NONE',  ( 33.80239623952288497, -294.1297444140612924, -253.2454116158244233 ) ) ;
#89405 = CARTESIAN_POINT ( 'NONE',  ( 193.9646936176702070, 21.00000000000000000, 15.00000000000000000 ) ) ;
#89407 = CARTESIAN_POINT ( 'NONE',  ( -68.51733844332717638, -295.4735227503932151, -336.3830273528693624 ) ) ;
#89406 = CARTESIAN_POINT ( 'NONE',  ( -60.74530722553166129, -281.3742846077544755, -342.0443710660948682 ) ) ;
#89408 = CARTESIAN_POINT ( 'NONE',  ( 25.93032726673651567, -282.1321097808176432, -314.2665421819561402 ) ) ;
#89409 = CARTESIAN_POINT ( 'NONE',  ( 31.84442904996111068, -283.0775418811463737, -239.9868900143509620 ) ) ;
#89410 = CARTESIAN_POINT ( 'NONE',  ( -43.66029834974155932, -285.6412345998592173, -193.5887780097785935 ) ) ;
#89411 = CARTESIAN_POINT ( 'NONE',  ( -94.83234444130621910, -289.2152406181785409, -222.4364852949967428 ) ) ;
#89412 = CARTESIAN_POINT ( 'NONE',  ( -13.65569264099284652, -281.2300240906441786, -342.8985621121468625 ) ) ;
#89413 = CARTESIAN_POINT ( 'NONE',  ( 28.10487465666762930, -285.7844200708175322, -236.8125148771269437 ) ) ;
#89414 = CARTESIAN_POINT ( 'NONE',  ( 35.64932073798920698, -286.7696222920217224, -293.8941454666069149 ) ) ;
#89415 = CARTESIAN_POINT ( 'NONE',  ( 17.06571399127465583, -89.54582641780471874, -22.50000000000000000 ) ) ;
#89416 = CARTESIAN_POINT ( 'NONE',  ( -67.60483385280748792, -297.0560810212458591, -337.6845789042358206 ) ) ;
#89417 = CARTESIAN_POINT ( 'NONE',  ( 23.06348465569197614, -277.6072768240239270, -317.1778564322460738 ) ) ;
#89419 = CARTESIAN_POINT ( 'NONE',  ( -85.49494253552357748, -279.0308847195248632, -215.4671043532024157 ) ) ;
#89418 = CARTESIAN_POINT ( 'NONE',  ( -67.58959721577458879, -293.4671412832298643, -339.3790252758977317 ) ) ;
#89420 = CARTESIAN_POINT ( 'NONE',  ( 38.85158054002001649, -293.5753268677494816, -258.8865971006352424 ) ) ;
#89421 = CARTESIAN_POINT ( 'NONE',  ( -64.01553590476950717, -283.7868149177917871, -199.6519509270303274 ) ) ;
#89422 = CARTESIAN_POINT ( 'NONE',  ( -12.50385522402253713, -278.7294596734267884, -341.1834041075422306 ) ) ;
#89423 = CARTESIAN_POINT ( 'NONE',  ( -78.09058255606841215, -294.6732798875499384, -331.2741399715538932 ) ) ;
#89424 = CARTESIAN_POINT ( 'NONE',  ( -111.7261818921962657, -270.6950922534273900, -259.1913258926078356 ) ) ;
#89425 = ORIENTED_EDGE ( 'NONE', *, *, #41918, .F. ) ;
#89426 = CARTESIAN_POINT ( 'NONE',  ( 205.4738562182569694, 293.9636489450776367, -54.00000000000000000 ) ) ;
#89427 = CARTESIAN_POINT ( 'NONE',  ( 29.63786612094960304, -283.9700359865263977, -303.4267081921054228 ) ) ;
#89428 = CARTESIAN_POINT ( 'NONE',  ( 8.261691419512516177, -293.9166311337340289, -327.5078217727971150 ) ) ;
#89429 = DIRECTION ( 'NONE',  ( 0.000000000000000000, 0.000000000000000000, -1.000000000000000000 ) ) ;
#89430 = CARTESIAN_POINT ( 'NONE',  ( -110.4542110544635705, -270.2666405000204009, -253.6410175316879361 ) ) ;
#89431 = CARTESIAN_POINT ( 'NONE',  ( -102.5765401351289086, -272.2816307452516185, -229.7584768185925554 ) ) ;
#89432 = CARTESIAN_POINT ( 'NONE',  ( 7.658067293608112891, -289.7677158402987629, -332.2998705699396282 ) ) ;
#89433 = CARTESIAN_POINT ( 'NONE',  ( -18.47555092028106571, -288.6357094860068742, -340.9336893357166787 ) ) ;
#89434 = CARTESIAN_POINT ( 'NONE',  ( -72.47715935342125704, -281.0982339343012200, -205.5829792430650969 ) ) ;
#89435 = CARTESIAN_POINT ( 'NONE',  ( -111.1417001269576588, -274.1520230526816704, -270.3814443024369325 ) ) ;
#89436 = CARTESIAN_POINT ( 'NONE',  ( -49.19098065889696159, -278.6926907910788600, -197.9268370460091546 ) ) ;
#89437 = ORIENTED_EDGE ( 'NONE', *, *, #21756, .F. ) ;
#89438 = CARTESIAN_POINT ( 'NONE',  ( -78.18764879069254903, -297.1854389532834375, -205.1127251338899100 ) ) ;
#89439 = CARTESIAN_POINT ( 'NONE',  ( -25.19779744363221141, -294.1281924848746030, -196.8658608858496564 ) ) ;
#89440 = CARTESIAN_POINT ( 'NONE',  ( 30.18048445740676300, -294.6905496191523071, -234.9319349767842198 ) ) ;
#89441 = PLANE ( 'NONE',  #50658 ) ;
#89442 = CARTESIAN_POINT ( 'NONE',  ( -98.38922950490488972, -291.7615813757562364, -230.0560744510994198 ) ) ;
#89443 = CARTESIAN_POINT ( 'NONE',  ( 209.6287663260175975, 29.00782453271232697, 12.00000000000000000 ) ) ;
#89444 = CARTESIAN_POINT ( 'NONE',  ( -53.10876038268776966, -289.9918161514729604, -196.2014567411923451 ) ) ;
#89446 = CARTESIAN_POINT ( 'NONE',  ( -44.56695475053873423, -297.6250690021802825, -197.6479168033173437 ) ) ;
#89445 = CIRCLE ( 'NONE', #30539, 25.00000000000001066 ) ;
#89447 = CARTESIAN_POINT ( 'NONE',  ( 132.9888089158688445, -299.5541904835127980, -202.0104999926936387 ) ) ;
#89448 = AXIS2_PLACEMENT_3D ( 'NONE', #58364, #87662, #37028 ) ;
#89449 = CARTESIAN_POINT ( 'NONE',  ( 195.7060440449982650, 26.13302583088762532, 14.67646719788673160 ) ) ;
#89450 = CARTESIAN_POINT ( 'NONE',  ( -100.0992595278448505, -291.4937834876097895, -313.7684502109029268 ) ) ;
#89451 = CARTESIAN_POINT ( 'NONE',  ( -55.63300648810263738, -294.3376638359845288, -190.3683826091709363 ) ) ;
#89452 = CARTESIAN_POINT ( 'NONE',  ( -8.817577174657690975, -288.4263100684626124, -201.1634395857448396 ) ) ;
#89453 = CARTESIAN_POINT ( 'NONE',  ( -8.234802571833906626, -272.4338772165622231, -201.3651656009776616 ) ) ;
#89454 = CARTESIAN_POINT ( 'NONE',  ( 18.34686840596227952, -276.7793647409547475, -220.8874262223460505 ) ) ;
#89455 = CARTESIAN_POINT ( 'NONE',  ( -6.654716109768185284, -290.5380812150057181, -202.5405959210113451 ) ) ;
#89456 = CARTESIAN_POINT ( 'NONE',  ( -74.42438996437691401, -281.4247891971587592, -204.2916121887988083 ) ) ;
#89457 = ORIENTED_EDGE ( 'NONE', *, *, #66023, .F. ) ;
#89458 = CARTESIAN_POINT ( 'NONE',  ( 20.25616722230283884, -281.5343718934914250, -315.3764303245428096 ) ) ;
#89459 = CARTESIAN_POINT ( 'NONE',  ( -112.1034855576187113, -279.8464499182607028, -253.2681969077653150 ) ) ;
#89460 = CARTESIAN_POINT ( 'NONE',  ( -6.376732243084020979, -279.2448364066792692, -200.2813807390731426 ) ) ;
#89461 = CARTESIAN_POINT ( 'NONE',  ( -95.25716805911793017, -238.2204399489505136, -338.9131918094142293 ) ) ;
#89462 = CARTESIAN_POINT ( 'NONE',  ( 35.50286416067508100, -276.1857100173000390, -245.9760889050689627 ) ) ;
#89463 = APPLICATION_PROTOCOL_DEFINITION ( 'draft international standard', 'automotive_design', 1998, #51103 ) ;
#89464 = CARTESIAN_POINT ( 'NONE',  ( 19.50628162436637325, -276.3748997461619865, -219.3814804009799673 ) ) ;
#89465 = CARTESIAN_POINT ( 'NONE',  ( -85.33152481854864391, -299.9090924074131408, -210.2361428286349110 ) ) ;
#89466 = ORIENTED_EDGE ( 'NONE', *, *, #25669, .T. ) ;
#89467 = EDGE_LOOP ( 'NONE', ( #2307, #42924, #6796, #76758 ) ) ;
#89468 = CARTESIAN_POINT ( 'NONE',  ( -98.36037189802839009, -291.0698786233921851, -311.0158215604650991 ) ) ;
#89469 = CARTESIAN_POINT ( 'NONE',  ( -84.51777558273262514, -291.4513693691804406, -329.9966162680774460 ) ) ;
#89470 = CARTESIAN_POINT ( 'NONE',  ( 6.744307514924360980, -292.0187043061973213, -212.0488842923588493 ) ) ;
#89471 = CARTESIAN_POINT ( 'NONE',  ( 20.24486260099647339, -286.3674025849967393, -219.2597765706826181 ) ) ;
#89472 = CARTESIAN_POINT ( 'NONE',  ( 199.2172143179937223, 26.36928053068234590, 9.271110512036644380 ) ) ;
#89473 = CARTESIAN_POINT ( 'NONE',  ( -32.10909449115905545, -281.3849132347797877, -343.9753846289269745 ) ) ;
#89474 = CARTESIAN_POINT ( 'NONE',  ( 36.18706099546115951, -289.5463120928164926, -280.6708646512282712 ) ) ;
#89475 = CARTESIAN_POINT ( 'NONE',  ( 19.01216452693342163, -280.7004775883492584, -317.8670106553200299 ) ) ;
#89476 = EDGE_CURVE ( 'NONE', #5341, #68064, #31054, .T. ) ;
#89477 = CARTESIAN_POINT ( 'NONE',  ( -14.16916049563535651, -281.6741265309902360, -200.5629539912193309 ) ) ;
#89478 = CARTESIAN_POINT ( 'NONE',  ( 22.23015896804160718, -289.1451100435464809, -318.7968261610265586 ) ) ;
#89479 = CARTESIAN_POINT ( 'NONE',  ( -87.57748483340623125, -279.8205072657860910, -217.2407063370519893 ) ) ;
#89480 = CARTESIAN_POINT ( 'NONE',  ( 6.282760694807794977, -291.4251603220413926, -207.3935458872689708 ) ) ;
#89481 = CARTESIAN_POINT ( 'NONE',  ( 24.56709055569362121, -287.7491371279205623, -224.8478182016912399 ) ) ;
#89482 = CARTESIAN_POINT ( 'NONE',  ( 9.768125325348606225, -287.1736571232110578, -209.5319206444170561 ) ) ;
#89483 = CARTESIAN_POINT ( 'NONE',  ( -38.88295117023228897, -283.2386657512871579, -343.3573368668735384 ) ) ;
#89484 = ORIENTED_EDGE ( 'NONE', *, *, #79409, .T. ) ;
#89485 = CYLINDRICAL_SURFACE ( 'NONE', #6564, 1.000000000000000888 ) ;
#89486 = CARTESIAN_POINT ( 'NONE',  ( -33.62405605891816407, -293.9588901553893834, -194.6875783233080597 ) ) ;
#89487 = CARTESIAN_POINT ( 'NONE',  ( 35.82032427846419154, -291.9542323640077370, -247.9866580422593927 ) ) ;
#89488 = CARTESIAN_POINT ( 'NONE',  ( 22.65171675344419810, -275.1958268891521016, -312.4505239295602905 ) ) ;
#89489 = CARTESIAN_POINT ( 'NONE',  ( -106.4181144413962414, -296.3352296150459892, -236.5711524323585309 ) ) ;
#89490 = CARTESIAN_POINT ( 'NONE',  ( 0.2794937784735365693, -291.0429634010310451, -206.9943007867879032 ) ) ;
#89491 = CARTESIAN_POINT ( 'NONE',  ( -110.3663237032401696, -294.6351290922206658, -282.4184131245139611 ) ) ;
#89492 = CARTESIAN_POINT ( 'NONE',  ( -17.33904456994252996, -293.5210522161517588, -199.6893769056655401 ) ) ;
#89493 = CARTESIAN_POINT ( 'NONE',  ( -9.623295292990453831, -293.5025586904683905, -202.4402105184946947 ) ) ;
#89494 = CARTESIAN_POINT ( 'NONE',  ( 209.3679137592659742, 36.51444217272602089, 14.69807323122302023 ) ) ;
#89495 = CARTESIAN_POINT ( 'NONE',  ( -50.18006202488202661, -293.2153406335911541, -344.4759498966058118 ) ) ;
#89496 = CARTESIAN_POINT ( 'NONE',  ( -40.56572100135387160, -300.0117644542553421, -195.4272741709044112 ) ) ;
#89497 = CARTESIAN_POINT ( 'NONE',  ( 23.71225731600947739, -289.0530819438629919, -310.8293345781241328 ) ) ;
#89498 = CARTESIAN_POINT ( 'NONE',  ( 27.68949517821442186, -278.0383698159658934, -308.4314533864418308 ) ) ;
#89499 = CARTESIAN_POINT ( 'NONE',  ( -99.33748818300107075, -276.7467863792031153, -315.3782167805674135 ) ) ;
#89500 = CARTESIAN_POINT ( 'NONE',  ( -85.73764015344455913, -272.7506409636969806, -210.6020536045909353 ) ) ;
#89501 = CARTESIAN_POINT ( 'NONE',  ( 35.98978329911530949, -279.4664256948481693, -257.5623782858217510 ) ) ;
#89502 = CARTESIAN_POINT ( 'NONE',  ( -88.68823285611243534, -276.1585796520872691, -326.6636400448284689 ) ) ;
#89503 = CARTESIAN_POINT ( 'NONE',  ( -109.2582484549825921, -295.4361481255918989, -255.1595544451657531 ) ) ;
#89504 = CARTESIAN_POINT ( 'NONE',  ( 207.4724402404594343, 29.73442829110639352, 14.90057469441957672 ) ) ;
#89505 = CARTESIAN_POINT ( 'NONE',  ( -69.54332678119122590, -274.2680799018471589, -204.7337768093673276 ) ) ;
#89506 = CARTESIAN_POINT ( 'NONE',  ( 154.7659666677267580, 20.47222690886501795, 12.53936336329526036 ) ) ;
#89507 = AXIS2_PLACEMENT_3D ( 'NONE', #31981, #67043, #3569 ) ;
#89509 = CARTESIAN_POINT ( 'NONE',  ( -64.56681560066327563, -273.5199108060260755, -202.6143888029167499 ) ) ;
#89508 = CARTESIAN_POINT ( 'NONE',  ( -96.02541180810462151, -287.9245676861992251, -317.6533354294903120 ) ) ;
#89510 = AXIS2_PLACEMENT_3D ( 'NONE', #18288, #25387, #40044 ) ;
#89511 = CARTESIAN_POINT ( 'NONE',  ( 7.934511617521064153, -288.4527535073499394, -332.7090066298840725 ) ) ;
#89512 = CARTESIAN_POINT ( 'NONE',  ( -109.2899178662530915, -274.8341690076491659, -248.4233425930360681 ) ) ;
#89513 = CARTESIAN_POINT ( 'NONE',  ( -95.38019244579690792, -293.8995456241070201, -317.6206749504253253 ) ) ;
#89514 = VECTOR ( 'NONE', #26310, 1000.000000000000000 ) ;
#89515 = CARTESIAN_POINT ( 'NONE',  ( -35.91247187751956460, -282.2318601589695390, -347.1994386176735929 ) ) ;
#89516 = CARTESIAN_POINT ( 'NONE',  ( 160.5350683151633291, 275.5000000000000568, 24.72542485937379197 ) ) ;
#89517 = AXIS2_PLACEMENT_3D ( 'NONE', #6778, #64570, #50784 ) ;
#89518 = CARTESIAN_POINT ( 'NONE',  ( -12.13826047484608139, -280.7241860383239782, -341.0534281199036286 ) ) ;
#89519 = DIRECTION ( 'NONE',  ( 0.000000000000000000, 0.000000000000000000, 1.000000000000000000 ) ) ;
#89520 = CARTESIAN_POINT ( 'NONE',  ( -102.7565311824030942, -289.7980703111861658, -236.9615677730293442 ) ) ;
#89521 = CARTESIAN_POINT ( 'NONE',  ( -76.80346382140157857, -281.7257616959386155, -333.2998574769731590 ) ) ;
#89522 = DIRECTION ( 'NONE',  ( -0.000000000000000000, -0.000000000000000000, 1.000000000000000000 ) ) ;
#89523 = CARTESIAN_POINT ( 'NONE',  ( 209.9972545312790544, 27.55378999303205845, 9.000000000000001776 ) ) ;
#89524 = CARTESIAN_POINT ( 'NONE',  ( -106.5387474176101250, -288.9312600503197928, -241.2991152413904388 ) ) ;
#89525 = CARTESIAN_POINT ( 'NONE',  ( -16.46258788178147370, -275.8469055298156150, -199.6342240971159185 ) ) ;
#89526 = CARTESIAN_POINT ( 'NONE',  ( -85.83907311387635275, -284.9119800860808596, -329.6571004007793135 ) ) ;
#89528 = CARTESIAN_POINT ( 'NONE',  ( -103.0126648816664812, -284.1191776638242459, -302.3570525356987559 ) ) ;
#89527 = CARTESIAN_POINT ( 'NONE',  ( -65.66433593259694135, -271.7645022383798050, -200.2962157397798819 ) ) ;
#89529 = CARTESIAN_POINT ( 'NONE',  ( 36.17457843463265732, -276.9214979134900432, -266.0867995092721117 ) ) ;
#89530 = CARTESIAN_POINT ( 'NONE',  ( -1.381964546635444435, -277.3654279028797305, -334.1326485075859409 ) ) ;
#89531 = CARTESIAN_POINT ( 'NONE',  ( 31.73412386079864334, -283.9355731619110088, -299.7091107255139946 ) ) ;
#89532 = ORIENTED_EDGE ( 'NONE', *, *, #28676, .F. ) ;
#89533 = DIRECTION ( 'NONE',  ( 0.000000000000000000, 0.000000000000000000, -1.000000000000000000 ) ) ;
#89534 = CARTESIAN_POINT ( 'NONE',  ( 37.78345704703205143, -293.5974273715423806, -287.3088078472175084 ) ) ;
#89535 = CARTESIAN_POINT ( 'NONE',  ( 33.83452654890530908, -289.2399818291281690, -247.8285627679293555 ) ) ;
#89536 = DIRECTION ( 'NONE',  ( 0.000000000000000000, 0.000000000000000000, 1.000000000000000000 ) ) ;
#89537 = CARTESIAN_POINT ( 'NONE',  ( -111.2586520408596868, -294.4809262143061801, -234.7283546768995564 ) ) ;
#89538 = CARTESIAN_POINT ( 'NONE',  ( -111.2879077670209540, -277.4870441926948388, -291.2445371603733975 ) ) ;
#89539 = CARTESIAN_POINT ( 'NONE',  ( -3.656448422669502207, -290.8890959978990054, -201.9965700247914242 ) ) ;
#89540 = EDGE_CURVE ( 'NONE', #23241, #60845, #53393, .T. ) ;
#89541 = CARTESIAN_POINT ( 'NONE',  ( -108.0254573401965388, -286.3475910243426483, -249.3389682291132772 ) ) ;
#89542 = CARTESIAN_POINT ( 'NONE',  ( -0.9527373633970337430, -278.3225820091101923, -334.8692371559108096 ) ) ;
#89543 = CARTESIAN_POINT ( 'NONE',  ( -3.764777859138308980, -287.9117285792387975, -201.7085463397041281 ) ) ;
#89544 = CARTESIAN_POINT ( 'NONE',  ( 36.19661376582089929, -283.7423361385128260, -285.1607479984036218 ) ) ;
#89545 = CARTESIAN_POINT ( 'NONE',  ( 36.88618722070909683, -275.9758810718828954, -290.8851671381925712 ) ) ;
#89546 = CARTESIAN_POINT ( 'NONE',  ( -41.38656795465438165, -276.9350503042121545, -347.2680134802552629 ) ) ;
#89547 = CARTESIAN_POINT ( 'NONE',  ( -37.17037521643547393, -299.9744739958862851, -195.9181485666683216 ) ) ;
#89548 = DIRECTION ( 'NONE',  ( -1.000000000000000000, 0.000000000000000000, 0.000000000000000000 ) ) ;
#89549 = CARTESIAN_POINT ( 'NONE',  ( -35.48537860860557203, -296.2147462987906010, -194.5968914209361458 ) ) ;
#89550 = CARTESIAN_POINT ( 'NONE',  ( 175.2296996224750103, 249.5000000000000568, 0.000000000000000000 ) ) ;
#89551 = CARTESIAN_POINT ( 'NONE',  ( -104.3303182376368881, -277.6664958076602829, -299.6514788180591040 ) ) ;
#89552 = CARTESIAN_POINT ( 'NONE',  ( -91.89709851682771102, -274.4996536539099452, -216.5864285385212611 ) ) ;
#89553 = CARTESIAN_POINT ( 'NONE',  ( 38.95033447754254041, -280.4983550037198370, -261.3894040300933739 ) ) ;
#89554 = CARTESIAN_POINT ( 'NONE',  ( 30.88732767148243497, -288.9310968579018208, -241.5444558237892352 ) ) ;
#89555 = CARTESIAN_POINT ( 'NONE',  ( -90.21755856913489424, -297.3033715790449492, -325.4506740825601128 ) ) ;
#89556 = CARTESIAN_POINT ( 'NONE',  ( -58.72568541237021122, -296.5276727506683869, -343.9740910476299973 ) ) ;
#89557 = CARTESIAN_POINT ( 'NONE',  ( -22.39883148805939328, -294.2441040339019764, -197.0348668834258206 ) ) ;
#89558 = CARTESIAN_POINT ( 'NONE',  ( 33.07118982870879620, -279.8829693740426023, -295.8529559536213469 ) ) ;
#89559 = CARTESIAN_POINT ( 'NONE',  ( 18.11967539104738023, -282.7756263267584700, -220.7088267491818669 ) ) ;
#89560 = CARTESIAN_POINT ( 'NONE',  ( -110.1333905936174489, -270.7855059343972925, -253.8318528300186472 ) ) ;
#89561 = CARTESIAN_POINT ( 'NONE',  ( -96.53789120484952946, -285.5017296358883527, -318.3633984162175921 ) ) ;
#89562 = CARTESIAN_POINT ( 'NONE',  ( 34.30988347380085202, -286.6768228988213991, -285.9207998429771465 ) ) ;
#89563 = CARTESIAN_POINT ( 'NONE',  ( 20.05813539071349538, -280.2058893438782547, -219.1693347566229022 ) ) ;
#89564 = CARTESIAN_POINT ( 'NONE',  ( -38.02263352848247990, -140.5509088181942445, -364.3887990180761562 ) ) ;
#89565 = ORIENTED_EDGE ( 'NONE', *, *, #51587, .F. ) ;
#89566 = CARTESIAN_POINT ( 'NONE',  ( 22.01124561654895828, -286.6234958640722539, -227.7398159755128404 ) ) ;
#89567 = VERTEX_POINT ( 'NONE', #47201 ) ;
#89568 = CARTESIAN_POINT ( 'NONE',  ( -104.1409881482590691, -285.1397499082257241, -308.1428741419522339 ) ) ;
#89569 = CARTESIAN_POINT ( 'NONE',  ( 19.86942043269093006, -275.2449088329015581, -224.9651806263860294 ) ) ;
#89570 = CARTESIAN_POINT ( 'NONE',  ( -47.68802408213801414, -290.8440142346942707, -194.3177641256785080 ) ) ;
#89571 = CARTESIAN_POINT ( 'NONE',  ( 39.30944045300030609, -282.1264530914276634, -264.2035670107734973 ) ) ;
#89572 = EDGE_CURVE ( 'NONE', #68312, #86758, #19419, .T. ) ;
#89573 = CARTESIAN_POINT ( 'NONE',  ( -113.5198228996071492, -280.1281459132346185, -265.9337754227978508 ) ) ;
#89574 = CARTESIAN_POINT ( 'NONE',  ( 19.14176147960793273, -281.1727975640687873, -218.0604214638796350 ) ) ;
#89575 = CARTESIAN_POINT ( 'NONE',  ( -102.0455923789670294, -281.6237833571633473, -301.4846348637937581 ) ) ;
#89576 = CARTESIAN_POINT ( 'NONE',  ( -113.3214668634831810, -274.1400524880032208, -284.1914339370617881 ) ) ;
#89577 = ORIENTED_EDGE ( 'NONE', *, *, #68389, .F. ) ;
#89578 = CIRCLE ( 'NONE', #74529, 9.550761578869391144 ) ;
#89579 = CARTESIAN_POINT ( 'NONE',  ( 26.96367716403861436, -278.0655883586620689, -308.6344360511462810 ) ) ;
#89580 = CARTESIAN_POINT ( 'NONE',  ( 193.0921611339578305, 279.2154153515940607, -125.6430880757993549 ) ) ;
#89581 = CARTESIAN_POINT ( 'NONE',  ( 35.05693201289778216, -279.3370976900665710, -252.1353739874853090 ) ) ;
#89582 = CARTESIAN_POINT ( 'NONE',  ( -36.47356891843505622, -297.4118876466293386, -197.2592832589931788 ) ) ;
#89583 = CARTESIAN_POINT ( 'NONE',  ( 32.17172918639448653, -293.4841391175193053, -303.4611917219432939 ) ) ;
#89584 = LINE ( 'NONE', #17655, #5231 ) ;
#89586 = CARTESIAN_POINT ( 'NONE',  ( 21.80253129913998222, -286.5649270830892306, -314.5229525738844814 ) ) ;
#89585 = CARTESIAN_POINT ( 'NONE',  ( -62.63277583733828635, -296.3040568366923253, -198.2572499750793042 ) ) ;
#89587 = CARTESIAN_POINT ( 'NONE',  ( 4.532336546358201268, -296.3408069062683126, -331.6590015584054072 ) ) ;
#89588 = CARTESIAN_POINT ( 'NONE',  ( -42.72686556746183584, -287.2979985812592645, -197.0528173508388363 ) ) ;
#89589 = CARTESIAN_POINT ( 'NONE',  ( 39.47615555355140060, -294.4926128789574591, -270.2981507593422634 ) ) ;
#89590 = VECTOR ( 'NONE', #12677, 1000.000000000000000 ) ;
#89591 = CARTESIAN_POINT ( 'NONE',  ( -102.2959638390236705, -285.4988446825265100, -236.9106760238458378 ) ) ;
#89592 = CARTESIAN_POINT ( 'NONE',  ( -68.00434641705011529, -296.4535213656557744, -200.1062516053708009 ) ) ;
#89593 = CARTESIAN_POINT ( 'NONE',  ( 22.97494117368558619, -293.7167107255746146, -222.7369285509479653 ) ) ;
#89594 = CARTESIAN_POINT ( 'NONE',  ( -97.41944825924889528, -291.6888234764058438, -222.2966707987500570 ) ) ;
#89595 = CARTESIAN_POINT ( 'NONE',  ( -80.40579356196042227, -289.8205086444457947, -329.3687714034125520 ) ) ;
#89596 = EDGE_LOOP ( 'NONE', ( #30440, #69231, #7757, #43157, #8678, #60952 ) ) ;
#89597 = CARTESIAN_POINT ( 'NONE',  ( 156.8097460173007391, 17.78059845260462879, 7.900495735314976287 ) ) ;
#89598 = CARTESIAN_POINT ( 'NONE',  ( 29.40725091552484116, -300.7397427917375126, -194.5754132039499211 ) ) ;
#89599 = CARTESIAN_POINT ( 'NONE',  ( -105.2497983556404222, -271.8080301367127163, -234.7993882073907912 ) ) ;
#89600 = EDGE_CURVE ( 'NONE', #19714, #70200, #18949, .T. ) ;
#89601 = CARTESIAN_POINT ( 'NONE',  ( 32.45191108217840537, -280.9060830272578642, -292.7131321126132661 ) ) ;
#89602 = ORIENTED_EDGE ( 'NONE', *, *, #87556, .T. ) ;
#89603 = CARTESIAN_POINT ( 'NONE',  ( -22.95656013185844557, -276.3806422459417718, -345.9969674020971411 ) ) ;
#89604 = CARTESIAN_POINT ( 'NONE',  ( -95.22765546882318688, -271.5910568669068539, -224.5827760291528534 ) ) ;
#89605 = CARTESIAN_POINT ( 'NONE',  ( -104.4971973853501197, -280.8343585884473441, -238.6015539059482364 ) ) ;
#89606 = CARTESIAN_POINT ( 'NONE',  ( 19.23467353355029630, -274.3638054465916412, -318.4233633109172388 ) ) ;
#89607 = CARTESIAN_POINT ( 'NONE',  ( -100.2449718660991493, -298.2759484656190807, -232.4428217309732077 ) ) ;
#89608 = CARTESIAN_POINT ( 'NONE',  ( -34.47848897105268406, -299.1684960680592553, -197.0514629679084919 ) ) ;
#89609 = CARTESIAN_POINT ( 'NONE',  ( -101.6522597959774288, -298.6936015266034019, -229.4882378558616836 ) ) ;
#89610 = CARTESIAN_POINT ( 'NONE',  ( -73.14075153709077881, -271.6005217377178838, -203.9944877908874616 ) ) ;
#89611 = CARTESIAN_POINT ( 'NONE',  ( 14.94261957995175294, -293.4646942536728034, -219.1980916455273416 ) ) ;
#89612 = CARTESIAN_POINT ( 'NONE',  ( 4.856258706341020748, -291.2090557548905281, -210.0101089810492567 ) ) ;
#89613 = DIRECTION ( 'NONE',  ( -0.000000000000000000, -1.000000000000000000, -0.000000000000000000 ) ) ;
#89614 = CARTESIAN_POINT ( 'NONE',  ( 39.07722661911996198, -276.1618146138142720, -279.7341719111043403 ) ) ;
#89615 = CARTESIAN_POINT ( 'NONE',  ( -90.19806985006050581, -273.4451126151090534, -219.9920179780639273 ) ) ;
#89616 = VECTOR ( 'NONE', #41113, 1000.000000000000000 ) ;
#89617 = CARTESIAN_POINT ( 'NONE',  ( 25.51554251903686321, -280.8171480738862442, -313.9991184223015921 ) ) ;
#89618 = AXIS2_PLACEMENT_3D ( 'NONE', #41694, #82910, #4322 ) ;
#89619 = CARTESIAN_POINT ( 'NONE',  ( 199.0061125298537377, 275.5000000000000568, -7.725424859374024678 ) ) ;
#89620 = CARTESIAN_POINT ( 'NONE',  ( -97.67128999651612276, -283.1734218353493020, -311.8371371473529621 ) ) ;
#89621 = CARTESIAN_POINT ( 'NONE',  ( -112.0836631749813250, -282.4497652703412882, -278.3403024742773937 ) ) ;
#89622 = CARTESIAN_POINT ( 'NONE',  ( 25.87252631797964852, -274.6407073834440666, -308.0352004666191306 ) ) ;
#89623 = CARTESIAN_POINT ( 'NONE',  ( -0.5222142068229049805, -282.5415884900606898, -205.0065253237449099 ) ) ;
#89624 = DIRECTION ( 'NONE',  ( -0.9693563597868445347, -0.2456588035076248955, 4.725301599749410243E-16 ) ) ;
#89625 = CARTESIAN_POINT ( 'NONE',  ( -39.80257052418234309, -229.5268262511776527, 22.50000000000000000 ) ) ;
#89626 = CARTESIAN_POINT ( 'NONE',  ( -7.979802776668437403, -272.8301804169730076, -199.9892464306108479 ) ) ;
#89627 = CARTESIAN_POINT ( 'NONE',  ( -104.6911229971985904, -280.1114965826322418, -303.8560367657680672 ) ) ;
#89628 = DIRECTION ( 'NONE',  ( 0.000000000000000000, 1.000000000000000000, 0.000000000000000000 ) ) ;
#89629 = CARTESIAN_POINT ( 'NONE',  ( -112.3922429004825148, -286.5839443893443672, -261.6015388478689943 ) ) ;
#89630 = CARTESIAN_POINT ( 'NONE',  ( 159.4851178187817879, 15.24064981607345892, -10.00000000000000178 ) ) ;
#89631 = CARTESIAN_POINT ( 'NONE',  ( -49.08822542786022325, -287.2015263728127366, -344.4875244724072445 ) ) ;
#89632 = DIRECTION ( 'NONE',  ( -0.000000000000000000, -0.000000000000000000, -1.000000000000000000 ) ) ;
#89633 = CARTESIAN_POINT ( 'NONE',  ( -101.5545765529196274, -295.8303392183124174, -234.8106326821514358 ) ) ;
#89634 = CARTESIAN_POINT ( 'NONE',  ( -93.35914168139744618, -288.0081132860211710, -319.1505097427698843 ) ) ;
#89635 = CARTESIAN_POINT ( 'NONE',  ( -110.2140734402150315, -271.0703965937372004, -283.6296548450457635 ) ) ;
#89636 = CARTESIAN_POINT ( 'NONE',  ( -110.7310329344303312, -294.7512726589940826, -254.8396355759154233 ) ) ;
#89637 = CARTESIAN_POINT ( 'NONE',  ( 24.99003905089042377, -285.4440322402592756, -226.3219713853931410 ) ) ;
#89638 = CARTESIAN_POINT ( 'NONE',  ( 34.43292557344552307, -283.3770420041131501, -287.5859502710481479 ) ) ;
#89639 = CARTESIAN_POINT ( 'NONE',  ( -94.58630382248043134, -282.1072233756623291, -320.3314027839390974 ) ) ;
#89640 = CARTESIAN_POINT ( 'NONE',  ( -56.06559070839884384, -289.2999729422390942, -340.9715655669982652 ) ) ;
#89641 = AXIS2_PLACEMENT_3D ( 'NONE', #67192, #44459, #45848 ) ;
#89642 = CARTESIAN_POINT ( 'NONE',  ( 26.96501145241477460, -282.4921625928938056, -234.5837262181236724 ) ) ;
#89643 = CARTESIAN_POINT ( 'NONE',  ( -21.34296844787180092, -283.6446520213218037, -341.8040192261576635 ) ) ;
#89644 = CARTESIAN_POINT ( 'NONE',  ( 34.27771780962692816, -289.2288727925524086, -246.7622623630037424 ) ) ;
#89645 = AXIS2_PLACEMENT_3D ( 'NONE', #81148, #36668, #51791 ) ;
#89646 = CARTESIAN_POINT ( 'NONE',  ( -70.73096209601445139, -297.7905275210860054, -200.9769901882598333 ) ) ;
#89647 = AXIS2_PLACEMENT_3D ( 'NONE', #92300, #57293, #43523 ) ;
#89648 = CARTESIAN_POINT ( 'NONE',  ( -52.54562162856652208, -273.8627062079351617, -194.8226338173148235 ) ) ;
#89649 = CARTESIAN_POINT ( 'NONE',  ( -69.75411472329601281, -293.6032317298727321, -203.1065217269365917 ) ) ;
#89650 = DIRECTION ( 'NONE',  ( 0.000000000000000000, 1.000000000000000000, -0.000000000000000000 ) ) ;
#89651 = CARTESIAN_POINT ( 'NONE',  ( -95.99890600148557951, -281.6948066931273615, -223.6242672951989618 ) ) ;
#89652 = VECTOR ( 'NONE', #29483, 1000.000000000000000 ) ;
#89653 = CARTESIAN_POINT ( 'NONE',  ( -6.071259384224857669, -274.6419973810752140, -338.7145229160199165 ) ) ;
#89654 = CARTESIAN_POINT ( 'NONE',  ( 198.0449670149796475, 67.45552974974890503, 11.11895152694587274 ) ) ;
#89655 = CARTESIAN_POINT ( 'NONE',  ( -108.1376984480758807, -295.3149284291123990, -242.0349015764902560 ) ) ;
#89656 = CARTESIAN_POINT ( 'NONE',  ( -104.7704509811376994, -291.7513341656749617, -300.4839769747057971 ) ) ;
#89657 = CARTESIAN_POINT ( 'NONE',  ( -0.4877240763478836172, -273.9045122362478537, -207.2142865447675320 ) ) ;
#89658 = CIRCLE ( 'NONE', #56458, 24.50000000000000000 ) ;
#89659 = CARTESIAN_POINT ( 'NONE',  ( -93.09359937935977314, -292.7524649219082562, -222.1694850611783920 ) ) ;
#89660 = CARTESIAN_POINT ( 'NONE',  ( -65.42824781417573377, -292.6170040373164056, -202.7121077450888720 ) ) ;
#89661 = CARTESIAN_POINT ( 'NONE',  ( -10.58885741231271815, -284.4586117343341698, -339.4245757958431113 ) ) ;
#89662 = CARTESIAN_POINT ( 'NONE',  ( -69.39269039516942428, -293.0639061606021869, -200.9830593273178181 ) ) ;
#89663 = CARTESIAN_POINT ( 'NONE',  ( -11.33672876627935189, -293.6990436908904485, -198.3537959456301678 ) ) ;
#89664 = CARTESIAN_POINT ( 'NONE',  ( -18.22254538749057673, -294.6321011485756003, -340.8129307803160941 ) ) ;
#89665 = CARTESIAN_POINT ( 'NONE',  ( 28.10039044746680048, -289.0632564918700496, -233.6170537162354606 ) ) ;
#89666 = CARTESIAN_POINT ( 'NONE',  ( 38.79440189358674473, -281.5706601735786876, -258.5134536059317156 ) ) ;
#89667 = CARTESIAN_POINT ( 'NONE',  ( -109.8480107706053275, -270.9742156050767221, -248.2015136030119606 ) ) ;
#89668 = CARTESIAN_POINT ( 'NONE',  ( -93.91829464007776096, -285.0973030077281010, -218.0518669750361482 ) ) ;
#89669 = CIRCLE ( 'NONE', #66993, 3.000000000000004885 ) ;
#89670 = CARTESIAN_POINT ( 'NONE',  ( 19.57864721398203045, -278.2034925973981103, -318.6510844766171999 ) ) ;
#89671 = EDGE_CURVE ( 'NONE', #2063, #88883, #68832, .T. ) ;
#89672 = CARTESIAN_POINT ( 'NONE',  ( -8.098805183234398797, -284.4348554765707036, -201.2417963333080877 ) ) ;
#89673 = CARTESIAN_POINT ( 'NONE',  ( -96.97166545007570448, -276.0567778406275465, -317.1005309045386298 ) ) ;
#89674 = DIRECTION ( 'NONE',  ( 0.000000000000000000, 0.000000000000000000, 1.000000000000000000 ) ) ;
#89675 = CARTESIAN_POINT ( 'NONE',  ( -42.94388623651373393, -282.6322750248692159, -343.2576875936265992 ) ) ;
#89676 = CIRCLE ( 'NONE', #3524, 24.00000000000000355 ) ;
#89677 = CARTESIAN_POINT ( 'NONE',  ( -71.07364184738068502, -280.8218972447962756, -201.5849242211563705 ) ) ;
#89678 = CARTESIAN_POINT ( 'NONE',  ( 39.36856562693941441, -286.6618503214559155, -274.4224749626239372 ) ) ;
#89679 = CARTESIAN_POINT ( 'NONE',  ( 19.62723108426097340, -295.9732243509820933, -317.6106141975219543 ) ) ;
#89680 = CARTESIAN_POINT ( 'NONE',  ( 34.45414767977475634, -277.4796374117198070, -296.0470743823016733 ) ) ;
#89681 = CARTESIAN_POINT ( 'NONE',  ( 9.197014594869811432, -275.9916088280801318, -209.6367711077459148 ) ) ;
#89682 = CARTESIAN_POINT ( 'NONE',  ( -109.6215042494474829, -278.5250331579922545, -259.7815659572450500 ) ) ;
#89683 = CARTESIAN_POINT ( 'NONE',  ( -107.8685235036640222, -274.8500381991245263, -245.9108830901979559 ) ) ;
#89684 = CARTESIAN_POINT ( 'NONE',  ( -7.501052274080759474, -284.4441422001780211, -201.7348535889083507 ) ) ;
#89685 = CARTESIAN_POINT ( 'NONE',  ( -101.6153986926417758, -291.6089879079249272, -311.3889997558484311 ) ) ;
#89686 = CIRCLE ( 'NONE', #35309, 4.025000000000000355 ) ;
#89687 = CARTESIAN_POINT ( 'NONE',  ( 27.76735225481852254, -292.0162625881526424, -236.6708023046132325 ) ) ;
#89688 = ORIENTED_EDGE ( 'NONE', *, *, #73573, .F. ) ;
#89689 = CARTESIAN_POINT ( 'NONE',  ( -64.07540055819274016, -291.3603113067068762, -202.3961520365329534 ) ) ;
#89690 = ORIENTED_EDGE ( 'NONE', *, *, #31275, .T. ) ;
#89691 = CARTESIAN_POINT ( 'NONE',  ( -15.02899007471783044, -289.8495555660354057, -343.7899098780044937 ) ) ;
#89692 = CARTESIAN_POINT ( 'NONE',  ( -72.18558837658798666, -280.2296655386205089, -206.0976281915633592 ) ) ;
#89693 = CARTESIAN_POINT ( 'NONE',  ( -91.40782768564372418, -296.2246694600536330, -215.9704353222274449 ) ) ;
#89694 = CARTESIAN_POINT ( 'NONE',  ( 14.54106201777362628, -288.9964586877092643, -327.1914694694860941 ) ) ;
#89695 = EDGE_CURVE ( 'NONE', #42343, #87260, #70339, .T. ) ;
#89696 = CARTESIAN_POINT ( 'NONE',  ( 38.76402612248147506, -287.7397053376743656, -258.7121262874467789 ) ) ;
#89697 = CARTESIAN_POINT ( 'NONE',  ( -98.12701881504915491, -285.4469649222994576, -229.8983879844416265 ) ) ;
#89698 = CARTESIAN_POINT ( 'NONE',  ( -22.45178514855419749, -108.0970913119723633, -362.6615123362100803 ) ) ;
#89699 = CARTESIAN_POINT ( 'NONE',  ( 119.9967176495213721, 149.6214322644071046, -262.1809137269642633 ) ) ;
#89700 = CARTESIAN_POINT ( 'NONE',  ( 166.9733864952704323, 230.1165055869454079, -189.8826931914318834 ) ) ;
#89701 = CARTESIAN_POINT ( 'NONE',  ( -13.74296406813424554, -275.9351860388663908, -339.6653729485777262 ) ) ;
#89702 = CARTESIAN_POINT ( 'NONE',  ( -87.31625309304148175, -276.6892941211253287, -323.9966484537966380 ) ) ;
#89703 = CARTESIAN_POINT ( 'NONE',  ( -111.7967352951812217, -272.4659885200412077, -250.6074206108544615 ) ) ;
#89704 = CARTESIAN_POINT ( 'NONE',  ( 154.7032878266783484, 204.3872195088065098, -214.8778263170268588 ) ) ;
#89705 = CARTESIAN_POINT ( 'NONE',  ( -64.93295899708127195, -276.0898287494861165, -341.7754456001293306 ) ) ;
#89706 = EDGE_LOOP ( 'NONE', ( #70069, #31400, #14060, #66514 ) ) ;
#89707 = CARTESIAN_POINT ( 'NONE',  ( -39.95393263892906077, -289.5780757828688365, -343.4255622367987826 ) ) ;
#89708 = CARTESIAN_POINT ( 'NONE',  ( -98.96906488981969119, -297.9668980725343204, -224.4455086316405357 ) ) ;
#89709 = CARTESIAN_POINT ( 'NONE',  ( -109.3777085860852338, -296.7006794720535368, -297.5362061286186872 ) ) ;
#89710 = CARTESIAN_POINT ( 'NONE',  ( 3.818136636171794773, -294.6473437734380809, -330.6509831510050503 ) ) ;
#89711 = ORIENTED_EDGE ( 'NONE', *, *, #92477, .T. ) ;
#89712 = AXIS2_PLACEMENT_3D ( 'NONE', #34352, #79767, #57541 ) ;
#89713 = CARTESIAN_POINT ( 'NONE',  ( -79.40389585043679688, -279.5349971063639032, -333.1941933107227669 ) ) ;
#89714 = ADVANCED_FACE ( 'NONE', ( #4149 ), #75183, .T. ) ;
#89715 = CARTESIAN_POINT ( 'NONE',  ( 11.44873081016254091, -281.9042857687664423, -329.9197245529882139 ) ) ;
#89716 = VECTOR ( 'NONE', #67661, 1000.000000000000000 ) ;
#89717 = CIRCLE ( 'NONE', #82163, 7.910944475430059519 ) ;
#89718 = CARTESIAN_POINT ( 'NONE',  ( -107.5270165688972952, -279.9109494194071885, -249.1892633164697202 ) ) ;
#89719 = CARTESIAN_POINT ( 'NONE',  ( 32.10288438361173746, -277.7112051631133340, -301.2062747073114224 ) ) ;
#89720 = CARTESIAN_POINT ( 'NONE',  ( -86.48037005042883152, -295.9282185874638458, -215.5818697765060961 ) ) ;
#89721 = PLANE ( 'NONE',  #89507 ) ;
#89722 = CARTESIAN_POINT ( 'NONE',  ( -83.00510463768449654, -277.8636661250710063, -327.3810119664037757 ) ) ;
#89723 = VECTOR ( 'NONE', #27252, 1000.000000000000000 ) ;
#89724 = CARTESIAN_POINT ( 'NONE',  ( 7.133180848106611904, -275.4434979990307966, -207.6368785608249539 ) ) ;
#89725 = CARTESIAN_POINT ( 'NONE',  ( 5.268687897342505089, -287.1734711991509243, -333.9036478670230395 ) ) ;
#89726 = CARTESIAN_POINT ( 'NONE',  ( -3.483820065667599497, -276.4991874008418904, -203.4241227442792308 ) ) ;
#89727 = CARTESIAN_POINT ( 'NONE',  ( 34.63973520401290074, -274.4547242220602925, -296.1544280080917702 ) ) ;
#89728 = CARTESIAN_POINT ( 'NONE',  ( 197.2550338912112409, 24.42483738579397823, 11.92230277053072562 ) ) ;
#89729 = CIRCLE ( 'NONE', #49007, 2.500000000000008882 ) ;
#89730 = CARTESIAN_POINT ( 'NONE',  ( -94.23629677755644707, -289.1001973245907379, -316.3568416929266505 ) ) ;
#89731 = ADVANCED_FACE ( 'NONE', ( #25446 ), #54323, .T. ) ;
#89732 = CARTESIAN_POINT ( 'NONE',  ( -111.0127099063557523, -283.6232389378021139, -292.4498882909786630 ) ) ;
#89733 = CARTESIAN_POINT ( 'NONE',  ( 32.30057180541375317, -280.1229499570794701, -295.5710139224876798 ) ) ;
#89735 = CARTESIAN_POINT ( 'NONE',  ( -110.0665815853239025, -282.8382930184193924, -254.4144102647672412 ) ) ;
#89734 = CARTESIAN_POINT ( 'NONE',  ( 28.67167796277082914, -280.5654193931208624, -302.9976018816071814 ) ) ;
#89736 = CARTESIAN_POINT ( 'NONE',  ( -42.15725490279448451, -291.1129995634192937, -345.2191098186257250 ) ) ;
#89737 = CARTESIAN_POINT ( 'NONE',  ( -72.33244455524882710, -280.7832386031947749, -205.8415216573589532 ) ) ;
#89738 = DIRECTION ( 'NONE',  ( -0.9531768234071978929, 0.3024135303179465439, -0.000000000000000000 ) ) ;
#89739 = CARTESIAN_POINT ( 'NONE',  ( -64.98120794621493701, -281.8071227091404012, -341.3857245747802835 ) ) ;
#89740 = CARTESIAN_POINT ( 'NONE',  ( 18.06970972713684631, -296.2584298839960866, -320.9796108451695886 ) ) ;
#89742 = CARTESIAN_POINT ( 'NONE',  ( -81.62983120171526252, -277.6982242743594611, -208.6153856801973348 ) ) ;
#89741 = AXIS2_PLACEMENT_3D ( 'NONE', #47367, #40259, #73273 ) ;
#89743 = CARTESIAN_POINT ( 'NONE',  ( -101.9431346154957936, -278.7381712298223420, -304.5743804698732333 ) ) ;
#89744 = CARTESIAN_POINT ( 'NONE',  ( -44.22533246178981159, -285.1390435861054016, -345.2640160457759748 ) ) ;
#89745 = CARTESIAN_POINT ( 'NONE',  ( 196.6005855419778641, 70.32660332368789113, 11.15032073793429568 ) ) ;
#89746 = CARTESIAN_POINT ( 'NONE',  ( -109.8572015051091029, -292.7436878732109449, -249.1286838525142855 ) ) ;
#89747 = AXIS2_PLACEMENT_3D ( 'NONE', #62456, #91299, #19818 ) ;
#89748 = CARTESIAN_POINT ( 'NONE',  ( -70.34881503073090414, -271.6169354810726304, -203.0147667888204239 ) ) ;
#89749 = CARTESIAN_POINT ( 'NONE',  ( 37.22261248932176869, -286.5166871011144849, -251.8051996535899377 ) ) ;
#89750 = CARTESIAN_POINT ( 'NONE',  ( -110.7668025937934289, -289.0489600255833125, -262.9318015864479889 ) ) ;
#89751 = CARTESIAN_POINT ( 'NONE',  ( -48.18343439339133027, -264.2011365548906383, -436.3931507628129225 ) ) ;
#89752 = CARTESIAN_POINT ( 'NONE',  ( -8.560885869508723545, -275.3522351774336130, -337.9980318598725830 ) ) ;
#89753 = CARTESIAN_POINT ( 'NONE',  ( -31.52887850723255880, -293.1177069419536565, -344.4193532260970301 ) ) ;
#89754 = CARTESIAN_POINT ( 'NONE',  ( 202.8019728163925492, 61.40723988820079171, 7.000000000000000000 ) ) ;
#89755 = CARTESIAN_POINT ( 'NONE',  ( -3.610238903460962323, -290.9690894537313852, -201.9004068496637672 ) ) ;
#89756 = CARTESIAN_POINT ( 'NONE',  ( -108.1280509493019650, -286.4275845287461379, -249.3094907452707218 ) ) ;
#89757 = CARTESIAN_POINT ( 'NONE',  ( 7.320561967526738378, -286.6928955798195489, -331.9016473640056688 ) ) ;
#89758 = CARTESIAN_POINT ( 'NONE',  ( 35.14461996519094100, -288.8075732341791877, -257.3812306982285349 ) ) ;
#89759 = DIRECTION ( 'NONE',  ( -0.2971780658744820891, 0.9548220761812652446, 0.000000000000000000 ) ) ;
#89760 = CARTESIAN_POINT ( 'NONE',  ( 17.95427823071062079, -289.0368565060061883, -318.3426870941156608 ) ) ;
#89761 = CARTESIAN_POINT ( 'NONE',  ( 36.44606664042736810, -295.3358420602150431, -255.0083620571739687 ) ) ;
#89762 = DIRECTION ( 'NONE',  ( 0.000000000000000000, 0.000000000000000000, 1.000000000000000000 ) ) ;
#89763 = CARTESIAN_POINT ( 'NONE',  ( 36.98780169253481631, -288.5242705936230436, -251.8372447611259020 ) ) ;
#89764 = CARTESIAN_POINT ( 'NONE',  ( -35.76651257513341875, -275.1124205830040523, -345.9175797689611045 ) ) ;
#89765 = CARTESIAN_POINT ( 'NONE',  ( -56.91455420214910532, -277.6310357544087992, -344.8651147841035822 ) ) ;
#89766 = CARTESIAN_POINT ( 'NONE',  ( -63.86008293881810260, -289.7890288565636752, -199.5522787797956141 ) ) ;
#89767 = CARTESIAN_POINT ( 'NONE',  ( -68.66003520145358152, -279.3184128645539772, -200.0267097626730219 ) ) ;
#89768 = CARTESIAN_POINT ( 'NONE',  ( -34.42409459764055413, -300.0687386000333277, -195.7153189856822735 ) ) ;
#89769 = CARTESIAN_POINT ( 'NONE',  ( -43.23635059700391992, -278.5233168282929910, -507.4184232499240466 ) ) ;
#89770 = CARTESIAN_POINT ( 'NONE',  ( -105.2868320042121297, -282.9708252739504246, -238.4818388863222935 ) ) ;
#89771 = CARTESIAN_POINT ( 'NONE',  ( -48.18343439339134449, -259.2200010662057821, -490.9919136893941527 ) ) ;
#89772 = CARTESIAN_POINT ( 'NONE',  ( -97.10120406042616992, -276.0845272991123807, -314.4240863681287124 ) ) ;
#89773 = CARTESIAN_POINT ( 'NONE',  ( 35.06112930142459305, -279.2998677739368532, -250.7462862747766223 ) ) ;
#89774 = CARTESIAN_POINT ( 'NONE',  ( -53.99892735073297700, -275.7419907114563671, -344.8816677552685519 ) ) ;
#89775 = CARTESIAN_POINT ( 'NONE',  ( -109.7303514691843418, -298.2535604188194611, -256.4883524508573487 ) ) ;
#89776 = CARTESIAN_POINT ( 'NONE',  ( 22.27426092079513609, -281.1222233881068746, -318.6252747122812821 ) ) ;
#89777 = CARTESIAN_POINT ( 'NONE',  ( -94.64289221352605352, -298.1353674368834845, -224.7543001308467012 ) ) ;
#89778 = CARTESIAN_POINT ( 'NONE',  ( -111.1508008949219573, -298.1233897627992064, -250.0277956969105162 ) ) ;
#89779 = CARTESIAN_POINT ( 'NONE',  ( 19.01787927376628673, -274.5610674547732515, -223.9317598509602476 ) ) ;
#89780 = CARTESIAN_POINT ( 'NONE',  ( 32.68696770348992686, -295.2032517795659601, -243.5099293965219545 ) ) ;
#89781 = CARTESIAN_POINT ( 'NONE',  ( 23.86014298253209986, -287.0956129528201473, -223.6133365455938815 ) ) ;
#89782 = CARTESIAN_POINT ( 'NONE',  ( -47.89304872393783086, -277.9989449497981582, -195.4886110040247331 ) ) ;
#89783 = CARTESIAN_POINT ( 'NONE',  ( -99.20332520864903358, -290.9952337031335219, -224.4899379185518740 ) ) ;
#89784 = EDGE_CURVE ( 'NONE', #58890, #73033, #17887, .T. ) ;
#89785 = CARTESIAN_POINT ( 'NONE',  ( 13.31092110019945629, -285.8402695796268063, -217.3976598597944871 ) ) ;
#89786 = CARTESIAN_POINT ( 'NONE',  ( -112.3891538888654793, -288.5414624955303680, -271.1808003295139997 ) ) ;
#89787 = ORIENTED_EDGE ( 'NONE', *, *, #80919, .T. ) ;
#89788 = CARTESIAN_POINT ( 'NONE',  ( 200.2349812190172713, 66.43136063442170780, 7.741079165001067963 ) ) ;
#89789 = AXIS2_PLACEMENT_3D ( 'NONE', #40003, #76488, #46181 ) ;
#89790 = CARTESIAN_POINT ( 'NONE',  ( 34.34331779029790255, -287.2467051061422580, -284.5412388223898574 ) ) ;
#89791 = DIRECTION ( 'NONE',  ( 0.5370370370370374236, 8.780046114482780452E-15, -0.8435586647355830525 ) ) ;
#89792 = CARTESIAN_POINT ( 'NONE',  ( -96.08250420123283675, -284.8256802426582226, -319.8014701400959439 ) ) ;
#89793 = CARTESIAN_POINT ( 'NONE',  ( 36.85824857785865305, -292.3632274944400251, -250.6332838989275160 ) ) ;
#89794 = CARTESIAN_POINT ( 'NONE',  ( 31.29195311423949022, -282.7217399448792321, -237.1359866008581605 ) ) ;
#89795 = CARTESIAN_POINT ( 'NONE',  ( 16.86182612839302664, -282.1192778667672769, -216.2935534489989493 ) ) ;
#89796 = APPLICATION_CONTEXT ( 'automotive_design' ) ;
#89797 = CARTESIAN_POINT ( 'NONE',  ( -66.56152234411779034, -283.2791404369732504, -337.2716397958188850 ) ) ;
#89798 = CARTESIAN_POINT ( 'NONE',  ( -99.92155132198499246, -297.1466648004941931, -225.4972993248834712 ) ) ;
#89799 = CIRCLE ( 'NONE', #80761, 1.000000000000000888 ) ;
#89800 = CARTESIAN_POINT ( 'NONE',  ( -107.6733376637402415, -274.1498483899442249, -248.8628631591116118 ) ) ;
#89801 = CARTESIAN_POINT ( 'NONE',  ( -38.90735864321626281, -290.0525215615998036, -195.7327351814898009 ) ) ;
#89802 = CARTESIAN_POINT ( 'NONE',  ( -96.59287825623330548, -271.9514021800117121, -226.9589390155948649 ) ) ;
#89803 = ORIENTED_EDGE ( 'NONE', *, *, #78924, .F. ) ;
#89804 = FACE_OUTER_BOUND ( 'NONE', #38014, .T. ) ;
#89805 = CARTESIAN_POINT ( 'NONE',  ( -109.7722178267710120, -286.6952035556068381, -253.1266692692933304 ) ) ;
#89806 = AXIS2_PLACEMENT_3D ( 'NONE', #35535, #58254, #64449 ) ;
#89807 = CARTESIAN_POINT ( 'NONE',  ( -66.79297008120266810, -296.5087523345606542, -341.1856787204346233 ) ) ;
#89808 = VECTOR ( 'NONE', #22075, 1000.000000000000114 ) ;
#89809 = CARTESIAN_POINT ( 'NONE',  ( -109.5231000566148509, -285.3569559644520837, -258.7172503771982406 ) ) ;
#89810 = CARTESIAN_POINT ( 'NONE',  ( -31.48023023705274426, -276.0387371632383520, -346.9541801191982131 ) ) ;
#89811 = CARTESIAN_POINT ( 'NONE',  ( -8.557082626845954110, -293.0705725152864147, -199.0536248140858220 ) ) ;
#89812 = CARTESIAN_POINT ( 'NONE',  ( 4.517305946693795704, -284.7496038322475442, -207.1469824801062884 ) ) ;
#89813 = CARTESIAN_POINT ( 'NONE',  ( -50.56689613274777884, -292.2209497488270813, -194.5268349564630626 ) ) ;
#89814 = CARTESIAN_POINT ( 'NONE',  ( -107.7450554036466031, -290.6272667590225751, -289.9240742387481191 ) ) ;
#89815 = DIRECTION ( 'NONE',  ( -1.000000000000000000, 0.000000000000000000, 0.000000000000000000 ) ) ;
#89816 = AXIS2_PLACEMENT_3D ( 'NONE', #35139, #83926, #84848 ) ;
#89817 = CARTESIAN_POINT ( 'NONE',  ( -39.80257052418233599, -229.5268262511776527, 25.50000000000000000 ) ) ;
#89818 = CARTESIAN_POINT ( 'NONE',  ( -54.88761368322284540, -169.8575745514222035, -360.7447470472093300 ) ) ;
#89819 = CARTESIAN_POINT ( 'NONE',  ( -98.79746901162829431, -286.6796149700505794, -225.0425659211572054 ) ) ;
#89820 = CARTESIAN_POINT ( 'NONE',  ( 36.60358173371529489, -272.6237833571633473, -234.7871824221999191 ) ) ;
#89821 = ORIENTED_EDGE ( 'NONE', *, *, #6894, .T. ) ;
#89822 = CARTESIAN_POINT ( 'NONE',  ( -34.84974809406566010, -281.9404765767924914, -343.6403546193134844 ) ) ;
#89823 = CARTESIAN_POINT ( 'NONE',  ( -74.09049100538294397, -277.1934562704336145, -338.0168632654421685 ) ) ;
#89824 = CARTESIAN_POINT ( 'NONE',  ( -41.16981823186733180, -282.0040053090052652, -195.6257586131330584 ) ) ;
#89825 = CARTESIAN_POINT ( 'NONE',  ( 27.39393885966332576, -24.46849793231620396, -343.6547034384808512 ) ) ;
#89826 = CARTESIAN_POINT ( 'NONE',  ( -19.07696777372116159, -281.3964061385267996, -344.6113786719984660 ) ) ;
#89827 = CARTESIAN_POINT ( 'NONE',  ( 34.62154628106470255, -285.3160390568893376, -250.5334108281160184 ) ) ;
#89828 = CARTESIAN_POINT ( 'NONE',  ( -37.27724884726870158, -299.8130847980922908, -194.3736719644936102 ) ) ;
#89829 = TOROIDAL_SURFACE ( 'NONE', #2184, 4.499999999999986677, 0.5000000000000000000 ) ;
#89830 = CARTESIAN_POINT ( 'NONE',  ( -18.19834555420284161, -295.2910223096777145, -340.8701274574840454 ) ) ;
#89831 = ORIENTED_EDGE ( 'NONE', *, *, #86831, .F. ) ;
#89832 = CARTESIAN_POINT ( 'NONE',  ( -14.67852482912937440, -291.0369281710678138, -200.4495741389052057 ) ) ;
#89833 = CARTESIAN_POINT ( 'NONE',  ( -101.8102993582165681, -279.7558828500485788, -228.3468240315060598 ) ) ;
#89834 = CARTESIAN_POINT ( 'NONE',  ( -4.104686705431316973, -274.5031169435301308, -205.3524627330299097 ) ) ;
#89835 = CARTESIAN_POINT ( 'NONE',  ( 37.60066400795967922, -274.6777176620538512, -286.7053776213849119 ) ) ;
#89836 = DIRECTION ( 'NONE',  ( 0.000000000000000000, 1.000000000000000000, 0.000000000000000000 ) ) ;
#89837 = CARTESIAN_POINT ( 'NONE',  ( -52.72996239112953276, -271.8549484850714180, -196.9042698117588941 ) ) ;
#89838 = CARTESIAN_POINT ( 'NONE',  ( -16.64886731540296338, -296.2153200427665070, -343.9714416967875081 ) ) ;
#89839 = CARTESIAN_POINT ( 'NONE',  ( 193.9646936176697523, 21.00000000000000000, 15.00000000000057909 ) ) ;
#89840 = CARTESIAN_POINT ( 'NONE',  ( -43.35439945481423507, -267.5770695277309983, -504.1101809961486993 ) ) ;
#89841 = CARTESIAN_POINT ( 'NONE',  ( -61.62419700654685073, -284.4547478530649869, -339.5852801861693706 ) ) ;
#89842 = CARTESIAN_POINT ( 'NONE',  ( 4.013252073238731121, -284.2638766398117127, -334.1708030930938094 ) ) ;
#89843 = CARTESIAN_POINT ( 'NONE',  ( -96.65267670545426881, -284.4977436308168421, -227.6068667201013511 ) ) ;
#89844 = CARTESIAN_POINT ( 'NONE',  ( -36.47702481675179342, -275.4410438882899825, -344.1686593674873507 ) ) ;
#89845 = CARTESIAN_POINT ( 'NONE',  ( -40.25958646312011524, -284.9496379451209123, -344.5389544407888138 ) ) ;
#89846 = CARTESIAN_POINT ( 'NONE',  ( -35.11590675149710705, -275.5035730322827590, -344.0208328738047499 ) ) ;
#89847 = CARTESIAN_POINT ( 'NONE',  ( -8.863391098975974103, -275.5132116173144823, -202.7554329741854815 ) ) ;
#89848 = CARTESIAN_POINT ( 'NONE',  ( 196.0143093133015384, 42.36571313990103249, 11.99999999999998757 ) ) ;
#89849 = CARTESIAN_POINT ( 'NONE',  ( -67.30893073698736373, -280.4718600113618550, -199.6071505291407959 ) ) ;
#89850 = EDGE_CURVE ( 'NONE', #10831, #6353, #86992, .T. ) ;
#89851 = ORIENTED_EDGE ( 'NONE', *, *, #29441, .T. ) ;
#89852 = CARTESIAN_POINT ( 'NONE',  ( 201.2104617360081704, 15.00000000000000533, 10.00000000000000178 ) ) ;
#89853 = CARTESIAN_POINT ( 'NONE',  ( 38.46692529297811802, -289.4271534675118005, -271.5085520155910217 ) ) ;
#89854 = CARTESIAN_POINT ( 'NONE',  ( -34.30470247405479256, -294.2101596997219985, -343.4595336464529964 ) ) ;
#89855 = EDGE_CURVE ( 'NONE', #39909, #81433, #2748, .T. ) ;
#89856 = CARTESIAN_POINT ( 'NONE',  ( -111.8253781160310041, -289.6605803078348913, -289.5317281382592682 ) ) ;
#89857 = CARTESIAN_POINT ( 'NONE',  ( -4.119895180196953000, -284.7362822176437476, -204.2227350859878072 ) ) ;
#89859 = CARTESIAN_POINT ( 'NONE',  ( -80.09807245662983632, -289.7048138470740923, -209.8841849596891223 ) ) ;
#89858 = CARTESIAN_POINT ( 'NONE',  ( 33.96398600394710598, -285.8881044716035831, -252.1202626243413363 ) ) ;
#89860 = CARTESIAN_POINT ( 'NONE',  ( -8.110837002141366270, -287.6488603328508589, -203.0358838827385455 ) ) ;
#89861 = CARTESIAN_POINT ( 'NONE',  ( -81.39271181780156894, -275.6511190905586659, -331.0612746139123601 ) ) ;
#89862 = CARTESIAN_POINT ( 'NONE',  ( 37.32031443120019532, -286.1445309829779262, -285.5934520003472699 ) ) ;
#89863 = CARTESIAN_POINT ( 'NONE',  ( -36.61118143951127024, -288.0614788422674337, -195.3519716531124004 ) ) ;
#89864 = CARTESIAN_POINT ( 'NONE',  ( 33.14412335963569234, -285.2138356135331492, -244.2502560263469036 ) ) ;
#89865 = CARTESIAN_POINT ( 'NONE',  ( 35.80151961470608057, -282.5416835992856477, -274.0323375544222131 ) ) ;
#89866 = CARTESIAN_POINT ( 'NONE',  ( 20.99872652587955102, -290.2038471282730256, -317.7778294364557610 ) ) ;
#89867 = CARTESIAN_POINT ( 'NONE',  ( 83.14890176555634582, -299.5541904835127980, -197.2570935515975918 ) ) ;
#89868 = CARTESIAN_POINT ( 'NONE',  ( 154.3120505024585327, 19.86534941647301977, -13.70129228612095673 ) ) ;
#89869 = CARTESIAN_POINT ( 'NONE',  ( -109.4464886090978837, -298.7635182668197444, -247.5995829736514793 ) ) ;
#89870 = CARTESIAN_POINT ( 'NONE',  ( 36.18652026696772595, -279.7426621459921989, -285.2108185068661328 ) ) ;
#89871 = CARTESIAN_POINT ( 'NONE',  ( -34.95516457603115867, -291.2785498861794622, -193.5465420314574203 ) ) ;
#89872 = CARTESIAN_POINT ( 'NONE',  ( -110.5268743519827410, -295.0810902075823492, -260.4695318092544198 ) ) ;
#89873 = CARTESIAN_POINT ( 'NONE',  ( 3.651497655673336951, -281.1730013320150192, -331.4210378835179540 ) ) ;
#89874 = CARTESIAN_POINT ( 'NONE',  ( 32.47723748092739982, -273.2943781902573619, -244.5419362090048878 ) ) ;
#89875 = CARTESIAN_POINT ( 'NONE',  ( -95.15104289980627073, -297.2316850054183988, -315.7408862491202513 ) ) ;
#89876 = DIRECTION ( 'NONE',  ( -1.000000000000000000, 0.000000000000000000, 0.000000000000000000 ) ) ;
#89877 = CARTESIAN_POINT ( 'NONE',  ( -20.67871297045058654, -296.7370723534652939, -194.0586629801171341 ) ) ;
#89878 = CARTESIAN_POINT ( 'NONE',  ( 25.65889246766253962, -292.3592539969980635, -312.8452249672719745 ) ) ;
#89879 = AXIS2_PLACEMENT_3D ( 'NONE', #3910, #90971, #69238 ) ;
#89880 = CARTESIAN_POINT ( 'NONE',  ( 139.6539576904058606, 275.0000000000000568, -10.49999999999999822 ) ) ;
#89881 = CARTESIAN_POINT ( 'NONE',  ( 33.27524152560594217, -294.6076599488613965, -289.5359632295803181 ) ) ;
#89882 = CARTESIAN_POINT ( 'NONE',  ( 196.0143093133015384, 20.19615242270663913, 11.99999999999998757 ) ) ;
#89884 = CARTESIAN_POINT ( 'NONE',  ( 17.97243039637194428, -294.2307742803172346, -318.0178407332722941 ) ) ;
#89883 = CARTESIAN_POINT ( 'NONE',  ( -47.06954514272372592, -281.1952504626975156, -345.0857848100808383 ) ) ;
#89885 = CARTESIAN_POINT ( 'NONE',  ( -13.42193596962568414, -282.7499011540667198, -343.5515878717734495 ) ) ;
#89886 = CARTESIAN_POINT ( 'NONE',  ( 14.16158275542191447, -282.6884595793933954, -215.0019489326299720 ) ) ;
#89887 = CARTESIAN_POINT ( 'NONE',  ( -54.95564823339118732, -285.4983639566385705, -195.4245239608235067 ) ) ;
#89888 = ADVANCED_FACE ( 'NONE', ( #89355 ), #24511, .F. ) ;
#89889 = CARTESIAN_POINT ( 'NONE',  ( -110.9875841250319723, -288.3811207866403947, -283.6393783691144108 ) ) ;
#89890 = CARTESIAN_POINT ( 'NONE',  ( 38.11214887289218467, -279.8841303986320099, -258.6413628431546954 ) ) ;
#89891 = VECTOR ( 'NONE', #24599, 1000.000000000000114 ) ;
#89892 = CARTESIAN_POINT ( 'NONE',  ( -12.33755586500258339, -287.6548295491841145, -342.9170043981440017 ) ) ;
#89893 = CARTESIAN_POINT ( 'NONE',  ( 196.3496553477289979, 250.5000000000000568, -12.41762739670150850 ) ) ;
#89894 = CARTESIAN_POINT ( 'NONE',  ( -5.174593117775942552, -296.2216817528400838, -336.7958443613134705 ) ) ;
#89895 = CARTESIAN_POINT ( 'NONE',  ( -62.19703594111321365, -278.7943127760404991, -342.6722225098698118 ) ) ;
#89897 = CARTESIAN_POINT ( 'NONE',  ( -91.30958548241221706, -278.9240228655258989, -221.1721472961937707 ) ) ;
#89896 = CARTESIAN_POINT ( 'NONE',  ( 37.80279614241336361, -291.5002937487391819, -264.7298232078958335 ) ) ;
#89898 = CARTESIAN_POINT ( 'NONE',  ( 8.849230703342058746, -292.8324343640053939, -208.6877723966226768 ) ) ;
#89899 = CARTESIAN_POINT ( 'NONE',  ( -111.7239106847011811, -282.4589670732569289, -283.9380352956530373 ) ) ;
#89900 = CARTESIAN_POINT ( 'NONE',  ( -74.32716041703696419, -279.5441218682748854, -335.6073927946701474 ) ) ;
#89901 = CARTESIAN_POINT ( 'NONE',  ( 23.54350313674527584, -292.0475267887983364, -229.6622178550532567 ) ) ;
#89902 = CARTESIAN_POINT ( 'NONE',  ( -95.50094917528325311, -271.2071589797232605, -222.7224496431605587 ) ) ;
#89903 = VERTEX_POINT ( 'NONE', #57613 ) ;
#89904 = DIRECTION ( 'NONE',  ( 0.000000000000000000, 1.000000000000000000, 0.000000000000000000 ) ) ;
#89905 = CARTESIAN_POINT ( 'NONE',  ( 1.597331475843968507, -294.0242067541956317, -332.2412583215452742 ) ) ;
#89906 = DIRECTION ( 'NONE',  ( -1.000000000000000000, 2.653393457432135558E-15, 0.000000000000000000 ) ) ;
#89907 = CARTESIAN_POINT ( 'NONE',  ( -21.39648532958014826, -286.3380690714489560, -340.3683826091709079 ) ) ;
#89908 = CARTESIAN_POINT ( 'NONE',  ( -82.82150239962889771, -296.5061975434459214, -208.4532835692209005 ) ) ;
#89909 = EDGE_CURVE ( 'NONE', #34073, #54318, #48616, .T. ) ;
#89910 = ADVANCED_FACE ( 'NONE', ( #34896 ), #41021, .T. ) ;
#89911 = CARTESIAN_POINT ( 'NONE',  ( -33.76723103276980709, -287.4114192802107368, -193.9378136556935033 ) ) ;
#89912 = CARTESIAN_POINT ( 'NONE',  ( 14.08187707290968049, -288.1384062289997701, -322.1743953576719832 ) ) ;
#89913 = CARTESIAN_POINT ( 'NONE',  ( -101.1738028703902046, -279.5708470231476213, -307.2897784851741676 ) ) ;
#89914 = CARTESIAN_POINT ( 'NONE',  ( -75.75548366577658044, -299.2923768206337058, -207.0375180098544092 ) ) ;
#89915 = CARTESIAN_POINT ( 'NONE',  ( -98.31495743973337653, -277.9125917595251849, -229.4126990596184612 ) ) ;
#89916 = VERTEX_POINT ( 'NONE', #49103 ) ;
#89917 = CARTESIAN_POINT ( 'NONE',  ( -91.61761176654559335, -296.9709393805669606, -215.7729351286436383 ) ) ;
#89918 = CARTESIAN_POINT ( 'NONE',  ( -85.60033671758756668, -291.6455633707108177, -327.1073345188580674 ) ) ;
#89919 = CARTESIAN_POINT ( 'NONE',  ( 31.45483283253144791, -294.7264885315386778, -237.4745970609529309 ) ) ;
#89920 = DIRECTION ( 'NONE',  ( 0.000000000000000000, 1.000000000000000000, 0.000000000000000000 ) ) ;
#89921 = CARTESIAN_POINT ( 'NONE',  ( -97.42796936618576353, -290.6240069292109638, -312.0188232723045871 ) ) ;
#89922 = CARTESIAN_POINT ( 'NONE',  ( 196.5878321470269157, 70.38283977259966662, 11.16596772118615988 ) ) ;
#89923 = CARTESIAN_POINT ( 'NONE',  ( -5.107791317458369562, -290.6115325695580509, -201.7952328262568642 ) ) ;
#89924 = CARTESIAN_POINT ( 'NONE',  ( -99.07802444478326720, -297.4974225790109017, -224.3568313837498636 ) ) ;
#89925 = CARTESIAN_POINT ( 'NONE',  ( -96.89752427075154628, -296.8086887944205046, -228.1095937792574944 ) ) ;
#89926 = CARTESIAN_POINT ( 'NONE',  ( 165.2494399300530290, 8.542400036368780647, -9.000000000000001776 ) ) ;
#89927 = CARTESIAN_POINT ( 'NONE',  ( 82.64890176555634582, -299.5541904835127980, -195.3611179825600175 ) ) ;
#89928 = CARTESIAN_POINT ( 'NONE',  ( -96.73807863619954617, -291.4240148852437642, -318.2855591002485767 ) ) ;
#89929 = CARTESIAN_POINT ( 'NONE',  ( -115.3430155898818299, -293.2662352645559167, -252.5904736702033517 ) ) ;
#89930 = CARTESIAN_POINT ( 'NONE',  ( 26.50187938659362530, -289.0275910420738796, -231.3223452077258457 ) ) ;
#89931 = CARTESIAN_POINT ( 'NONE',  ( 32.84646208357424513, -273.2143846631282713, -244.4063436589451612 ) ) ;
#89932 = CARTESIAN_POINT ( 'NONE',  ( 21.16921154658293602, -278.1090717182042908, -316.4010783418359551 ) ) ;
#89933 = CARTESIAN_POINT ( 'NONE',  ( -32.03061151134350126, -290.1994883993817211, -196.0979521634439209 ) ) ;
#89934 = CARTESIAN_POINT ( 'NONE',  ( -79.51858870759124898, -279.4752685990683858, -333.3640381407938094 ) ) ;
#89935 = ORIENTED_EDGE ( 'NONE', *, *, #71254, .T. ) ;
#89936 = CARTESIAN_POINT ( 'NONE',  ( 17.67611166433070480, -281.5865838464993658, -318.4956487684563058 ) ) ;
#89937 = CARTESIAN_POINT ( 'NONE',  ( -97.67717078006829468, -278.9963892631488989, -317.7016238148365233 ) ) ;
#89938 = CARTESIAN_POINT ( 'NONE',  ( 27.52334373093404807, -279.8096424740933799, -229.5120189446091388 ) ) ;
#89939 = VECTOR ( 'NONE', #18002, 1000.000000000000000 ) ;
#89940 = CARTESIAN_POINT ( 'NONE',  ( -113.1080972910931024, -270.6751398228194034, -270.3372191192045761 ) ) ;
#89941 = CARTESIAN_POINT ( 'NONE',  ( 38.68947411932053626, -276.3605926166272297, -259.7742980904465639 ) ) ;
#89942 = CARTESIAN_POINT ( 'NONE',  ( -27.10883676588594682, -275.6999603168554813, -194.6907365096304829 ) ) ;
#89943 = CARTESIAN_POINT ( 'NONE',  ( 31.03373250439201669, -301.4082689599840705, -195.3320873922940848 ) ) ;
#89944 = ORIENTED_EDGE ( 'NONE', *, *, #83917, .F. ) ;
#89945 = VERTEX_POINT ( 'NONE', #5087 ) ;
#89946 = EDGE_CURVE ( 'NONE', #91341, #37341, #20225, .T. ) ;
#89947 = DIRECTION ( 'NONE',  ( -1.000000000000000000, -0.000000000000000000, -0.000000000000000000 ) ) ;
#89948 = CARTESIAN_POINT ( 'NONE',  ( -50.79475610227913762, -290.3076064726240588, -342.4771613618003698 ) ) ;
#89949 = CARTESIAN_POINT ( 'NONE',  ( -99.83429374786048527, -291.7337639988218712, -313.5889996891918940 ) ) ;
#89950 = CARTESIAN_POINT ( 'NONE',  ( -109.0403350769879012, -289.7121110847018599, -284.6799490144572360 ) ) ;
#89951 = CARTESIAN_POINT ( 'NONE',  ( 30.08065940350859435, -286.5781675359449991, -233.1863923119585706 ) ) ;
#89952 = CARTESIAN_POINT ( 'NONE',  ( 200.5559520117673458, 215.0000000000000568, -2.971689740512053035 ) ) ;
#89953 = CARTESIAN_POINT ( 'NONE',  ( 35.26893285779855347, -280.1251340339272815, -283.6278980665212543 ) ) ;
#89954 = CARTESIAN_POINT ( 'NONE',  ( -18.13139690053984054, -290.6624792496601799, -342.1211510195499272 ) ) ;
#89955 = CARTESIAN_POINT ( 'NONE',  ( -13.32149529327954340, -281.2144630202237749, -340.0839961675785617 ) ) ;
#89956 = CARTESIAN_POINT ( 'NONE',  ( 30.47012436447508676, -282.4897937925332485, -242.0273936280131011 ) ) ;
#89957 = CARTESIAN_POINT ( 'NONE',  ( -4.423062348311134429, -289.5701354822533062, -339.7238313491587292 ) ) ;
#89958 = CARTESIAN_POINT ( 'NONE',  ( -106.3202312655517687, -278.7226032226615189, -294.5966783749041156 ) ) ;
#89959 = CARTESIAN_POINT ( 'NONE',  ( -111.9271295817409708, -289.5666440736679874, -252.8962265219410028 ) ) ;
#89960 = AXIS2_PLACEMENT_3D ( 'NONE', #13234, #78092, #19841 ) ;
#89961 = CARTESIAN_POINT ( 'NONE',  ( -97.46046614397103269, -285.9969746689826593, -222.5082936754134266 ) ) ;
#89962 = CARTESIAN_POINT ( 'NONE',  ( -83.24419353751396500, -285.9348222748192825, -208.5493295224553378 ) ) ;
#89963 = CARTESIAN_POINT ( 'NONE',  ( -73.79495122221321424, -283.7169860311362299, -333.6655429074372137 ) ) ;
#89964 = VERTEX_POINT ( 'NONE', #57161 ) ;
#89965 = DIRECTION ( 'NONE',  ( 0.000000000000000000, 0.000000000000000000, 1.000000000000000000 ) ) ;
#89966 = CARTESIAN_POINT ( 'NONE',  ( -63.97711796632140846, -293.5689891483524434, -199.3772824239310637 ) ) ;
#89967 = CARTESIAN_POINT ( 'NONE',  ( -3.462327495357582663, -293.2991735245171299, -338.9721750415013730 ) ) ;
#89968 = CARTESIAN_POINT ( 'NONE',  ( -76.49169910805632355, -276.6483234226089962, -332.3133016373562896 ) ) ;
#89969 = CARTESIAN_POINT ( 'NONE',  ( -112.2084711431010646, -295.6801526898366319, -287.9759849426580445 ) ) ;
#89970 = CARTESIAN_POINT ( 'NONE',  ( -25.27669040141606871, -290.6884702498393835, -197.6101573193406580 ) ) ;
#89971 = CARTESIAN_POINT ( 'NONE',  ( -6.360878613344971733, -292.8793467238133417, -337.5783978623062467 ) ) ;
#89972 = CARTESIAN_POINT ( 'NONE',  ( -30.78671084144532699, -293.3419363980237335, -197.2573381877226382 ) ) ;
#89973 = FACE_OUTER_BOUND ( 'NONE', #57291, .T. ) ;
#89974 = CARTESIAN_POINT ( 'NONE',  ( 16.20199196301189204, -290.8091783406275681, -217.5326901332017826 ) ) ;
#89975 = CARTESIAN_POINT ( 'NONE',  ( 36.63390184229079694, -295.3898195050147706, -257.7057802422615396 ) ) ;
#89976 = CARTESIAN_POINT ( 'NONE',  ( 31.62499701618000358, -288.8203895685710449, -294.9985515516568739 ) ) ;
#89977 = CARTESIAN_POINT ( 'NONE',  ( -35.72105268046706072, -279.0118359600550093, -345.7117356905076804 ) ) ;
#89978 = CARTESIAN_POINT ( 'NONE',  ( -68.86606538362335073, -276.2523913870165870, -340.1910864744706942 ) ) ;
#89979 = CARTESIAN_POINT ( 'NONE',  ( -48.93550933732409192, -297.1053589863586808, -194.3487443504060650 ) ) ;
#89980 = CARTESIAN_POINT ( 'NONE',  ( -66.61387008749871086, -277.7455892132325062, -201.9041390836186167 ) ) ;
#89981 = CARTESIAN_POINT ( 'NONE',  ( -98.17716941829219479, -276.3343318637661810, -316.2681162950927956 ) ) ;
#89982 = CARTESIAN_POINT ( 'NONE',  ( -110.5922315924300534, -295.1509359700516484, -276.9271489052590596 ) ) ;
#89983 = DIRECTION ( 'NONE',  ( 1.000000000000000000, 0.000000000000000000, 0.000000000000000000 ) ) ;
#89984 = CARTESIAN_POINT ( 'NONE',  ( -110.4439418194319558, -273.2393927828638311, -267.6417298770065827 ) ) ;
#89985 = DIRECTION ( 'NONE',  ( -1.000000000000000000, 0.000000000000000000, 0.000000000000000000 ) ) ;
#89987 = CARTESIAN_POINT ( 'NONE',  ( 13.49817791269440548, -274.6218043813393024, -217.9749861794490471 ) ) ;
#89986 = CARTESIAN_POINT ( 'NONE',  ( 4.620051286339034391, -286.5088600877796807, -332.9519976615662813 ) ) ;
#89988 = CARTESIAN_POINT ( 'NONE',  ( 5.557323458068381683, -288.4884333716127003, -334.3038562360549690 ) ) ;
#89989 = CARTESIAN_POINT ( 'NONE',  ( -20.98175107099430647, -300.2358698884595469, -195.0004213312810180 ) ) ;
#89990 = CARTESIAN_POINT ( 'NONE',  ( -96.23156543239005600, -293.9168872290219383, -316.5348355649385326 ) ) ;
#89991 = CARTESIAN_POINT ( 'NONE',  ( -31.65845397940219286, -282.1793319711410390, -347.0024177934992053 ) ) ;
#89992 = EDGE_CURVE ( 'NONE', #14615, #52785, #78914, .T. ) ;
#89993 = CARTESIAN_POINT ( 'NONE',  ( 153.7504314680575987, 128.6410103095127226, -12.94315874461255689 ) ) ;
#89994 = CARTESIAN_POINT ( 'NONE',  ( -105.6853938518041076, -276.9585912438295736, -239.3474525068313312 ) ) ;
#89995 = CARTESIAN_POINT ( 'NONE',  ( 197.4657836131030706, 215.0000000000000568, -12.48225014817974987 ) ) ;
#89996 = CARTESIAN_POINT ( 'NONE',  ( -55.09361898898775678, -290.6136367259565532, -199.1431435632293017 ) ) ;
#89997 = CARTESIAN_POINT ( 'NONE',  ( 197.9510320457498551, 42.14527911255801484, 11.14415317764935587 ) ) ;
#89998 = DIRECTION ( 'NONE',  ( 0.000000000000000000, -0.000000000000000000, 1.000000000000000000 ) ) ;
#89999 = CARTESIAN_POINT ( 'NONE',  ( -80.66580624260511456, -289.4648332342621870, -209.0763803563716010 ) ) ;
#90000 = CARTESIAN_POINT ( 'NONE',  ( -6.253936451024444843, -275.9883323341943537, -203.5460096308692926 ) ) ;
#90001 = CARTESIAN_POINT ( 'NONE',  ( 22.07661768964510429, -283.6267616130615465, -318.4241436015711884 ) ) ;
#90003 = CARTESIAN_POINT ( 'NONE',  ( -94.28501196460319989, -283.9064458894444556, -316.0587792790577737 ) ) ;
#90002 = CARTESIAN_POINT ( 'NONE',  ( 29.00626007061389089, -296.8988656039310285, -195.0281631133275084 ) ) ;
#90004 = CARTESIAN_POINT ( 'NONE',  ( -54.36531900083412694, -275.2544331140441045, -198.7680225340782556 ) ) ;
#90005 = CARTESIAN_POINT ( 'NONE',  ( 7.421663323858610717, -275.4835860584792044, -212.4919291262028196 ) ) ;
#90006 = CARTESIAN_POINT ( 'NONE',  ( 33.72245909192765367, -283.8642270597196102, -294.4994570755767427 ) ) ;
#90007 = ORIENTED_EDGE ( 'NONE', *, *, #14648, .F. ) ;
#90008 = CARTESIAN_POINT ( 'NONE',  ( 208.3418117619747818, 38.42745601219718310, 12.00000000000000000 ) ) ;
#90009 = CARTESIAN_POINT ( 'NONE',  ( 39.23683374338022389, -293.4922253118551794, -278.8969769189378667 ) ) ;
#90010 = CARTESIAN_POINT ( 'NONE',  ( -106.1227554609115771, -286.9142439715722048, -241.2279264058203694 ) ) ;
#90011 = LINE ( 'NONE', #51701, #3467 ) ;
#90012 = CARTESIAN_POINT ( 'NONE',  ( -115.3288506153726871, -270.2666405000204009, -252.5284128619063608 ) ) ;
#90013 = CARTESIAN_POINT ( 'NONE',  ( -51.29335182039595509, -276.4233504259822780, -345.9224191563960176 ) ) ;
#90014 = EDGE_CURVE ( 'NONE', #60939, #87677, #56701, .T. ) ;
#90015 = CARTESIAN_POINT ( 'NONE',  ( -111.7881649066637095, -288.7466284839798050, -286.6142500018415831 ) ) ;
#90016 = CARTESIAN_POINT ( 'NONE',  ( -100.2108334420428832, -286.5981973201796791, -231.8167487287633719 ) ) ;
#90017 = CIRCLE ( 'NONE', #74986, 0.5000000000000004441 ) ;
#90018 = CARTESIAN_POINT ( 'NONE',  ( -70.89239331583017645, -279.2612618837947593, -336.3332712183571971 ) ) ;
#90019 = CARTESIAN_POINT ( 'NONE',  ( -49.27078224464337808, -287.3283742385361279, -194.8339336776473374 ) ) ;
#90020 = CARTESIAN_POINT ( 'NONE',  ( -30.09378542254856370, -282.1438988379376269, -195.6604158146076884 ) ) ;
#90021 = CARTESIAN_POINT ( 'NONE',  ( 39.55419714377931939, -275.6572572191269614, -265.4376621109302619 ) ) ;
#90022 = CARTESIAN_POINT ( 'NONE',  ( -84.86804626794169337, -277.5201096972257346, -331.0114285673242307 ) ) ;
#90023 = CARTESIAN_POINT ( 'NONE',  ( -72.36368689922639419, -299.5051649154558504, -204.6596937049019402 ) ) ;
#90024 = CARTESIAN_POINT ( 'NONE',  ( 156.5008572374906066, 15.54442400203491026, 9.984260581292296877 ) ) ;
#90025 = CARTESIAN_POINT ( 'NONE',  ( -85.33152481854864391, -281.9090924074130839, -210.2361428286349110 ) ) ;
#90026 = ADVANCED_FACE ( 'NONE', ( #50021 ), #49565, .T. ) ;
#90027 = CARTESIAN_POINT ( 'NONE',  ( -23.61459040309954105, -296.3618478091602242, -194.6006057249171022 ) ) ;
#90028 = CARTESIAN_POINT ( 'NONE',  ( 140.6539576904058606, 250.0000000000000568, -10.49999999999999822 ) ) ;
#90029 = CARTESIAN_POINT ( 'NONE',  ( -69.28397759739200978, -276.9917183236604501, -336.0840179051645578 ) ) ;
#90030 = CARTESIAN_POINT ( 'NONE',  ( -94.79886426350851991, -274.4467380231901075, -219.6986761869628424 ) ) ;
#90031 = CARTESIAN_POINT ( 'NONE',  ( 28.09813090857735673, -281.1379961476027916, -310.5922256237240617 ) ) ;
#90032 = CARTESIAN_POINT ( 'NONE',  ( 16.69924425416339631, -288.5944773308765434, -219.7701927582697579 ) ) ;
#90033 = CARTESIAN_POINT ( 'NONE',  ( -92.18511600274811713, -297.3387870389506702, -323.4168197256554436 ) ) ;
#90034 = CARTESIAN_POINT ( 'NONE',  ( -39.08335000664671099, -296.2786235757576492, -346.9442452079462669 ) ) ;
#90035 = CARTESIAN_POINT ( 'NONE',  ( -16.95706390093824112, -294.3160089804863446, -198.3037731900492133 ) ) ;
#90036 = CARTESIAN_POINT ( 'NONE',  ( -70.53102447828852917, -277.6134202975084690, -203.2760907243010138 ) ) ;
#90037 = CARTESIAN_POINT ( 'NONE',  ( 3.473493612593856028, -282.5253630614609506, -208.0462942103282273 ) ) ;
#90038 = CARTESIAN_POINT ( 'NONE',  ( -58.28699278625388303, -295.8591700093917893, -198.9285700023416155 ) ) ;
#90039 = CARTESIAN_POINT ( 'NONE',  ( -113.5540968977842482, -286.1209057257423751, -272.8437134375274127 ) ) ;
#90040 = CARTESIAN_POINT ( 'NONE',  ( 30.25209705113452685, -286.0917412910500275, -241.8517075044405544 ) ) ;
#90041 = CARTESIAN_POINT ( 'NONE',  ( -88.13691865063097453, -231.3408449674847702, -347.3187200103926102 ) ) ;
#90042 = VERTEX_POINT ( 'NONE', #41977 ) ;
#90043 = CARTESIAN_POINT ( 'NONE',  ( 34.58897289824625432, -287.0493038545163813, -257.5033832534419389 ) ) ;
#90044 = EDGE_LOOP ( 'NONE', ( #89069, #17389, #66652, #12307 ) ) ;
#90045 = CARTESIAN_POINT ( 'NONE',  ( -63.79245144485228280, -284.4687785119766090, -342.3461877144193863 ) ) ;
#90046 = CARTESIAN_POINT ( 'NONE',  ( 2.938067282751138709, -274.9423024915284941, -209.3939758896729018 ) ) ;
#90047 = CARTESIAN_POINT ( 'NONE',  ( 16.03357058837823246, -285.5838686363346142, -215.4148788587463343 ) ) ;
#90048 = CARTESIAN_POINT ( 'NONE',  ( -98.09492390808233608, -290.0997878408114161, -223.5366871470241676 ) ) ;
#90049 = CARTESIAN_POINT ( 'NONE',  ( 38.94753206673036061, -282.3805555496907118, -261.3655998634806110 ) ) ;
#90050 = CARTESIAN_POINT ( 'NONE',  ( -94.45581688582235813, -280.7640520483145679, -219.7579024668104637 ) ) ;
#90051 = CARTESIAN_POINT ( 'NONE',  ( 22.50950570810978846, -282.5349472567730231, -318.7924266976679633 ) ) ;
#90052 = CARTESIAN_POINT ( 'NONE',  ( -37.30987171927208834, -277.5523547857346784, -200.3611179825600459 ) ) ;
#90053 = CARTESIAN_POINT ( 'NONE',  ( 174.8075198983063956, 243.0437970287033522, -179.7850249908958347 ) ) ;
#90054 = VERTEX_POINT ( 'NONE', #6021 ) ;
#90055 = CARTESIAN_POINT ( 'NONE',  ( 8.728621298072505752, -278.4196222335515358, -329.3979537630773393 ) ) ;
#90056 = CARTESIAN_POINT ( 'NONE',  ( -114.3264802394368189, -272.8779462956648558, -270.3652661221577205 ) ) ;
#90057 = CARTESIAN_POINT ( 'NONE',  ( 23.92059713507495999, -280.1536162727486499, -313.0082484570966130 ) ) ;
#90058 = CARTESIAN_POINT ( 'NONE',  ( 0.06149831950429140298, -296.3215892981411912, -336.5196919456309388 ) ) ;
#90059 = CARTESIAN_POINT ( 'NONE',  ( -58.44558161531324458, -294.6808956684941450, -340.3505375693898714 ) ) ;
#90060 = CARTESIAN_POINT ( 'NONE',  ( -98.29566159531329106, -290.6870168510663461, -223.3915173916311403 ) ) ;
#90061 = FACE_OUTER_BOUND ( 'NONE', #26744, .T. ) ;
#90062 = EDGE_CURVE ( 'NONE', #56456, #14859, #14061, .T. ) ;
#90064 = CARTESIAN_POINT ( 'NONE',  ( 20.97723512376344246, -286.5823125567796978, -315.6070307612565102 ) ) ;
#90063 = CARTESIAN_POINT ( 'NONE',  ( -101.8094543688281135, -295.6686885890848089, -229.3426470773057417 ) ) ;
#90065 = CARTESIAN_POINT ( 'NONE',  ( 36.06294326259726546, -295.5605663584228751, -281.7697388787118484 ) ) ;
#90066 = CARTESIAN_POINT ( 'NONE',  ( 22.38261756572735806, -288.2716847834572036, -227.4472063587725472 ) ) ;
#90067 = ORIENTED_EDGE ( 'NONE', *, *, #10809, .T. ) ;
#90068 = CARTESIAN_POINT ( 'NONE',  ( 38.09179241347295175, -294.3148378761175081, -256.1270596544019327 ) ) ;
#90069 = CARTESIAN_POINT ( 'NONE',  ( -108.0898192706969496, -285.2850792517341461, -252.1212693096084934 ) ) ;
#90070 = CARTESIAN_POINT ( 'NONE',  ( -109.9741202492437537, -295.0389716840304573, -294.7032679612080415 ) ) ;
#90071 = CARTESIAN_POINT ( 'NONE',  ( -99.08096175945159700, -291.9645896086000221, -224.5960691673709277 ) ) ;
#90072 = CARTESIAN_POINT ( 'NONE',  ( -111.5750778233228715, -291.2985384042939927, -250.0890304602676508 ) ) ;
#90073 = CARTESIAN_POINT ( 'NONE',  ( -108.6622656024757703, -290.5127488894129328, -285.9876803642017649 ) ) ;
#90074 = ORIENTED_EDGE ( 'NONE', *, *, #73934, .T. ) ;
#90075 = DIRECTION ( 'NONE',  ( -1.000000000000000000, -0.000000000000000000, -0.000000000000000000 ) ) ;
#90076 = CARTESIAN_POINT ( 'NONE',  ( -20.86902814125024719, -300.1166924632333917, -194.5911552220985072 ) ) ;
#90077 = CARTESIAN_POINT ( 'NONE',  ( -66.06402550845980670, -272.4794651163252865, -199.3326804433910979 ) ) ;
#90078 = CARTESIAN_POINT ( 'NONE',  ( 34.45899735771880046, -280.8013993939400734, -284.8487499001383298 ) ) ;
#90079 = EDGE_LOOP ( 'NONE', ( #73456, #10162, #18683, #53631 ) ) ;
#90080 = CARTESIAN_POINT ( 'NONE',  ( 35.67354879588813077, -274.7523419694737754, -245.9382336360603460 ) ) ;
#90081 = CARTESIAN_POINT ( 'NONE',  ( -109.5680933949462883, -294.8400185573922272, -285.0546890491760337 ) ) ;
#90082 = CARTESIAN_POINT ( 'NONE',  ( -21.36446662396460283, -278.7056433737603811, -342.9094662571563390 ) ) ;
#90083 = CARTESIAN_POINT ( 'NONE',  ( 24.08755217628629097, -273.1214950897380049, -228.6572265365895475 ) ) ;
#90084 = CARTESIAN_POINT ( 'NONE',  ( -109.4385927434285009, -297.9385651161336455, -256.5402513225126881 ) ) ;
#90085 = CARTESIAN_POINT ( 'NONE',  ( -88.35065948004125858, -298.3969179446072530, -217.6374811047282094 ) ) ;
#90086 = DIRECTION ( 'NONE',  ( 0.000000000000000000, 0.000000000000000000, 1.000000000000000000 ) ) ;
#90087 = CARTESIAN_POINT ( 'NONE',  ( -100.8938457658708501, -298.7113467824224244, -228.2949275043332023 ) ) ;
#90088 = CARTESIAN_POINT ( 'NONE',  ( -98.22295295006043148, -271.1755381684280337, -225.8687767058872282 ) ) ;
#90089 = CARTESIAN_POINT ( 'NONE',  ( 30.92061690884715475, -293.8547217613084399, -244.2048808540021128 ) ) ;
#90090 = CARTESIAN_POINT ( 'NONE',  ( -4.554374849586840135, -291.0675422885425405, -204.4656237401924272 ) ) ;
#90091 = DIRECTION ( 'NONE',  ( 0.000000000000000000, -1.000000000000000000, 0.000000000000000000 ) ) ;
#90092 = CARTESIAN_POINT ( 'NONE',  ( 39.56917834748387719, -276.0187144069889200, -268.3010997361222962 ) ) ;
#90093 = CARTESIAN_POINT ( 'NONE',  ( -100.7188197837267580, -273.2164235174000169, -234.0332193051329739 ) ) ;
#90094 = CARTESIAN_POINT ( 'NONE',  ( 36.06928846079339479, -283.3140484478532244, -253.2976408231910739 ) ) ;
#90095 = AXIS2_PLACEMENT_3D ( 'NONE', #12159, #5545, #78897 ) ;
#90096 = CARTESIAN_POINT ( 'NONE',  ( -33.10292009630843069, -281.6846740888414615, -346.7635073191975721 ) ) ;
#90097 = DIRECTION ( 'NONE',  ( 0.000000000000000000, -1.000000000000000000, 0.000000000000000000 ) ) ;
#90098 = CARTESIAN_POINT ( 'NONE',  ( -105.3678443114821590, -283.3882811167611067, -297.4257394242372925 ) ) ;
#90099 = CARTESIAN_POINT ( 'NONE',  ( -63.30328705811949419, -281.3894433031901485, -340.9020594997853664 ) ) ;
#90100 = CARTESIAN_POINT ( 'NONE',  ( 12.13051257253169268, -274.9229138450200480, -324.9084561355986125 ) ) ;
#90101 = CARTESIAN_POINT ( 'NONE',  ( -56.69646648405463907, -281.8029284398158438, -197.8483490588826044 ) ) ;
#90102 = CARTESIAN_POINT ( 'NONE',  ( 208.8931598777758438, 1.060642095945600216, 7.489249145872055813 ) ) ;
#90103 = DIRECTION ( 'NONE',  ( -1.000000000000000000, 0.000000000000000000, 0.000000000000000000 ) ) ;
#90104 = CARTESIAN_POINT ( 'NONE',  ( -89.59924740339535276, -271.7303822857220439, -214.8310865714975364 ) ) ;
#90105 = CARTESIAN_POINT ( 'NONE',  ( -93.81612771484273594, -279.8646018512585556, -319.9662332155795070 ) ) ;
#90106 = DIRECTION ( 'NONE',  ( 0.000000000000000000, 0.000000000000000000, 1.000000000000000000 ) ) ;
#90107 = CARTESIAN_POINT ( 'NONE',  ( -112.9009035535466694, -286.4767408517752756, -270.0133064719049685 ) ) ;
#90108 = VERTEX_POINT ( 'NONE', #70438 ) ;
#90109 = CARTESIAN_POINT ( 'NONE',  ( 199.7648473163311849, 63.23516263141960536, 10.15923027032019021 ) ) ;
#90110 = CARTESIAN_POINT ( 'NONE',  ( -38.08263916034813690, -287.0612442873232908, -345.3700619854940896 ) ) ;
#90111 = CARTESIAN_POINT ( 'NONE',  ( 207.1360844159087549, 30.54655824920636675, 14.49999999999999822 ) ) ;
#90112 = CARTESIAN_POINT ( 'NONE',  ( -92.13113289799510142, -296.0417140836379986, -221.5221114184148519 ) ) ;
#90113 = CARTESIAN_POINT ( 'NONE',  ( -103.9642223943870789, -288.2554163740471154, -303.1071865146585651 ) ) ;
#90114 = CARTESIAN_POINT ( 'NONE',  ( -104.9628119525177112, -256.0684274861638983, -326.9234398911233939 ) ) ;
#90115 = CARTESIAN_POINT ( 'NONE',  ( -104.5719721256332946, -294.1120329261154325, -303.7214697279811162 ) ) ;
#90116 = CARTESIAN_POINT ( 'NONE',  ( 2.396614496387613702, -285.0544049508075659, -205.2183969541654278 ) ) ;
#90117 = CARTESIAN_POINT ( 'NONE',  ( -6.452979259716959959, -282.0648534210299658, -203.3224978476007152 ) ) ;
#90118 = CARTESIAN_POINT ( 'NONE',  ( -70.05446133020546995, -281.7169623758215948, -338.9600048021335965 ) ) ;
#90119 = CARTESIAN_POINT ( 'NONE',  ( -0.9914430039996633415, -288.5555535167002290, -333.7253754827576699 ) ) ;
#90120 = CARTESIAN_POINT ( 'NONE',  ( -106.0710654899730940, -280.3275246294902558, -243.9190744701859046 ) ) ;
#90121 = CARTESIAN_POINT ( 'NONE',  ( 5.008326495467926520, -281.4440702163716423, -210.7031179196456492 ) ) ;
#90122 = EDGE_CURVE ( 'NONE', #13010, #48224, #27808, .T. ) ;
#90123 = CARTESIAN_POINT ( 'NONE',  ( 9.231606064393066191, -290.3964007067284570, -329.6671498845664701 ) ) ;
#90124 = CARTESIAN_POINT ( 'NONE',  ( -114.1602446862054023, -272.9571022064550334, -264.6320451274926882 ) ) ;
#90125 = ORIENTED_EDGE ( 'NONE', *, *, #76676, .F. ) ;
#90126 = CARTESIAN_POINT ( 'NONE',  ( -73.94486433745520060, -273.5800940724460020, -202.5581494274476029 ) ) ;
#90127 = CARTESIAN_POINT ( 'NONE',  ( 24.69450874071718971, -294.9681996804666824, -228.8477997341847754 ) ) ;
#90128 = PLANE ( 'NONE',  #65125 ) ;
#90129 = CARTESIAN_POINT ( 'NONE',  ( 35.78497577281001440, -278.2662352645559167, -287.0191576251351080 ) ) ;
#90130 = EDGE_LOOP ( 'NONE', ( #19576, #67716 ) ) ;
#90131 = CARTESIAN_POINT ( 'NONE',  ( 37.11183059700131537, -273.4196546579663618, -260.0315396234426544 ) ) ;
#90132 = DIRECTION ( 'NONE',  ( -0.000000000000000000, -0.000000000000000000, -1.000000000000000000 ) ) ;
#90133 = CARTESIAN_POINT ( 'NONE',  ( -65.23003479733981180, -296.0937110755624531, -199.3915327245204310 ) ) ;
#90134 = CARTESIAN_POINT ( 'NONE',  ( -32.67625149399010809, -273.4610545259048422, -197.3956698614260574 ) ) ;
#90135 = MANIFOLD_SOLID_BREP ( 'Chamfer2', #5316 ) ;
#90136 = CARTESIAN_POINT ( 'NONE',  ( -105.3503269531424849, -292.4509758920632407, -241.8463026787514423 ) ) ;
#90137 = CARTESIAN_POINT ( 'NONE',  ( 12.61696937742673263, -284.1042407086167714, -324.9697743730834532 ) ) ;
#90138 = CARTESIAN_POINT ( 'NONE',  ( -111.7476824061083391, -292.1965662743479584, -252.9727282709146152 ) ) ;
#90139 = CARTESIAN_POINT ( 'NONE',  ( -97.08901479694810632, -292.5115170597400720, -222.5745438735997936 ) ) ;
#90140 = CARTESIAN_POINT ( 'NONE',  ( 3.814636806671683367, -294.3140373766194671, -330.6533723325371170 ) ) ;
#90141 = CARTESIAN_POINT ( 'NONE',  ( 31.79581338937473944, -289.1710774746628658, -241.1577655107864473 ) ) ;
#90142 = CARTESIAN_POINT ( 'NONE',  ( -4.161912957332621232, -282.7934014040489501, -339.8601504212729196 ) ) ;
#90143 = CARTESIAN_POINT ( 'NONE',  ( -110.2264170385144837, -294.8885843840683378, -250.2398400608089730 ) ) ;
#90144 = CARTESIAN_POINT ( 'NONE',  ( 0.8665143576031041350, -282.3904208385632728, -337.2279194807567251 ) ) ;
#90145 = CARTESIAN_POINT ( 'NONE',  ( 4.067037680883670347, -278.4710852926170332, -332.4671823712152445 ) ) ;
#90146 = EDGE_CURVE ( 'NONE', #79714, #26085, #85518, .T. ) ;
#90147 = CARTESIAN_POINT ( 'NONE',  ( -6.941161984400275209, -285.1233781216987495, -333.4151289067050357 ) ) ;
#90148 = B_SPLINE_CURVE_WITH_KNOTS ( 'NONE', 3,
 ( #20362, #50639, #444, #6152, #28401, #27944 ),
 .UNSPECIFIED., .F., .F.,
 ( 4, 2, 4 ),
 ( 0.000000000000000000, 0.0004262108901887199383, 0.0008524217803774398767 ),
 .UNSPECIFIED. ) ;
#90149 = CARTESIAN_POINT ( 'NONE',  ( -106.4591617536603252, -276.2874856991006709, -301.5224302475011200 ) ) ;
#90150 = CARTESIAN_POINT ( 'NONE',  ( 152.4536156746142410, 275.5000000000000568, 14.50000000000000000 ) ) ;
#90151 = CARTESIAN_POINT ( 'NONE',  ( -37.54698722155948332, -282.5624774651789153, -343.4348082593910476 ) ) ;
#90152 = CARTESIAN_POINT ( 'NONE',  ( -99.11680002086713159, -280.3621460004630421, -225.0416702303547822 ) ) ;
#90153 = CARTESIAN_POINT ( 'NONE',  ( 39.11202683624916432, -286.6974951852448044, -277.2638598844710032 ) ) ;
#90154 = CARTESIAN_POINT ( 'NONE',  ( -55.27934195559270592, -293.5783764819179282, -198.5543284943716174 ) ) ;
#90155 = CARTESIAN_POINT ( 'NONE',  ( 6.755258838090697715, -276.2406654620227755, -208.1521992418941807 ) ) ;
#90156 = CARTESIAN_POINT ( 'NONE',  ( 31.41946182506521268, -277.3021462103484396, -304.0258547448161153 ) ) ;
#90157 = CARTESIAN_POINT ( 'NONE',  ( -94.45436295300844165, -277.7431814912611685, -315.8469381730821510 ) ) ;
#90158 = CARTESIAN_POINT ( 'NONE',  ( 98.54881674486404108, -301.7573013711235035, -195.4813331363455120 ) ) ;
#90159 = CARTESIAN_POINT ( 'NONE',  ( -35.87256191074403233, -284.0704663282263596, -195.5422028401620196 ) ) ;
#90160 = CARTESIAN_POINT ( 'NONE',  ( 29.45939891080023898, -292.7217262870388481, -232.1072625082411491 ) ) ;
#90161 = CARTESIAN_POINT ( 'NONE',  ( -109.1051765401954583, -291.8237004611193015, -296.1385909104058669 ) ) ;
#90162 = CARTESIAN_POINT ( 'NONE',  ( -44.31598193566112087, -290.8823355036425369, -197.3334762996184963 ) ) ;
#90163 = ORIENTED_EDGE ( 'NONE', *, *, #29603, .F. ) ;
#90164 = CARTESIAN_POINT ( 'NONE',  ( -16.76768863807515331, -290.8875847654112476, -196.7722849802970302 ) ) ;
#90165 = CARTESIAN_POINT ( 'NONE',  ( -17.42275272762526583, -291.9829429016224935, -200.0566551615702906 ) ) ;
#90166 = VERTEX_POINT ( 'NONE', #64744 ) ;
#90167 = CARTESIAN_POINT ( 'NONE',  ( -75.49790889335865529, -290.6284404359536779, -336.8862729430172749 ) ) ;
#90168 = CARTESIAN_POINT ( 'NONE',  ( -110.4939043938701104, -279.1998073312115025, -270.6467192223136067 ) ) ;
#90169 = CARTESIAN_POINT ( 'NONE',  ( -93.42726370851575268, -296.1891288855873086, -217.9778211481304879 ) ) ;
#90170 = CARTESIAN_POINT ( 'NONE',  ( -67.15720418183705931, -286.3227829624628384, -199.4784790307031130 ) ) ;
#90171 = CARTESIAN_POINT ( 'NONE',  ( 39.58341944732033113, -287.9361783288266565, -274.4175880791987652 ) ) ;
#90172 = CARTESIAN_POINT ( 'NONE',  ( -108.3870707587850291, -285.1085875285713769, -253.4358932869931778 ) ) ;
#90173 = CARTESIAN_POINT ( 'NONE',  ( -31.41437309758456919, -124.1952521004627670, -364.2598719284257527 ) ) ;
#90174 = CARTESIAN_POINT ( 'NONE',  ( 187.7861472146279311, 270.9134355758718584, -138.7283278565937508 ) ) ;
#90175 = CARTESIAN_POINT ( 'NONE',  ( 83.88734089079683542, 81.93120406021242275, -298.7933839319709364 ) ) ;
#90176 = CARTESIAN_POINT ( 'NONE',  ( -56.65261662564040535, -276.5045677411774818, -340.9806545945097582 ) ) ;
#90177 = CARTESIAN_POINT ( 'NONE',  ( 35.14937760062440475, -274.3279059302714131, -259.3554836774226260 ) ) ;
#90178 = CARTESIAN_POINT ( 'NONE',  ( -99.86787969626108463, -296.6543971366326105, -225.5280523731308335 ) ) ;
#90179 = CARTESIAN_POINT ( 'NONE',  ( 203.7387371057621976, 292.1034155335181595, -68.30586525936504927 ) ) ;
#90180 = CARTESIAN_POINT ( 'NONE',  ( -39.96293960670030287, -275.7692390514889667, -346.8360344649427702 ) ) ;
#90181 = CARTESIAN_POINT ( 'NONE',  ( -100.1521190306095974, -274.8452414421937533, -231.2098052351783508 ) ) ;
#90182 = ORIENTED_EDGE ( 'NONE', *, *, #92757, .F. ) ;
#90183 = CARTESIAN_POINT ( 'NONE',  ( -109.4788638772821940, -290.8907649120752694, -282.0250181196129233 ) ) ;
#90184 = CARTESIAN_POINT ( 'NONE',  ( -87.36490513066451058, -298.1782784623947009, -211.9656929289267850 ) ) ;
#90185 = CARTESIAN_POINT ( 'NONE',  ( -113.7144538629193846, -297.1610611753389435, -261.0482564390395623 ) ) ;
#90186 = CARTESIAN_POINT ( 'NONE',  ( 21.32773324413360072, -294.3278788925558160, -313.7995524882792324 ) ) ;
#90187 = VERTEX_POINT ( 'NONE', #28728 ) ;
#90188 = CARTESIAN_POINT ( 'NONE',  ( -95.92217566525884820, -279.8194266966205532, -318.1060205293470062 ) ) ;
#90189 = CARTESIAN_POINT ( 'NONE',  ( 33.50680871513438319, -281.4434666549176995, -300.4974095092120479 ) ) ;
#90190 = CARTESIAN_POINT ( 'NONE',  ( -24.27588793701781000, -277.8226245302699908, -342.4730785326017894 ) ) ;
#90191 = CARTESIAN_POINT ( 'NONE',  ( 20.06954850271101165, -277.9940718067817897, -320.1595542729565977 ) ) ;
#90192 = CARTESIAN_POINT ( 'NONE',  ( -106.9550501378554799, -271.3505882487010581, -246.1807695084043530 ) ) ;
#90193 = CARTESIAN_POINT ( 'NONE',  ( 151.4851178187871312, 20.00000000000000000, -3.492110388858667314 ) ) ;
#90194 = CARTESIAN_POINT ( 'NONE',  ( -72.84014796095637223, -277.7030459553524224, -334.1631175055009066 ) ) ;
#90195 = CARTESIAN_POINT ( 'NONE',  ( -32.70258911654635625, -274.9120186768099074, -193.6496411329764555 ) ) ;
#90196 = CARTESIAN_POINT ( 'NONE',  ( -15.11164831457424107, -287.4550957492417638, -343.6225398705749967 ) ) ;
#90197 = CARTESIAN_POINT ( 'NONE',  ( -77.78506792377260126, -275.5091014192090597, -207.1999380638553703 ) ) ;
#90198 = DIRECTION ( 'NONE',  ( 0.000000000000000000, 0.000000000000000000, 1.000000000000000000 ) ) ;
#90199 = CARTESIAN_POINT ( 'NONE',  ( -15.81387265384110918, -287.9637265144304479, -340.3365456402897280 ) ) ;
#90200 = CARTESIAN_POINT ( 'NONE',  ( -109.2106551898552027, -283.5523808708134652, -297.8621645647637592 ) ) ;
#90201 = CARTESIAN_POINT ( 'NONE',  ( 27.73553469996999610, -280.2664762417829820, -305.6162951674692749 ) ) ;
#90203 = CARTESIAN_POINT ( 'NONE',  ( -52.35594776973218245, -283.9382260207681838, -197.4509913697332593 ) ) ;
#90202 = CARTESIAN_POINT ( 'NONE',  ( 24.18507444310836974, -279.5705762980783220, -229.8980252222388856 ) ) ;
#90204 = CARTESIAN_POINT ( 'NONE',  ( -79.64505473336781449, -291.6235539402017594, -332.3540981352957715 ) ) ;
#90205 = CARTESIAN_POINT ( 'NONE',  ( -89.76789227409565797, -280.4973907152653965, -218.9215265224820541 ) ) ;
#90206 = CARTESIAN_POINT ( 'NONE',  ( 153.6987871352710613, 19.48326534539920019, -11.45812909362551757 ) ) ;
#90207 = CARTESIAN_POINT ( 'NONE',  ( 38.47990406833412891, -280.0543012940727863, -278.4540283201876605 ) ) ;
#90208 = CARTESIAN_POINT ( 'NONE',  ( -33.66360306652134682, -294.0986121181003341, -195.4513572526384735 ) ) ;
#90209 = CARTESIAN_POINT ( 'NONE',  ( -98.59751601564781254, -277.3974082529711609, -225.3758587141356031 ) ) ;
#90210 = CARTESIAN_POINT ( 'NONE',  ( -41.85460081388423248, -277.7618990135222248, -343.3362319250621226 ) ) ;
#90211 = CARTESIAN_POINT ( 'NONE',  ( -107.5804948036154656, -286.2035275333274171, -297.2742918177161187 ) ) ;
#90212 = DIRECTION ( 'NONE',  ( 0.9951408606192336803, 0.000000000000000000, -0.09846150276128748380 ) ) ;
#90213 = CARTESIAN_POINT ( 'NONE',  ( -112.9489458325655136, -292.4611462319977591, -271.2369360244861696 ) ) ;
#90214 = CARTESIAN_POINT ( 'NONE',  ( 38.92898483075529725, -286.8715371414518813, -280.1128547203847461 ) ) ;
#90215 = CARTESIAN_POINT ( 'NONE',  ( -41.61905078916150558, -290.3973912909737010, -196.6347808735201852 ) ) ;
#90216 = CARTESIAN_POINT ( 'NONE',  ( -48.18343439338967471, -273.4767344845260482, -432.0952024610487001 ) ) ;
#90217 = CARTESIAN_POINT ( 'NONE',  ( 32.53589558288029338, -273.9349542496498771, -247.4296587769936195 ) ) ;
#90218 = CARTESIAN_POINT ( 'NONE',  ( 23.93947580448152124, -292.2661274993499774, -312.3494546677990797 ) ) ;
#90219 = CARTESIAN_POINT ( 'NONE',  ( 73.43068321062709458, -134.2391364535880598, 4.999999999999990230 ) ) ;
#90220 = CARTESIAN_POINT ( 'NONE',  ( 37.64750106673213281, -291.8538617524871484, -256.2427803231421990 ) ) ;
#90221 = CARTESIAN_POINT ( 'NONE',  ( -102.9588975220734852, -286.6064475842487695, -236.5850344434279862 ) ) ;
#90222 = CARTESIAN_POINT ( 'NONE',  ( -20.73992347687352833, -287.0818639099150005, -344.5659556676834541 ) ) ;
#90223 = CARTESIAN_POINT ( 'NONE',  ( 33.22992185544049448, -288.7031185475520942, -249.4595447327372995 ) ) ;
#90224 = DIRECTION ( 'NONE',  ( -0.000000000000000000, -1.000000000000000000, -9.656854691831248164E-17 ) ) ;
#90225 = CARTESIAN_POINT ( 'NONE',  ( 32.82193134830651360, -288.0807793293030272, -249.5885461554855738 ) ) ;
#90226 = EDGE_CURVE ( 'NONE', #47196, #64985, #62903, .T. ) ;
#90227 = CARTESIAN_POINT ( 'NONE',  ( 38.01029806876059780, -295.4951506261967893, -267.4739222729283483 ) ) ;
#90228 = CARTESIAN_POINT ( 'NONE',  ( -112.6462317283272938, -276.5451384234661987, -277.1764000091938556 ) ) ;
#90229 = CARTESIAN_POINT ( 'NONE',  ( -74.08302051657516074, -277.8599109470321196, -338.0209206272429583 ) ) ;
#90230 = CARTESIAN_POINT ( 'NONE',  ( 22.84335777169875925, -291.0114167651252615, -224.6553238796714140 ) ) ;
#90231 = CARTESIAN_POINT ( 'NONE',  ( -86.80472195717005945, -279.3863449120256064, -211.2796780886763770 ) ) ;
#90232 = CARTESIAN_POINT ( 'NONE',  ( -37.85865255701175869, -300.0255354181899179, -195.7181037938501333 ) ) ;
#90233 = CARTESIAN_POINT ( 'NONE',  ( -48.18343439339133027, -275.3442733027022200, -501.6452696258747324 ) ) ;
#90234 = CARTESIAN_POINT ( 'NONE',  ( -110.6810105371885982, -282.3496828225431159, -286.1176294838675176 ) ) ;
#90235 = CARTESIAN_POINT ( 'NONE',  ( -48.18343439339132317, -275.3442733027010831, -501.6452696257773596 ) ) ;
#90236 = CARTESIAN_POINT ( 'NONE',  ( -111.1924004894778051, -276.7959876254700475, -262.3241402486000879 ) ) ;
#90237 = CARTESIAN_POINT ( 'NONE',  ( 36.03345623882090365, -279.3518397112863454, -254.7726022256022134 ) ) ;
#90238 = CYLINDRICAL_SURFACE ( 'NONE', #89510, 0.5000000000000004441 ) ;
#90239 = CARTESIAN_POINT ( 'NONE',  ( -73.78293023564260977, -276.0068072159758117, -337.4188423444060163 ) ) ;
#90240 = CARTESIAN_POINT ( 'NONE',  ( -70.01421983127275439, -297.0107569983521785, -336.4157484848395825 ) ) ;
#90241 = CARTESIAN_POINT ( 'NONE',  ( -21.80210880432005993, -281.7778021113119280, -345.4611420196619065 ) ) ;
#90242 = CARTESIAN_POINT ( 'NONE',  ( -107.8260178613610947, -297.2314009983613801, -290.2450160460394954 ) ) ;
#90243 = CARTESIAN_POINT ( 'NONE',  ( -62.69749977286563336, -299.0440613989799203, -198.1781442523023031 ) ) ;
#90244 = CARTESIAN_POINT ( 'NONE',  ( -16.63060276863775755, -273.9938007425339492, -200.2859830649728679 ) ) ;
#90245 = CARTESIAN_POINT ( 'NONE',  ( -0.2902045951222534947, -294.5449658596472204, -205.1374507274707639 ) ) ;
#90246 = CARTESIAN_POINT ( 'NONE',  ( 38.28978479963161874, -287.5380813172204739, -255.9084887355259070 ) ) ;
#90247 = CARTESIAN_POINT ( 'NONE',  ( 5.158502412749834676, -274.6235960332911077, -333.0830301226208690 ) ) ;
#90248 = CARTESIAN_POINT ( 'NONE',  ( -62.76565589592060235, -289.2073230599058888, -343.0991544958789632 ) ) ;
#90249 = EDGE_CURVE ( 'NONE', #30132, #19742, #41510, .T. ) ;
#90250 = CARTESIAN_POINT ( 'NONE',  ( 25.89318396655322729, -287.1175450148280675, -307.4039760413180602 ) ) ;
#90251 = CARTESIAN_POINT ( 'NONE',  ( -101.4916234322722772, -289.0738365933872842, -231.4050520080278943 ) ) ;
#90252 = ORIENTED_EDGE ( 'NONE', *, *, #73796, .T. ) ;
#90253 = CARTESIAN_POINT ( 'NONE',  ( 68.56402772857219929, 46.98157435473511612, -321.4867780223927980 ) ) ;
#90254 = CARTESIAN_POINT ( 'NONE',  ( -66.35923439008259095, -288.9501479939425508, -337.4671855449669238 ) ) ;
#90255 = CYLINDRICAL_SURFACE ( 'NONE', #27822, 0.5000000000000004441 ) ;
#90256 = CARTESIAN_POINT ( 'NONE',  ( -97.40381903799490715, -286.1353716648494583, -222.5556571405401485 ) ) ;
#90257 = CARTESIAN_POINT ( 'NONE',  ( -39.19396321485209711, -291.0882250066502479, -193.6057655870010592 ) ) ;
#90258 = CARTESIAN_POINT ( 'NONE',  ( 14.60095078737550978, -282.3684854302027816, -214.5359661306991370 ) ) ;
#90259 = CARTESIAN_POINT ( 'NONE',  ( -48.06632584490038340, -281.2337519709469120, -194.5561768831846621 ) ) ;
#90260 = CARTESIAN_POINT ( 'NONE',  ( -38.88720806377160244, -282.9053596033864437, -343.3572467925595220 ) ) ;
#90261 = CARTESIAN_POINT ( 'NONE',  ( -68.85521594082125318, -279.4665886444153671, -338.4332954252337231 ) ) ;
#90262 = CARTESIAN_POINT ( 'NONE',  ( -113.1391160217790457, -296.7216824773335020, -256.8056119485592603 ) ) ;
#90263 = CARTESIAN_POINT ( 'NONE',  ( -94.17031542830721946, -274.5232084580507603, -223.7393757060845871 ) ) ;
#90264 = CARTESIAN_POINT ( 'NONE',  ( -14.31559698186996421, -290.3723170832461733, -199.3565732352207647 ) ) ;
#90265 = CARTESIAN_POINT ( 'NONE',  ( -104.7382635720461934, -271.7370843226956936, -241.1663573600054065 ) ) ;
#90266 = VERTEX_POINT ( 'NONE', #1695 ) ;
#90267 = CARTESIAN_POINT ( 'NONE',  ( -95.39291326371389346, -285.8262890322477574, -316.9793568464417604 ) ) ;
#90268 = CARTESIAN_POINT ( 'NONE',  ( 22.05599015673160679, -295.2857992579992015, -318.8936639282692340 ) ) ;
#90269 = CARTESIAN_POINT ( 'NONE',  ( -81.54679794574521168, -286.0836324178754921, -212.1391118786113168 ) ) ;
#90270 = CARTESIAN_POINT ( 'NONE',  ( 3.366532553764151281, -275.5783129631894894, -335.5056328408796276 ) ) ;
#90271 = CARTESIAN_POINT ( 'NONE',  ( -84.21079868002868807, -292.0783456313117199, -209.3300742823917631 ) ) ;
#90272 = CARTESIAN_POINT ( 'NONE',  ( -102.9586576800951008, -283.1933971071168799, -232.3791388229669792 ) ) ;
#90273 = CARTESIAN_POINT ( 'NONE',  ( -34.96531909373578628, -292.4144799636879952, -193.4058042189810749 ) ) ;
#90274 = CARTESIAN_POINT ( 'NONE',  ( -39.95452290089063041, -289.4190355840145230, -343.3850933968739696 ) ) ;
#90275 = DIRECTION ( 'NONE',  ( 0.000000000000000000, 0.000000000000000000, -1.000000000000000000 ) ) ;
#90276 = DIRECTION ( 'NONE',  ( -0.000000000000000000, 1.000000000000000000, -0.000000000000000000 ) ) ;
#90277 = CARTESIAN_POINT ( 'NONE',  ( -110.8433564205054438, -271.0408464140099909, -283.6640628832823268 ) ) ;
#90278 = CARTESIAN_POINT ( 'NONE',  ( -78.16799930467063007, -287.0338436876424453, -205.8946844890710111 ) ) ;
#90279 = CARTESIAN_POINT ( 'NONE',  ( 40.65961533371913106, -272.8380690714490129, -252.5904736702033802 ) ) ;
#90280 = VERTEX_POINT ( 'NONE', #22090 ) ;
#90281 = CARTESIAN_POINT ( 'NONE',  ( 21.58561121256696680, -279.8633862053048915, -226.7303755778752645 ) ) ;
#90282 = CARTESIAN_POINT ( 'NONE',  ( -1.481342910053283335, -276.2565674700657041, -338.4770417580498361 ) ) ;
#90283 = CARTESIAN_POINT ( 'NONE',  ( -97.90403835941212662, -281.1523823480698638, -226.4039613800688642 ) ) ;
#90284 = CARTESIAN_POINT ( 'NONE',  ( -10.82389337143313135, -93.05637620313754610, -358.2402470118966562 ) ) ;
#90285 = CARTESIAN_POINT ( 'NONE',  ( -78.85494278081915809, -282.1747055079428605, -334.5113866990816973 ) ) ;
#90286 = CARTESIAN_POINT ( 'NONE',  ( -60.46473692186032878, -283.7708841519874454, -199.3880810574634950 ) ) ;
#90287 = CARTESIAN_POINT ( 'NONE',  ( -33.42247641351010401, -299.8607127602575133, -194.3732890516851910 ) ) ;
#90288 = CARTESIAN_POINT ( 'NONE',  ( -77.97876766186865893, -296.1066482066365779, -331.1397416483043799 ) ) ;
#90289 = VERTEX_POINT ( 'NONE', #23483 ) ;
#90290 = CARTESIAN_POINT ( 'NONE',  ( 27.93216489230453448, -291.7807978776816640, -236.5888509290503237 ) ) ;
#90291 = CARTESIAN_POINT ( 'NONE',  ( 23.44257852655138308, -276.8335429644004080, -317.4843262545308562 ) ) ;
#90292 = CARTESIAN_POINT ( 'NONE',  ( 34.12134524492419985, -275.3547811567860890, -255.3993167324521494 ) ) ;
#90293 = CARTESIAN_POINT ( 'NONE',  ( 17.87662385336003013, -273.7401728499644378, -217.0642995870800291 ) ) ;
#90294 = DIRECTION ( 'NONE',  ( -0.3994899938747922263, 0.000000000000000000, 0.9167375550253837879 ) ) ;
#90295 = CARTESIAN_POINT ( 'NONE',  ( 9.741099533415315648, -272.6996006410201971, -211.9152923815999543 ) ) ;
#90296 = CARTESIAN_POINT ( 'NONE',  ( -0.9705319950128667994, -296.0043371559549996, -337.5751797897855795 ) ) ;
#90297 = CARTESIAN_POINT ( 'NONE',  ( 189.9243309297870610, 275.5000000000000568, 24.72542485937349710 ) ) ;
#90298 = CARTESIAN_POINT ( 'NONE',  ( 197.8536156918358131, 70.38469146216345962, 8.282373351508748982 ) ) ;
#90299 = CARTESIAN_POINT ( 'NONE',  ( -1.087228655259989685, -283.6384841326533319, -334.0779868018282741 ) ) ;
#90300 = CARTESIAN_POINT ( 'NONE',  ( 36.68514615086283470, -283.0943330725252167, -253.1575948953936859 ) ) ;
#90301 = CARTESIAN_POINT ( 'NONE',  ( -101.0761317332694205, -284.3911811793102515, -234.4549573645665816 ) ) ;
#90302 = CARTESIAN_POINT ( 'NONE',  ( -59.45389679821642659, -275.7431620975099804, -340.7705716957821096 ) ) ;
#90303 = CARTESIAN_POINT ( 'NONE',  ( -34.78059007177041906, -284.8800885926299316, -344.5647762741884321 ) ) ;
#90304 = CARTESIAN_POINT ( 'NONE',  ( -110.1802725726846148, -276.8857796841296590, -281.5526378572948261 ) ) ;
#90305 = CARTESIAN_POINT ( 'NONE',  ( 222.8344101925596306, -44.55766379199612004, -21.49999999999998579 ) ) ;
#90306 = CARTESIAN_POINT ( 'NONE',  ( -114.2231699715874953, -279.3392566174510989, -271.6159845739180696 ) ) ;
#90307 = VERTEX_POINT ( 'NONE', #86938 ) ;
#90308 = CARTESIAN_POINT ( 'NONE',  ( 198.8856906601484980, 17.32477107587147458, 10.54429824094339097 ) ) ;
#90309 = CARTESIAN_POINT ( 'NONE',  ( -93.02823615882769559, -287.1240718687753315, -218.9099358403580027 ) ) ;
#90310 = EDGE_CURVE ( 'NONE', #10071, #4825, #68901, .T. ) ;
#90311 = CARTESIAN_POINT ( 'NONE',  ( -39.70447306423596956, -294.2797126374510981, -343.4968896658414224 ) ) ;
#90312 = CARTESIAN_POINT ( 'NONE',  ( -101.5942191312459641, -290.4579537820420683, -228.0171874096032809 ) ) ;
#90313 = CARTESIAN_POINT ( 'NONE',  ( 34.05350582185366193, -286.0484844918586305, -290.0625849946681001 ) ) ;
#90315 = CARTESIAN_POINT ( 'NONE',  ( -108.3614058151910484, -289.0644404839585491, -249.4792877253562153 ) ) ;
#90314 = CARTESIAN_POINT ( 'NONE',  ( -16.99165617770425385, -284.8946983804767683, -199.5883189499267303 ) ) ;
#90316 = CARTESIAN_POINT ( 'NONE',  ( -66.70440491860692589, -284.6506744658333901, -337.6425996158478711 ) ) ;
#90317 = CARTESIAN_POINT ( 'NONE',  ( 15.52685055953734938, -274.3048549042079571, -323.6305749097360831 ) ) ;
#90318 = CARTESIAN_POINT ( 'NONE',  ( -3.822688026705792996, -284.8868179811015580, -201.9149022078535154 ) ) ;
#90319 = CARTESIAN_POINT ( 'NONE',  ( -3.157811986379429392, -288.5037884096350922, -203.5900097945627465 ) ) ;
#90320 = CARTESIAN_POINT ( 'NONE',  ( 36.23435358872315959, -285.3541356054674907, -254.9171253671933073 ) ) ;
#90321 = CARTESIAN_POINT ( 'NONE',  ( 28.36746431961739034, -282.9315629165246833, -302.8137459536339975 ) ) ;
#90322 = CARTESIAN_POINT ( 'NONE',  ( -41.62988728091504242, -291.1061843201651413, -345.4182782326228107 ) ) ;
#90323 = LINE ( 'NONE', #75671, #21649 ) ;
#90324 = CARTESIAN_POINT ( 'NONE',  ( 196.6930115205277616, 40.98292740024594849, 12.61309341605360856 ) ) ;
#90325 = CARTESIAN_POINT ( 'NONE',  ( -78.66854085205032732, -297.5243033608015253, -333.6177890311099645 ) ) ;
#90326 = CARTESIAN_POINT ( 'NONE',  ( -68.10394727419324568, -277.6480984868964583, -201.9462293040242002 ) ) ;
#90327 = CARTESIAN_POINT ( 'NONE',  ( 13.18000835964080686, -291.9348286519712019, -212.4671131848947994 ) ) ;
#90328 = CARTESIAN_POINT ( 'NONE',  ( -90.60933017775367659, -295.6818859337348613, -219.2096358531310614 ) ) ;
#90329 = CARTESIAN_POINT ( 'NONE',  ( 20.55921766436886955, -280.8707185380458782, -315.6239857483237188 ) ) ;
#90330 = CARTESIAN_POINT ( 'NONE',  ( -31.19693970416748741, -272.2101873814651185, -196.1622624428697179 ) ) ;
#90331 = CARTESIAN_POINT ( 'NONE',  ( 20.08956524221319739, -295.5109225487952926, -316.2384998094022421 ) ) ;
#90332 = PRESENTATION_STYLE_ASSIGNMENT (( #53437 ) ) ;
#90333 = CARTESIAN_POINT ( 'NONE',  ( -111.2436806109478482, -271.3741745718391485, -250.7396404103864995 ) ) ;
#90334 = CARTESIAN_POINT ( 'NONE',  ( -4.955047983882035822, -292.8714688989705905, -339.1146034758447172 ) ) ;
#90335 = CARTESIAN_POINT ( 'NONE',  ( -49.80624549954305991, -293.3154643216282693, -197.7834499110632009 ) ) ;
#90336 = CARTESIAN_POINT ( 'NONE',  ( 125.0516381006429043, 8.053287430127898716, 21.50000000000000000 ) ) ;
#90337 = CARTESIAN_POINT ( 'NONE',  ( 21.46233837268349021, -294.9639285873884091, -313.8891179752441758 ) ) ;
#90338 = DIRECTION ( 'NONE',  ( 0.000000000000000000, 0.000000000000000000, 1.000000000000000000 ) ) ;
#90340 = CARTESIAN_POINT ( 'NONE',  ( -55.80330993922925131, -295.2963975017402163, -341.0404718313893113 ) ) ;
#90339 = CARTESIAN_POINT ( 'NONE',  ( -96.76331142473912905, -281.9396113719575396, -316.7020169601669863 ) ) ;
#90341 = CARTESIAN_POINT ( 'NONE',  ( 34.58750622549786868, -281.9000618070899691, -297.8418252759362304 ) ) ;
#90342 = CARTESIAN_POINT ( 'NONE',  ( -67.87686953301690096, -283.1088642971622562, -341.0247417291120087 ) ) ;
#90343 = CARTESIAN_POINT ( 'NONE',  ( -108.7080324253075787, -288.2588691537977184, -293.0465819194508299 ) ) ;
#90344 = DIRECTION ( 'NONE',  ( -0.000000000000000000, -1.000000000000000000, -0.000000000000000000 ) ) ;
#90345 = CARTESIAN_POINT ( 'NONE',  ( 36.66361052477951432, -279.7972148318758627, -251.7621462369345409 ) ) ;
#90346 = CARTESIAN_POINT ( 'NONE',  ( 27.17727345250740711, -287.0196806989632705, -311.9173560281780055 ) ) ;
#90347 = CARTESIAN_POINT ( 'NONE',  ( -36.97128956651225451, -296.6475354380180534, -344.1727519500162202 ) ) ;
#90348 = CARTESIAN_POINT ( 'NONE',  ( -25.84060616489625062, -278.3336692868807063, -345.9013796268242800 ) ) ;
#90349 = CARTESIAN_POINT ( 'NONE',  ( -30.25611005660749697, -279.8108334134322490, -197.6341914982838830 ) ) ;
#90350 = CARTESIAN_POINT ( 'NONE',  ( -5.888878814159318686, -292.6209827031057671, -200.0636878991154788 ) ) ;
#90351 = CARTESIAN_POINT ( 'NONE',  ( -90.86538316923216030, -283.3796230072475169, -217.0269867841931841 ) ) ;
#90352 = CARTESIAN_POINT ( 'NONE',  ( -66.89641061907894937, -279.4396156094911703, -339.2923862049638046 ) ) ;
#90353 = CARTESIAN_POINT ( 'NONE',  ( 35.87667263266076390, -292.6523132273595138, -273.5110069074565331 ) ) ;
#90354 = CARTESIAN_POINT ( 'NONE',  ( -102.1094738061161422, -295.0584019353717053, -232.4416868310134703 ) ) ;
#90355 = ORIENTED_EDGE ( 'NONE', *, *, #87037, .T. ) ;
#90356 = CARTESIAN_POINT ( 'NONE',  ( 197.2116943569230330, 275.0000000000000568, -12.92446933126074882 ) ) ;
#90357 = CARTESIAN_POINT ( 'NONE',  ( -12.99364014805401624, -294.2348347125465011, -339.2995436961770110 ) ) ;
#90358 = DIRECTION ( 'NONE',  ( -1.000000000000000000, 0.000000000000000000, 0.000000000000000000 ) ) ;
#90359 = CARTESIAN_POINT ( 'NONE',  ( -82.08285599513421005, -282.9094976428776249, -214.2051214447836571 ) ) ;
#90360 = CARTESIAN_POINT ( 'NONE',  ( -109.0122795034231871, -272.1026371911677870, -242.5111566755481647 ) ) ;
#90361 = CARTESIAN_POINT ( 'NONE',  ( 35.79890992453862708, -279.4395897272321463, -250.5442946994076863 ) ) ;
#90362 = CARTESIAN_POINT ( 'NONE',  ( 21.69885967798633430, -288.2093361042900028, -221.7040468376499405 ) ) ;
#90363 = CARTESIAN_POINT ( 'NONE',  ( -75.87054129358756427, -289.4157248156358833, -332.3653791501772048 ) ) ;
#90364 = CARTESIAN_POINT ( 'NONE',  ( -69.53700670080370116, -279.0038616006360712, -336.6636209178132049 ) ) ;
#90365 = CARTESIAN_POINT ( 'NONE',  ( -73.35934398949902402, -299.3275775620223271, -205.7027593182978364 ) ) ;
#90366 = ADVANCED_FACE ( 'NONE', ( #87852, #65205 ), #1238, .T. ) ;
#90367 = CARTESIAN_POINT ( 'NONE',  ( -45.96992635546732942, -275.9587742842610965, -343.3001819554278882 ) ) ;
#90368 = ORIENTED_EDGE ( 'NONE', *, *, #26658, .F. ) ;
#90369 = CARTESIAN_POINT ( 'NONE',  ( -29.05819509579903936, -297.8199280375310423, -193.3827149222969126 ) ) ;
#90370 = CARTESIAN_POINT ( 'NONE',  ( -111.7444087704486861, -292.4251952944334221, -274.0033251148691420 ) ) ;
#90371 = CARTESIAN_POINT ( 'NONE',  ( 0.1646776635978103864, -296.1616022925646234, -336.7064670191150526 ) ) ;
#90372 = CARTESIAN_POINT ( 'NONE',  ( 113.5000000000000568, -298.0521521680024080, -540.3336712212508246 ) ) ;
#90373 = EDGE_CURVE ( 'NONE', #20997, #71446, #44685, .T. ) ;
#90374 = CARTESIAN_POINT ( 'NONE',  ( -91.75457245208659174, -291.9014077840197388, -221.5250595760859653 ) ) ;
#90375 = CARTESIAN_POINT ( 'NONE',  ( -43.51953433940560956, -250.4898501243895055, -452.7628537496786407 ) ) ;
#90376 = CARTESIAN_POINT ( 'NONE',  ( -30.78024186626734249, -290.2737031250564996, -194.8290579847819401 ) ) ;
#90377 = CARTESIAN_POINT ( 'NONE',  ( -34.05234342206758669, -298.4255600716530807, -193.3820815229926495 ) ) ;
#90378 = CARTESIAN_POINT ( 'NONE',  ( -107.6243128501388071, -295.9570737400011353, -290.1712627519395369 ) ) ;
#90379 = CARTESIAN_POINT ( 'NONE',  ( 200.1145890159574492, 64.93834475843401322, -5.212391550061756362 ) ) ;
#90380 = CARTESIAN_POINT ( 'NONE',  ( 195.8444066023239714, 25.85623389517961002, 14.49918517833957132 ) ) ;
#90381 = CARTESIAN_POINT ( 'NONE',  ( -80.13562550161836384, -291.1397549930306923, -333.6023700536939032 ) ) ;
#90382 = CARTESIAN_POINT ( 'NONE',  ( 40.64545035920995986, -289.8376638359844719, -252.5284128619064461 ) ) ;
#90383 = CARTESIAN_POINT ( 'NONE',  ( -102.6023083257882860, -287.0423280101258570, -233.6340795789281231 ) ) ;
#90384 = CARTESIAN_POINT ( 'NONE',  ( -24.25130737657040569, -272.2193692844222710, -196.6287218267999890 ) ) ;
#90385 = CARTESIAN_POINT ( 'NONE',  ( -79.69405811200000755, -275.3953687301681725, -209.0809121852981320 ) ) ;
#90386 = CARTESIAN_POINT ( 'NONE',  ( -1.729442012136990448, -290.6076750210952468, -204.9778309715839271 ) ) ;
#90387 = CARTESIAN_POINT ( 'NONE',  ( -81.80199211890199251, -279.5110740460269767, -331.7092060873821424 ) ) ;
#90388 = CARTESIAN_POINT ( 'NONE',  ( 26.94074944044356101, -281.3750257754271047, -305.1700154851422440 ) ) ;
#90389 = CARTESIAN_POINT ( 'NONE',  ( -106.0622624743833171, -279.1911556051008461, -304.5243044831680663 ) ) ;
#90390 = CARTESIAN_POINT ( 'NONE',  ( -31.09077634398100543, -278.9242592134537517, -193.9612389027497557 ) ) ;
#90391 = CARTESIAN_POINT ( 'NONE',  ( 119.9890085633751937, 148.7358962376707439, -260.8480417884134113 ) ) ;
#90392 = CARTESIAN_POINT ( 'NONE',  ( 39.08184792331802271, -276.3959431867834269, -262.5922020079913750 ) ) ;
#90393 = CARTESIAN_POINT ( 'NONE',  ( -78.48416444828940541, -275.0291402594331203, -206.0960000615810372 ) ) ;
#90394 = CARTESIAN_POINT ( 'NONE',  ( -37.30987171927208124, -297.5519495502701943, -345.3611179825600175 ) ) ;
#90395 = ORIENTED_EDGE ( 'NONE', *, *, #51306, .F. ) ;
#90396 = AXIS2_PLACEMENT_3D ( 'NONE', #11438, #90937, #33211 ) ;
#90397 = FACE_OUTER_BOUND ( 'NONE', #15109, .T. ) ;
#90398 = CARTESIAN_POINT ( 'NONE',  ( -29.12488192841018986, -290.0252483340416916, -343.2082865755819512 ) ) ;
#90399 = CARTESIAN_POINT ( 'NONE',  ( 38.59288139358631042, -289.3628087000748792, -274.3471321351187271 ) ) ;
#90400 = CARTESIAN_POINT ( 'NONE',  ( -63.86560607265932532, -288.7558257394470047, -338.5356800184054009 ) ) ;
#90401 = CARTESIAN_POINT ( 'NONE',  ( -33.72394485042956802, -285.6041901037870616, -193.5077592394279691 ) ) ;
#90402 = CARTESIAN_POINT ( 'NONE',  ( 201.2104617360081704, 25.32700003806617772, 9.000000000000000000 ) ) ;
#90403 = CARTESIAN_POINT ( 'NONE',  ( 34.54422362365561838, -279.7341205553152577, -253.6621843615318710 ) ) ;
#90404 = CARTESIAN_POINT ( 'NONE',  ( 4.327205072108847972, -290.3445182259978310, -331.8606263311714315 ) ) ;
#90405 = CARTESIAN_POINT ( 'NONE',  ( 3.761029688458136011, -280.9680863860985482, -331.5887828602889726 ) ) ;
#90406 = CARTESIAN_POINT ( 'NONE',  ( -105.9808377428451536, -280.2174440780810301, -243.9523122969912947 ) ) ;
#90407 = CARTESIAN_POINT ( 'NONE',  ( -71.67756389271399087, -278.0110926378047225, -334.8658244490279685 ) ) ;
#90408 = CARTESIAN_POINT ( 'NONE',  ( -90.49928961750495660, -290.1146560998924997, -215.1306523232821348 ) ) ;
#90409 = CARTESIAN_POINT ( 'NONE',  ( -111.3332120467901376, -285.0947679566928628, -291.0834485645143559 ) ) ;
#90410 = CARTESIAN_POINT ( 'NONE',  ( -46.50439295085475067, -286.4311645642620761, -193.9702025320064820 ) ) ;
#90411 = CARTESIAN_POINT ( 'NONE',  ( -66.55762340021280465, -283.6124466284776986, -337.2733422451516958 ) ) ;
#90412 = VERTEX_POINT ( 'NONE', #87392 ) ;
#90413 = CARTESIAN_POINT ( 'NONE',  ( 82.64890176555634582, -299.5541904835138780, -197.7570935515976203 ) ) ;
#90414 = CARTESIAN_POINT ( 'NONE',  ( -110.3453433170029712, -292.1544968999503453, -290.6286674967419117 ) ) ;
#90415 = CARTESIAN_POINT ( 'NONE',  ( 29.13780701110361449, -292.7331104276376550, -308.3332980187386738 ) ) ;
#90416 = CARTESIAN_POINT ( 'NONE',  ( 35.82272852617663261, -274.5553545514828784, -266.1373098899807701 ) ) ;
#90417 = CARTESIAN_POINT ( 'NONE',  ( -77.03672865549508231, -294.9175268721442080, -336.2836616551266502 ) ) ;
#90418 = CARTESIAN_POINT ( 'NONE',  ( -108.7758209300875905, -289.2693709503874402, -252.2025557979152950 ) ) ;
#90419 = CARTESIAN_POINT ( 'NONE',  ( -3.898560151428867027, -292.8446945248484781, -336.4020487897673206 ) ) ;
#90420 = CARTESIAN_POINT ( 'NONE',  ( -110.3694930110057442, -291.8537121254119029, -263.0077533798935292 ) ) ;
#90421 = DIRECTION ( 'NONE',  ( -0.000000000000000000, 1.000000000000000000, 0.000000000000000000 ) ) ;
#90422 = CARTESIAN_POINT ( 'NONE',  ( 26.50882205886980003, -291.0193906701816786, -230.5998967255951300 ) ) ;
#90423 = CARTESIAN_POINT ( 'NONE',  ( -85.29585550121535675, -297.7143839599389139, -328.0941810272661883 ) ) ;
#90424 = CARTESIAN_POINT ( 'NONE',  ( 33.25289301502674277, -288.2367111987811086, -250.8723553861403275 ) ) ;
#90425 = ADVANCED_FACE ( 'NONE', ( #50960 ), #30120, .T. ) ;
#90426 = CARTESIAN_POINT ( 'NONE',  ( 36.30370095453862689, -277.7367860560564168, -286.3827532494691468 ) ) ;
#90427 = CARTESIAN_POINT ( 'NONE',  ( -96.75620157317635517, -276.6947032797544352, -318.7337652591716619 ) ) ;
#90428 = CARTESIAN_POINT ( 'NONE',  ( -14.85853804091576791, -297.5240962728179284, -193.5255645770875788 ) ) ;
#90429 = CARTESIAN_POINT ( 'NONE',  ( 31.20820741809435006, -274.1623476043325809, -298.4058836241657104 ) ) ;
#90430 = CARTESIAN_POINT ( 'NONE',  ( -52.08918302576198300, -277.9418988163803874, -197.3438173247801046 ) ) ;
#90431 = CARTESIAN_POINT ( 'NONE',  ( 11.80105736291380225, -275.9576610621847976, -215.7755448104324785 ) ) ;
#90432 = CARTESIAN_POINT ( 'NONE',  ( -14.84552422774434000, -275.1654575875252249, -343.2199471010634966 ) ) ;
#90433 = DIRECTION ( 'NONE',  ( 0.000000000000000000, 1.000000000000000000, 0.000000000000000000 ) ) ;
#90434 = CARTESIAN_POINT ( 'NONE',  ( -52.67889550529869780, -298.6535656316958693, -198.7733060897125767 ) ) ;
#90435 = DIRECTION ( 'NONE',  ( 0.000000000000000000, -1.000000000000000000, 0.000000000000000000 ) ) ;
#90437 = CARTESIAN_POINT ( 'NONE',  ( -54.20947691318854567, -273.6627369625291522, -199.3366284679518117 ) ) ;
#90436 = CARTESIAN_POINT ( 'NONE',  ( -5.061026023153183395, -286.6494641961273828, -338.4661430223707157 ) ) ;
#90438 = CARTESIAN_POINT ( 'NONE',  ( 39.70246838695052105, -287.5670368962058205, -271.5512887772176782 ) ) ;
#90439 = CARTESIAN_POINT ( 'NONE',  ( -14.96245253393503916, -288.4368304901600482, -344.0708654539153599 ) ) ;
#90440 = CARTESIAN_POINT ( 'NONE',  ( -107.4656973267147180, -274.9051788809576351, -243.1501452168379558 ) ) ;
#90441 = CARTESIAN_POINT ( 'NONE',  ( -110.2578004204040525, -294.7685807993274807, -253.5304688717324098 ) ) ;
#90442 = CARTESIAN_POINT ( 'NONE',  ( 29.61615870820702767, -281.2406369717811572, -308.1630850858723534 ) ) ;
#90443 = FACE_OUTER_BOUND ( 'NONE', #40658, .T. ) ;
#90444 = CARTESIAN_POINT ( 'NONE',  ( -96.33610129740313255, -277.1878192745356841, -224.0303015786622893 ) ) ;
#90445 = CARTESIAN_POINT ( 'NONE',  ( 150.6539576904058606, 293.9636489450775230, -9.103929867429224387 ) ) ;
#90446 = CARTESIAN_POINT ( 'NONE',  ( -108.7402307614557202, -289.1238630663619347, -287.3723004675085235 ) ) ;
#90447 = LINE ( 'NONE', #68716, #23029 ) ;
#90448 = CARTESIAN_POINT ( 'NONE',  ( 140.6539576904058606, 250.0000000000000568, -12.50000000000000000 ) ) ;
#90449 = CARTESIAN_POINT ( 'NONE',  ( -89.29822738331768051, -289.3211376660325413, -216.2012950742297335 ) ) ;
#90450 = CARTESIAN_POINT ( 'NONE',  ( -66.10141161950679134, -275.1888895343701620, -202.5113814432587560 ) ) ;
#90451 = CARTESIAN_POINT ( 'NONE',  ( 34.04354860159339324, -283.3251045196583391, -297.6146050172361583 ) ) ;
#90453 = CARTESIAN_POINT ( 'NONE',  ( -106.9858573769190286, -284.2621611793797456, -292.2401344389542146 ) ) ;
#90452 = CARTESIAN_POINT ( 'NONE',  ( -20.93113067675179906, -296.2767230804165592, -195.0114142401944264 ) ) ;
#90454 = CARTESIAN_POINT ( 'NONE',  ( -24.51140070544253646, -275.6442507432472553, -197.8469987294978125 ) ) ;
#90455 = CARTESIAN_POINT ( 'NONE',  ( 28.00092992438041506, -275.9093325594704993, -237.4530274233429452 ) ) ;
#90456 = CARTESIAN_POINT ( 'NONE',  ( -0.1019808792622469984, -284.5569116119880277, -335.4774467391374060 ) ) ;
#90458 = CARTESIAN_POINT ( 'NONE',  ( -52.67268509034047241, -296.9097616766705983, -198.6964329503011299 ) ) ;
#90457 = AXIS2_PLACEMENT_3D ( 'NONE', #980, #58745, #87588 ) ;
#90459 = ORIENTED_EDGE ( 'NONE', *, *, #22911, .F. ) ;
#90460 = CARTESIAN_POINT ( 'NONE',  ( 204.9097360766351130, 294.4826453818760683, -54.00000000002630429 ) ) ;
#90461 = CARTESIAN_POINT ( 'NONE',  ( -1.969369272137820870, -294.4300618183150391, -338.7555491472663221 ) ) ;
#90462 = CARTESIAN_POINT ( 'NONE',  ( -99.49017384628112382, -287.0933102938046773, -229.0160576099841307 ) ) ;
#90463 = DIRECTION ( 'NONE',  ( 0.000000000000000000, -1.000000000000000000, 0.000000000000000000 ) ) ;
#90464 = CARTESIAN_POINT ( 'NONE',  ( -99.90806341382575795, -281.4094976428775112, -320.2154176792147382 ) ) ;
#90465 = CARTESIAN_POINT ( 'NONE',  ( -31.47282331195544458, -276.1771342397307194, -347.0276969494658488 ) ) ;
#90466 = CARTESIAN_POINT ( 'NONE',  ( -113.0215390613652460, -288.8341820646413680, -279.6859390279827835 ) ) ;
#90467 = CARTESIAN_POINT ( 'NONE',  ( -32.07703169672834775, -284.5046599341272895, -343.8661587566058984 ) ) ;
#90468 = CARTESIAN_POINT ( 'NONE',  ( -95.23179281835876964, -279.6696906995564404, -316.4976339776339955 ) ) ;
#90469 = CARTESIAN_POINT ( 'NONE',  ( -100.5196209850382019, -286.5495977951537157, -227.2890596849693168 ) ) ;
#90470 = CARTESIAN_POINT ( 'NONE',  ( 22.92119638784911118, -282.9427202210016503, -225.6921835737705635 ) ) ;
#90471 = CARTESIAN_POINT ( 'NONE',  ( 35.72928442274577776, -275.4112629501662468, -245.9107351557189816 ) ) ;
#90472 = CARTESIAN_POINT ( 'NONE',  ( -75.33804700893723805, -277.3776311521315847, -337.3333333275879227 ) ) ;
#90473 = CARTESIAN_POINT ( 'NONE',  ( -42.46489358481200327, -297.0374314556101467, -344.6246156608897877 ) ) ;
#90474 = CARTESIAN_POINT ( 'NONE',  ( 208.6208076322478746, 32.98517505407394168, 10.50000000000000000 ) ) ;
#90475 = DIRECTION ( 'NONE',  ( 0.000000000000000000, 1.000000000000000000, 0.000000000000000000 ) ) ;
#90476 = CARTESIAN_POINT ( 'NONE',  ( -48.76006227618365330, -296.0479459154993265, -195.4088716011214899 ) ) ;
#90477 = CARTESIAN_POINT ( 'NONE',  ( -64.36172741372259054, -276.9220473737363477, -338.2964106327274294 ) ) ;
#90478 = CARTESIAN_POINT ( 'NONE',  ( -51.75605163194205005, -298.9516942827281696, -194.9829020043151502 ) ) ;
#90479 = CARTESIAN_POINT ( 'NONE',  ( 20.29031449776807960, -288.6644592594607275, -223.9026456087891006 ) ) ;
#90480 = CARTESIAN_POINT ( 'NONE',  ( -112.9177906086094936, -298.2064033619323595, -259.7325634386737647 ) ) ;
#90481 = CARTESIAN_POINT ( 'NONE',  ( -32.02467138531660851, -296.1915785838982629, -346.7924821553039578 ) ) ;
#90482 = CARTESIAN_POINT ( 'NONE',  ( -101.2911949615413647, -293.0744354850784816, -231.4960882580051020 ) ) ;
#90483 = CARTESIAN_POINT ( 'NONE',  ( -68.03553479123888792, -277.6480984893867685, -202.0982390200752263 ) ) ;
#90484 = CARTESIAN_POINT ( 'NONE',  ( -65.38075117785712109, -281.6028941185841177, -201.4036976774882532 ) ) ;
#90485 = CARTESIAN_POINT ( 'NONE',  ( -40.55615258561152103, -296.0912925320236013, -195.9777527788390898 ) ) ;
#90486 = CARTESIAN_POINT ( 'NONE',  ( -44.28208289165075939, -284.9993215759203622, -345.8598682605903605 ) ) ;
#90487 = CARTESIAN_POINT ( 'NONE',  ( 28.49938087140639098, -286.9073053107481996, -302.5974038332714713 ) ) ;
#90488 = CARTESIAN_POINT ( 'NONE',  ( 186.9901108754978054, 262.1367507616976127, -152.9611386112110836 ) ) ;
#90489 = CARTESIAN_POINT ( 'NONE',  ( 6.943116152020298415, -286.3404107245024761, -212.2374102784823720 ) ) ;
#90490 = ORIENTED_EDGE ( 'NONE', *, *, #26879, .T. ) ;
#90491 = CARTESIAN_POINT ( 'NONE',  ( -85.89600774059142907, -284.7865959364761466, -329.7241681159889026 ) ) ;
#90492 = CARTESIAN_POINT ( 'NONE',  ( -33.81466304744931506, -298.5898263505375780, -197.2992743959117092 ) ) ;
#90493 = CARTESIAN_POINT ( 'NONE',  ( -26.66120766543634701, -284.9799229863747314, -194.4531921616974444 ) ) ;
#90494 = CARTESIAN_POINT ( 'NONE',  ( -11.59958383191884224, -281.3204845604748812, -197.9854402697818330 ) ) ;
#90495 = CARTESIAN_POINT ( 'NONE',  ( 196.1243318874861927, 19.88069242108673507, -13.74009414728758216 ) ) ;
#90496 = CARTESIAN_POINT ( 'NONE',  ( -64.51370615259645547, -281.2240678548217261, -199.0004806361470173 ) ) ;
#90497 = CARTESIAN_POINT ( 'NONE',  ( 30.70113632595101549, -281.4191624949866082, -234.2486450573983916 ) ) ;
#90498 = CARTESIAN_POINT ( 'NONE',  ( -109.1418805571601069, -282.0523547857346784, -270.3284710469131937 ) ) ;
#90499 = CARTESIAN_POINT ( 'NONE',  ( -30.45121505427302822, -124.7187385046102577, -364.4204196855452551 ) ) ;
#90500 = ORIENTED_EDGE ( 'NONE', *, *, #29763, .F. ) ;
#90501 = CARTESIAN_POINT ( 'NONE',  ( -5.473321563751323282, -278.6321329384867909, -338.0836899838909062 ) ) ;
#90502 = CARTESIAN_POINT ( 'NONE',  ( 193.4698978865293100, 279.2676723978439099, -125.7697831199173493 ) ) ;
#90503 = CARTESIAN_POINT ( 'NONE',  ( 37.33344107558067293, -279.5491298462316081, -268.5686846150931046 ) ) ;
#90504 = CARTESIAN_POINT ( 'NONE',  ( 37.84583692617987083, -295.1685309301496432, -259.0174925633831435 ) ) ;
#90505 = CARTESIAN_POINT ( 'NONE',  ( -108.9862823002714691, -295.7085867948225655, -284.9474886127082414 ) ) ;
#90506 = CARTESIAN_POINT ( 'NONE',  ( -39.20391299603881663, -291.5370572017369568, -193.4321710414825191 ) ) ;
#90507 = CARTESIAN_POINT ( 'NONE',  ( -110.6395987777366372, -271.3322271728258670, -283.6871839692949493 ) ) ;
#90509 = CARTESIAN_POINT ( 'NONE',  ( 22.59969361385117637, -286.5473646369430867, -313.4130602447166893 ) ) ;
#90508 = CARTESIAN_POINT ( 'NONE',  ( -112.6265387581754567, -294.9584046760650153, -283.7295356724400790 ) ) ;
#90510 = CARTESIAN_POINT ( 'NONE',  ( 21.14159985307658118, -294.7785392034865595, -224.6178047424902786 ) ) ;
#90511 = CARTESIAN_POINT ( 'NONE',  ( -109.1503233189311572, -286.0730973678907390, -254.6573329654319764 ) ) ;
#90512 = CARTESIAN_POINT ( 'NONE',  ( 10.96140137255359193, -293.6428233615162071, -210.6300977006126232 ) ) ;
#90513 = CARTESIAN_POINT ( 'NONE',  ( 26.91214494292058390, -282.5186020735537227, -305.1380044889103829 ) ) ;
#90514 = CARTESIAN_POINT ( 'NONE',  ( -71.90866226528002869, -294.2938732441011780, -338.7214416260713961 ) ) ;
#90515 = CARTESIAN_POINT ( 'NONE',  ( -112.7076064441146457, -291.1665157253328289, -285.3990380602929235 ) ) ;
#90516 = CARTESIAN_POINT ( 'NONE',  ( -27.86289646378844154, -292.6616469247202303, -193.9551510633994837 ) ) ;
#90517 = CARTESIAN_POINT ( 'NONE',  ( -96.55737201012961179, -290.1217991645716552, -313.0519156803845817 ) ) ;
#90518 = VERTEX_POINT ( 'NONE', #58085 ) ;
#90519 = FACE_OUTER_BOUND ( 'NONE', #83632, .T. ) ;
#90520 = CARTESIAN_POINT ( 'NONE',  ( -113.1299716508203801, -298.3858968312070488, -272.4596064290795994 ) ) ;
#90521 = CARTESIAN_POINT ( 'NONE',  ( -113.7836448741590232, -271.4189930081095667, -264.6405309598038116 ) ) ;
#90522 = CARTESIAN_POINT ( 'NONE',  ( -4.230497036130876687, -279.5584965282023973, -205.0244694356096602 ) ) ;
#90523 = ORIENTED_EDGE ( 'NONE', *, *, #31936, .F. ) ;
#90524 = CARTESIAN_POINT ( 'NONE',  ( 2.391592923915218272, -274.0773285237768846, -204.4764283617008118 ) ) ;
#90525 = CIRCLE ( 'NONE', #87504, 0.5000000000000004441 ) ;
#90526 = CARTESIAN_POINT ( 'NONE',  ( -84.50384236265387017, -295.8692250111691351, -213.6690705701821571 ) ) ;
#90527 = CARTESIAN_POINT ( 'NONE',  ( -8.232863205915352367, -278.5273120249084968, -338.6650163409780703 ) ) ;
#90528 = CARTESIAN_POINT ( 'NONE',  ( -8.468905047304291500, -272.5735991943565750, -201.9160284759665274 ) ) ;
#90529 = CARTESIAN_POINT ( 'NONE',  ( -110.4472800381208373, -297.8501861935719717, -263.2765083089749396 ) ) ;
#90530 = CARTESIAN_POINT ( 'NONE',  ( -41.90124506154118222, -299.0730200822998768, -197.1939352843758968 ) ) ;
#90531 = DIRECTION ( 'NONE',  ( 0.000000000000000000, 0.000000000000000000, 1.000000000000000000 ) ) ;
#90532 = CARTESIAN_POINT ( 'NONE',  ( -105.8035841109465736, -298.5864088478954272, -236.9035201173315954 ) ) ;
#90533 = CARTESIAN_POINT ( 'NONE',  ( 95.17455889409825431, -297.7070312337581868, -195.2394971372179668 ) ) ;
#90534 = CARTESIAN_POINT ( 'NONE',  ( 23.42136893306190615, -293.6399350351919679, -229.7194877680895502 ) ) ;
#90535 = CARTESIAN_POINT ( 'NONE',  ( 30.40524502766028903, -291.7426236418784811, -241.4952184992853290 ) ) ;
#90536 = CARTESIAN_POINT ( 'NONE',  ( 38.12323504225818738, -276.2320633510027506, -285.3467932484457492 ) ) ;
#90537 = EDGE_CURVE ( 'NONE', #43024, #25984, #93087, .T. ) ;
#90538 = CARTESIAN_POINT ( 'NONE',  ( -109.1301048258702906, -272.8971213833867182, -256.8458732120670902 ) ) ;
#90539 = ADVANCED_FACE ( 'NONE', ( #79843 ), #22064, .T. ) ;
#90540 = CARTESIAN_POINT ( 'NONE',  ( -11.24742307381640849, -284.6938370694468290, -341.1095283698787739 ) ) ;
#90541 =( BOUNDED_CURVE ( )  B_SPLINE_CURVE ( 3, ( #12804, #62038, #18954, #70085 ),
 .UNSPECIFIED., .F., .F. ) 
 B_SPLINE_CURVE_WITH_KNOTS ( ( 4, 4 ),
 ( 3.141592653589793116, 4.289818581638156658 ),
 .UNSPECIFIED. ) 
 CURVE ( )  GEOMETRIC_REPRESENTATION_ITEM ( )  RATIONAL_B_SPLINE_CURVE ( ( 1.000000000000000000, 0.8931162488197521565, 0.8931162488197521565, 1.000000000000000000 ) ) 
 REPRESENTATION_ITEM ( '' )  );
#90542 = CARTESIAN_POINT ( 'NONE',  ( -70.27312709790456324, -282.1618575070084489, -339.4321271594369591 ) ) ;
#90543 = CARTESIAN_POINT ( 'NONE',  ( -68.98102638335927850, -276.8059643674052950, -340.4630626115244354 ) ) ;
#90544 = CARTESIAN_POINT ( 'NONE',  ( 205.7381008070597943, 1.000000000000000000, -6.999999999999991118 ) ) ;
#90545 = CARTESIAN_POINT ( 'NONE',  ( -94.41739525194741134, -283.1037433213924714, -316.1518576435993282 ) ) ;
#90546 = CARTESIAN_POINT ( 'NONE',  ( 33.86396058564700695, -279.8645509640809905, -294.6013771361581917 ) ) ;
#90547 = CARTESIAN_POINT ( 'NONE',  ( -4.821906802915019163, -275.1900306274544050, -336.3890416430190271 ) ) ;
#90548 = CARTESIAN_POINT ( 'NONE',  ( -111.7797188516766198, -280.4293875169361741, -279.9349634603549362 ) ) ;
#90549 = DIRECTION ( 'NONE',  ( 0.000000000000000000, 0.000000000000000000, 1.000000000000000000 ) ) ;
#90550 = CARTESIAN_POINT ( 'NONE',  ( -94.47303263745031643, -271.6419870804418792, -219.9383923306725706 ) ) ;
#90551 = CARTESIAN_POINT ( 'NONE',  ( -71.97281133627406291, -279.5090360652539516, -337.0891456231197481 ) ) ;
#90552 = CARTESIAN_POINT ( 'NONE',  ( 175.2296996224750103, 133.0000000000000000, 24.00000000000001066 ) ) ;
#90553 = CARTESIAN_POINT ( 'NONE',  ( -69.82840687882638520, -285.3966615483934675, -338.5950119462010548 ) ) ;
#90554 = EDGE_LOOP ( 'NONE', ( #87716, #86799, #88063, #19828, #42462, #74256 ) ) ;
#90555 = CYLINDRICAL_SURFACE ( 'NONE', #50140, 4.000000000000003553 ) ;
#90556 = CARTESIAN_POINT ( 'NONE',  ( 34.38310171782613622, -285.2673908178722968, -248.2655814507496075 ) ) ;
#90557 = CARTESIAN_POINT ( 'NONE',  ( 216.5288609127277084, 293.9636489450776935, -40.00000000000000711 ) ) ;
#90558 = CARTESIAN_POINT ( 'NONE',  ( -75.87953643057717557, -294.3737662519613991, -332.8860940508052977 ) ) ;
#90559 = CARTESIAN_POINT ( 'NONE',  ( -85.50411400532475170, -287.8656017415780184, -326.9201125168872863 ) ) ;
#90560 = CARTESIAN_POINT ( 'NONE',  ( 155.4148940283161835, 19.61091623264263362, -11.07022379048152239 ) ) ;
#90561 = CARTESIAN_POINT ( 'NONE',  ( -106.5996002965573695, -294.9276701843219826, -241.5801536071919884 ) ) ;
#90562 = CARTESIAN_POINT ( 'NONE',  ( -73.26929873800466453, -284.0648507988596521, -202.9830993872690783 ) ) ;
#90563 = CARTESIAN_POINT ( 'NONE',  ( 23.25314589603187798, -283.7330588521203936, -312.4883663038660870 ) ) ;
#90564 = CARTESIAN_POINT ( 'NONE',  ( -66.21227798649148610, -281.6647525063432909, -340.6635517949474661 ) ) ;
#90565 = CARTESIAN_POINT ( 'NONE',  ( 19.51348556975623083, -288.1995056051616757, -316.1485382993283224 ) ) ;
#90566 = CARTESIAN_POINT ( 'NONE',  ( -89.90708202472318078, -280.7175517807921210, -218.7888280785315942 ) ) ;
#90567 = CARTESIAN_POINT ( 'NONE',  ( -1.896780215286702154, -281.3373586711661005, -206.3590916116236542 ) ) ;
#90568 = CARTESIAN_POINT ( 'NONE',  ( 15.54983676550273053, -290.2889745846089795, -324.1076463553332587 ) ) ;
#90569 = ORIENTED_EDGE ( 'NONE', *, *, #40534, .T. ) ;
#90570 = CARTESIAN_POINT ( 'NONE',  ( -7.690579524509375986, -274.4300503898912780, -199.2424981971485067 ) ) ;
#90571 = CARTESIAN_POINT ( 'NONE',  ( -106.6306356591301636, -292.1669916897665189, -298.2646329065370878 ) ) ;
#90572 = CARTESIAN_POINT ( 'NONE',  ( 175.2296996224750103, 20.00000000000000000, 0.000000000000000000 ) ) ;
#90573 = CARTESIAN_POINT ( 'NONE',  ( -99.90806341382572953, -299.6948066931273047, -220.5068182859052968 ) ) ;
#90574 = ORIENTED_EDGE ( 'NONE', *, *, #3741, .T. ) ;
#90575 = CARTESIAN_POINT ( 'NONE',  ( 37.87262138082609653, -273.5624502598165577, -271.1777661500246381 ) ) ;
#90576 = CARTESIAN_POINT ( 'NONE',  ( 196.9830544186642953, 72.65363667333228648, 12.32798201617853984 ) ) ;
#90577 = CARTESIAN_POINT ( 'NONE',  ( -36.30597713269166604, -293.4392857900434137, -346.5670494187592112 ) ) ;
#90578 = CARTESIAN_POINT ( 'NONE',  ( -71.94867088985502335, -272.9307878819382154, -205.9133346863624467 ) ) ;
#90579 = CARTESIAN_POINT ( 'NONE',  ( -42.69513748755241522, -290.6408991098892898, -343.9108313187412591 ) ) ;
#90580 = CARTESIAN_POINT ( 'NONE',  ( 29.07010127890838191, -283.7503203867120760, -303.1492995913209256 ) ) ;
#90581 = CARTESIAN_POINT ( 'NONE',  ( -113.6009320973543169, -292.0380420358455922, -265.5511459457677006 ) ) ;
#90582 = CARTESIAN_POINT ( 'NONE',  ( -7.398745630150998842, -293.7518173882294263, -199.9429284146028465 ) ) ;
#90583 = CARTESIAN_POINT ( 'NONE',  ( -55.01030098087403530, -291.6518653089868849, -199.5316004888768759 ) ) ;
#90584 = CARTESIAN_POINT ( 'NONE',  ( -94.80339294769228786, -287.2184767542982513, -222.1620048122800597 ) ) ;
#90585 = CARTESIAN_POINT ( 'NONE',  ( -41.01051860918858694, -280.1738915585690961, -193.4353761973161454 ) ) ;
#90586 = CARTESIAN_POINT ( 'NONE',  ( -67.67104348097620914, -293.5268697507071352, -339.5669351673868164 ) ) ;
#90587 = CARTESIAN_POINT ( 'NONE',  ( -55.70423773753437757, -283.1155459800356198, -345.1395722125438397 ) ) ;
#90588 = CARTESIAN_POINT ( 'NONE',  ( 35.10381599171308409, -277.6234969144568367, -286.6212447235566287 ) ) ;
#90589 = CARTESIAN_POINT ( 'NONE',  ( -105.5795714935544112, -286.8376638359844719, -285.9686137636504668 ) ) ;
#90590 = AXIS2_PLACEMENT_3D ( 'NONE', #93061, #91164, #57105 ) ;
#90591 = CARTESIAN_POINT ( 'NONE',  ( -98.66419258219457333, -276.0915520697607235, -314.8787760645458320 ) ) ;
#90592 = DIRECTION ( 'NONE',  ( 1.124465274301078034E-16, 1.000000000000000000, 0.000000000000000000 ) ) ;
#90593 = CARTESIAN_POINT ( 'NONE',  ( -33.49925342348564783, -282.5101675445274623, -343.3341291046178299 ) ) ;
#90594 = CARTESIAN_POINT ( 'NONE',  ( -22.65740913718828153, -281.4410204041606107, -195.1248301900121760 ) ) ;
#90595 = CARTESIAN_POINT ( 'NONE',  ( 28.69521240344508328, -287.1224149888095099, -309.5012047962646875 ) ) ;
#90596 = CARTESIAN_POINT ( 'NONE',  ( 30.77975472383667821, -294.9275245018964142, -241.2915136975370274 ) ) ;
#90597 = CARTESIAN_POINT ( 'NONE',  ( -0.4507878081491541455, -276.1341585071139093, -203.6716920053025319 ) ) ;
#90598 = CARTESIAN_POINT ( 'NONE',  ( 2.149019613623236680, -275.8845582162140317, -204.8341668346853908 ) ) ;
#90599 = CARTESIAN_POINT ( 'NONE',  ( -87.09708192572611551, -277.6021384487344790, -323.7783622643488002 ) ) ;
#90600 = CARTESIAN_POINT ( 'NONE',  ( -106.4651649713362218, -298.9273471198818584, -241.6910110428851226 ) ) ;
#90601 = CARTESIAN_POINT ( 'NONE',  ( -74.44298135506785741, -283.5574047911027833, -205.3576201718144034 ) ) ;
#90602 = CARTESIAN_POINT ( 'NONE',  ( 13.26776739764922297, -292.4043044654659411, -212.3574449246964662 ) ) ;
#90603 = CARTESIAN_POINT ( 'NONE',  ( 20.89097088326920471, -289.8212973518486706, -319.5078009258397742 ) ) ;
#90604 = CARTESIAN_POINT ( 'NONE',  ( 35.93072163279381925, -292.4420104958599040, -268.0420056553431323 ) ) ;
#90605 = ORIENTED_EDGE ( 'NONE', *, *, #7600, .T. ) ;
#90606 = CARTESIAN_POINT ( 'NONE',  ( -69.35957396144178233, -290.2138235857514701, -200.9677691882640431 ) ) ;
#90607 = CARTESIAN_POINT ( 'NONE',  ( -33.50308118302822891, -291.7684830894787069, -197.4284433137697761 ) ) ;
#90608 = ORIENTED_EDGE ( 'NONE', *, *, #21310, .T. ) ;
#90609 = CARTESIAN_POINT ( 'NONE',  ( -3.185999573392908957, -289.6913388354190033, -339.0406772653464031 ) ) ;
#90610 = CARTESIAN_POINT ( 'NONE',  ( -81.30399101819510577, -279.7692269770939220, -211.9932115196273799 ) ) ;
#90611 = CARTESIAN_POINT ( 'NONE',  ( -68.04103870623133332, -296.5789054304839851, -200.0262277653163494 ) ) ;
#90612 = CARTESIAN_POINT ( 'NONE',  ( -87.68947464013822923, -286.0221398584377539, -212.1664879785889752 ) ) ;
#90613 = CARTESIAN_POINT ( 'NONE',  ( -4.786748280962233260, -286.8025829718178557, -200.6049755872068374 ) ) ;
#90614 = CARTESIAN_POINT ( 'NONE',  ( -106.1922471466907183, -284.5600154893914464, -294.8363354118778261 ) ) ;
#90615 = CARTESIAN_POINT ( 'NONE',  ( 203.3290562182569090, 295.9433822784110362, -54.00000000004157386 ) ) ;
#90616 = CARTESIAN_POINT ( 'NONE',  ( -100.5277185204516144, -246.4223321106570097, -332.7819595289345216 ) ) ;
#90617 = CARTESIAN_POINT ( 'NONE',  ( 137.9338102360727873, 178.6954944670252416, -238.2672434279379843 ) ) ;
#90618 = CARTESIAN_POINT ( 'NONE',  ( 33.99349039586270038, -274.5348307297093697, -254.0603081086666464 ) ) ;
#90619 = CARTESIAN_POINT ( 'NONE',  ( -9.885297577637768285, -275.6052940316844797, -338.3480584340046562 ) ) ;
#90620 = CARTESIAN_POINT ( 'NONE',  ( -93.61345767255416206, -296.7763583323657031, -217.8142208377114457 ) ) ;
#90621 = CARTESIAN_POINT ( 'NONE',  ( 85.86301894190751227, 81.15251262249802267, -299.4358512761199336 ) ) ;
#90622 = CARTESIAN_POINT ( 'NONE',  ( 35.26728156765977928, -273.9296478136211022, -246.0852129532705703 ) ) ;
#90623 = CARTESIAN_POINT ( 'NONE',  ( -85.99290297156427698, -275.1275707684375220, -214.5161435434588100 ) ) ;
#90624 = ORIENTED_EDGE ( 'NONE', *, *, #92813, .F. ) ;
#90625 = CARTESIAN_POINT ( 'NONE',  ( -81.08540120362570747, -274.5531893405452593, -207.3048453682714580 ) ) ;
#90626 = CARTESIAN_POINT ( 'NONE',  ( -107.8128992308467815, -291.2990398897558748, -251.0790398058898631 ) ) ;
#90627 = CARTESIAN_POINT ( 'NONE',  ( -50.42993694010502992, -296.0178825118061923, -346.1305805619630860 ) ) ;
#90628 = CARTESIAN_POINT ( 'NONE',  ( -112.2159187317890598, -297.2660806873803381, -252.6586240328183521 ) ) ;
#90629 = CARTESIAN_POINT ( 'NONE',  ( -86.48840921147282756, -295.9246126122980627, -324.3389003634646315 ) ) ;
#90630 = VERTEX_POINT ( 'NONE', #59474 ) ;
#90631 = CARTESIAN_POINT ( 'NONE',  ( -42.67957362113180153, -279.0391638687532918, -345.7323413049605847 ) ) ;
#90632 = EDGE_CURVE ( 'NONE', #77294, #4433, #2171, .T. ) ;
#90633 = ORIENTED_EDGE ( 'NONE', *, *, #53671, .F. ) ;
#90634 = CARTESIAN_POINT ( 'NONE',  ( 38.19546491524776144, -280.8768524322094891, -255.7438815600982025 ) ) ;
#90635 = CARTESIAN_POINT ( 'NONE',  ( 9.824706139981804753, -277.3249706530182834, -326.3855641391881477 ) ) ;
#90636 = CARTESIAN_POINT ( 'NONE',  ( 21.86572908666779824, -277.9592877654428662, -318.0100010161548880 ) ) ;
#90637 = CARTESIAN_POINT ( 'NONE',  ( -106.0861757196606163, -276.1680286674200602, -301.3524653305345282 ) ) ;
#90638 = CARTESIAN_POINT ( 'NONE',  ( -27.28790972808698001, -274.6755835064429903, -197.9436809192020803 ) ) ;
#90639 = CARTESIAN_POINT ( 'NONE',  ( -80.05542733467437699, -296.0359304892675141, -210.4368956361018093 ) ) ;
#90640 = PLANE ( 'NONE',  #7884 ) ;
#90641 = EDGE_CURVE ( 'NONE', #87746, #5433, #52258, .T. ) ;
#90642 = CARTESIAN_POINT ( 'NONE',  ( -107.2277311223854070, -278.9981054427363460, -249.2674536168235875 ) ) ;
#90643 = CARTESIAN_POINT ( 'NONE',  ( -45.98678922299930605, -287.8442927162407727, -346.4307498323549339 ) ) ;
#90644 = CARTESIAN_POINT ( 'NONE',  ( -32.82907011243004547, -276.1091532367080390, -195.4841864206673847 ) ) ;
#90645 = CARTESIAN_POINT ( 'NONE',  ( 196.8803347170859865, 20.19615242270636557, -12.49999999999999289 ) ) ;
#90646 = CARTESIAN_POINT ( 'NONE',  ( -96.69559085280752697, -289.1524431895654175, -313.1363138688400909 ) ) ;
#90647 = CARTESIAN_POINT ( 'NONE',  ( -89.81062465253063465, -284.6836706174646565, -214.0719371500587442 ) ) ;
#90648 = CARTESIAN_POINT ( 'NONE',  ( 33.92926937936289278, -280.0522227695563515, -290.3216520527920466 ) ) ;
#90650 = CARTESIAN_POINT ( 'NONE',  ( -108.7290556674159063, -282.9078703479744945, -249.0837395250946713 ) ) ;
#90649 = CARTESIAN_POINT ( 'NONE',  ( 32.78734996933208379, -280.4221407947374018, -292.8269739511292755 ) ) ;
#90652 = CARTESIAN_POINT ( 'NONE',  ( -69.51293540009807259, -287.6289154997058972, -202.5975507336678163 ) ) ;
#90651 = AXIS2_PLACEMENT_3D ( 'NONE', #62453, #3270, #10366 ) ;
#90653 = CARTESIAN_POINT ( 'NONE',  ( -103.4822045126110481, -279.3276377534990615, -302.2994821243185015 ) ) ;
#90654 = DIRECTION ( 'NONE',  ( -0.000000000000000000, 0.000000000000000000, -1.000000000000000000 ) ) ;
#90655 = CARTESIAN_POINT ( 'NONE',  ( -44.72615378725276969, -293.9589824281899268, -195.6739853190973975 ) ) ;
#90656 = CARTESIAN_POINT ( 'NONE',  ( -112.2339107445989868, -276.9548691370670213, -257.5107948838872858 ) ) ;
#90657 = AXIS2_PLACEMENT_3D ( 'NONE', #68351, #38977, #61271 ) ;
#90658 = CARTESIAN_POINT ( 'NONE',  ( 19.26578866550989133, -276.8577630935376988, -316.6354122796417982 ) ) ;
#90659 = CARTESIAN_POINT ( 'NONE',  ( -4.930710786768611520, -284.6265849785726232, -338.1952929343584060 ) ) ;
#90660 = CARTESIAN_POINT ( 'NONE',  ( 198.6806486734898272, 66.92004278903957015, 8.362876768746247080 ) ) ;
#90661 = CARTESIAN_POINT ( 'NONE',  ( -90.56650167772804139, -291.7187488390284216, -324.0670995159550216 ) ) ;
#90662 = CARTESIAN_POINT ( 'NONE',  ( -75.10123183301142546, -293.5550138477503879, -335.1772404801290577 ) ) ;
#90663 = CARTESIAN_POINT ( 'NONE',  ( 35.69874235161989873, -286.4465967501391219, -246.3318718969451311 ) ) ;
#90664 = CARTESIAN_POINT ( 'NONE',  ( -49.80398252576205920, -290.2905506021631368, -197.5690644006636774 ) ) ;
#90665 = LINE ( 'NONE', #25825, #72405 ) ;
#90666 = CARTESIAN_POINT ( 'NONE',  ( 34.64424301569840736, -274.4310025422716990, -285.1688007543081653 ) ) ;
#90667 = CARTESIAN_POINT ( 'NONE',  ( -35.64575197263904016, -293.1702674211743442, -344.5896546003434651 ) ) ;
#90668 = SURFACE_STYLE_USAGE ( .BOTH. , #61386 ) ;
#90669 = LINE ( 'NONE', #90219, #83723 ) ;
#90670 = CARTESIAN_POINT ( 'NONE',  ( -112.9762366047404640, -289.1644397743135642, -259.8693321595174552 ) ) ;
#90671 = CARTESIAN_POINT ( 'NONE',  ( -75.14723633963060934, -287.1393933818288815, -206.9798759082806896 ) ) ;
#90672 = CARTESIAN_POINT ( 'NONE',  ( -71.47167865511831053, -287.7366007749833443, -338.2516076156232998 ) ) ;
#90673 = CARTESIAN_POINT ( 'NONE',  ( -104.0270410264673728, -286.3957068942892192, -239.1204850148393177 ) ) ;
#90674 = CARTESIAN_POINT ( 'NONE',  ( 151.4851178187871312, 21.00000000000000000, -3.492110388858666870 ) ) ;
#90675 = CARTESIAN_POINT ( 'NONE',  ( -95.09080413602785598, -285.9866801744764189, -225.4225942282864423 ) ) ;
#90676 = CARTESIAN_POINT ( 'NONE',  ( 12.17821917378289953, -294.7171054700545483, -213.5616074885234354 ) ) ;
#90677 = CARTESIAN_POINT ( 'NONE',  ( -41.33329328226338362, -275.1818595130561107, -345.8285784664917060 ) ) ;
#90678 = CARTESIAN_POINT ( 'NONE',  ( 29.07984607417623835, -276.3920240203173080, -309.2702748940043875 ) ) ;
#90679 = CARTESIAN_POINT ( 'NONE',  ( 21.99279681067072900, -290.9941651548755885, -223.5565506714850414 ) ) ;
#90680 = CARTESIAN_POINT ( 'NONE',  ( -93.07375337715214414, -279.2792445185638712, -217.1536065092782906 ) ) ;
#90681 = CARTESIAN_POINT ( 'NONE',  ( -111.8828994258877430, -298.4813300197060357, -274.2925817380099716 ) ) ;
#90682 = CARTESIAN_POINT ( 'NONE',  ( 164.2231345125756263, 264.6571197653884155, -7.500000000000000000 ) ) ;
#90683 = DIRECTION ( 'NONE',  ( 1.110223024625155531E-13, 0.000000000000000000, 1.000000000000000000 ) ) ;
#90684 = CARTESIAN_POINT ( 'NONE',  ( -111.5152681033728612, -276.6524956580881849, -273.3855669416655019 ) ) ;
#90685 = CARTESIAN_POINT ( 'NONE',  ( 37.62000210017881585, -279.5827599649646800, -272.7577499571896169 ) ) ;
#90686 = DIRECTION ( 'NONE',  ( 0.7666168903225505371, 0.000000000000000000, -0.6421047760857900855 ) ) ;
#90687 = CARTESIAN_POINT ( 'NONE',  ( 36.91265796786614573, -274.2545288238475223, -287.9956782465559399 ) ) ;
#90688 = CARTESIAN_POINT ( 'NONE',  ( 6.490727046354843210, -295.9647838861012588, -329.6651332146280993 ) ) ;
#90689 = CARTESIAN_POINT ( 'NONE',  ( -33.08968521958203723, -281.9201386677901269, -346.9471255576982003 ) ) ;
#90690 = CARTESIAN_POINT ( 'NONE',  ( -88.65819797007746672, -296.7348767808570074, -322.6820201918375233 ) ) ;
#90691 = CARTESIAN_POINT ( 'NONE',  ( -67.99535505441080829, -298.9733638128169559, -200.2072329143113905 ) ) ;
#90692 = CARTESIAN_POINT ( 'NONE',  ( -5.294946954141301454, -274.1526001175590181, -204.7340811125050095 ) ) ;
#90693 = CARTESIAN_POINT ( 'NONE',  ( -25.10726373508821396, -294.2081860196391290, -196.3128317803379446 ) ) ;
#90694 = CARTESIAN_POINT ( 'NONE',  ( 36.38600856691606111, -287.9980934139662168, -292.6155855646658210 ) ) ;
#90695 = CARTESIAN_POINT ( 'NONE',  ( 35.30228972421073763, -273.9666682000668061, -291.9279064809528563 ) ) ;
#90696 = CARTESIAN_POINT ( 'NONE',  ( -46.02787954747933696, -288.9926015983626257, -346.9227429523101023 ) ) ;
#90697 = CARTESIAN_POINT ( 'NONE',  ( 34.23810733270660478, -286.8152198767577943, -285.9034150297784436 ) ) ;
#90698 = CARTESIAN_POINT ( 'NONE',  ( -39.13758790572180146, -290.0294877941399818, -195.3699211357650540 ) ) ;
#90699 = ORIENTED_EDGE ( 'NONE', *, *, #32642, .T. ) ;
#90700 = DIRECTION ( 'NONE',  ( 1.000000000000000000, 0.000000000000000000, 0.000000000000000000 ) ) ;
#90701 = CARTESIAN_POINT ( 'NONE',  ( 12.19292191415735971, -287.8484076537902183, -324.1356281857199519 ) ) ;
#90702 = DIRECTION ( 'NONE',  ( 0.000000000000000000, 0.000000000000000000, 1.000000000000000000 ) ) ;
#90703 = CARTESIAN_POINT ( 'NONE',  ( -71.62287469123025119, -284.4352618367339005, -339.0460601790132387 ) ) ;
#90704 = CARTESIAN_POINT ( 'NONE',  ( 38.99349840474387463, -292.5030567905028533, -261.7642130439592734 ) ) ;
#90705 = CARTESIAN_POINT ( 'NONE',  ( -25.53980054998473648, -281.8002742272543628, -195.0806053637984121 ) ) ;
#90706 = CARTESIAN_POINT ( 'NONE',  ( -50.86899104264909965, -281.1979495101255111, -195.0596527109729550 ) ) ;
#90707 = CARTESIAN_POINT ( 'NONE',  ( -71.41076191019858754, -283.3486884180255174, -334.9234834427126657 ) ) ;
#90708 = CARTESIAN_POINT ( 'NONE',  ( -67.58645676448941231, -279.4491100240194328, -338.9924180400056457 ) ) ;
#90709 = CARTESIAN_POINT ( 'NONE',  ( -110.8131257326467392, -296.8436739640969790, -247.1420255719417298 ) ) ;
#90710 = CARTESIAN_POINT ( 'NONE',  ( -32.67634471788182537, -275.4273242342445087, -197.0035825727832446 ) ) ;
#90711 = CARTESIAN_POINT ( 'NONE',  ( -111.7646678862558929, -288.4898831002248585, -276.7460579482406047 ) ) ;
#90712 = CARTESIAN_POINT ( 'NONE',  ( -81.29659581834329174, -272.2346935961606960, -211.5172749958831275 ) ) ;
#90713 = ORIENTED_EDGE ( 'NONE', *, *, #75906, .F. ) ;
#90714 = ORIENTED_EDGE ( 'NONE', *, *, #71361, .F. ) ;
#90715 = DIRECTION ( 'NONE',  ( -0.000000000000000000, 1.000000000000000000, -0.000000000000000000 ) ) ;
#90716 = CARTESIAN_POINT ( 'NONE',  ( -111.7494130062512312, -286.5006740938570147, -268.1687541312248300 ) ) ;
#90717 = CARTESIAN_POINT ( 'NONE',  ( 31.95662831818015093, -295.0559047529468444, -303.3366583851507130 ) ) ;
#90718 = CARTESIAN_POINT ( 'NONE',  ( -89.74170372891182978, -285.9402786022944269, -219.3165910058665418 ) ) ;
#90719 = CARTESIAN_POINT ( 'NONE',  ( 32.79990346686290792, -275.0102467585803652, -301.5536757076124559 ) ) ;
#90720 = CARTESIAN_POINT ( 'NONE',  ( -112.8264954240849676, -291.3881973638704608, -255.6173880199340545 ) ) ;
#90721 = CARTESIAN_POINT ( 'NONE',  ( -35.15968300279987346, -284.2188319458764454, -194.6148093390386009 ) ) ;
#90722 = CIRCLE ( 'NONE', #43907, 25.00000000000000355 ) ;
#90723 = CARTESIAN_POINT ( 'NONE',  ( -67.01121706702680569, -292.0070216581106024, -199.3296879239660768 ) ) ;
#90724 = CARTESIAN_POINT ( 'NONE',  ( -73.55176158966020239, -289.8801298503398129, -333.7862494643336504 ) ) ;
#90725 = PLANE ( 'NONE',  #85237 ) ;
#90726 = DIRECTION ( 'NONE',  ( -1.000000000000000000, 0.000000000000000000, 0.000000000000000000 ) ) ;
#90727 = CARTESIAN_POINT ( 'NONE',  ( -110.7271127053023747, -271.1905260033421428, -283.6752375529766255 ) ) ;
#90728 = CIRCLE ( 'NONE', #42363, 6.649382010133625620 ) ;
#90729 = CARTESIAN_POINT ( 'NONE',  ( -3.185662161419823057, -284.1294238190711212, -338.6110628531907309 ) ) ;
#90730 = CARTESIAN_POINT ( 'NONE',  ( -85.28047601435909542, -282.9094976428775681, -210.1954327657594206 ) ) ;
#90731 = ORIENTED_EDGE ( 'NONE', *, *, #77442, .F. ) ;
#90732 = CARTESIAN_POINT ( 'NONE',  ( 14.13197469526531869, -281.2290757296504466, -322.6311112145170341 ) ) ;
#90733 = CARTESIAN_POINT ( 'NONE',  ( -70.29581879405932909, -277.1413115772413676, -339.9440097967894872 ) ) ;
#90734 = CARTESIAN_POINT ( 'NONE',  ( -24.58837989201014196, -282.2154531742766608, -196.6225171904349338 ) ) ;
#90735 = CARTESIAN_POINT ( 'NONE',  ( -28.99282367148100903, -125.6822456004873771, -362.4878069686170079 ) ) ;
#90736 = CIRCLE ( 'NONE', #6170, 2.000000000000000000 ) ;
#90737 = CARTESIAN_POINT ( 'NONE',  ( 37.41203481182020596, -279.9266348538377542, -254.4717227220314442 ) ) ;
#90738 = CARTESIAN_POINT ( 'NONE',  ( -57.82199640242539118, -283.8065939204187202, -198.5270754086298268 ) ) ;
#90739 = CARTESIAN_POINT ( 'NONE',  ( -96.85772876603391524, -275.0498151047976307, -223.4767088475412891 ) ) ;
#90740 = CARTESIAN_POINT ( 'NONE',  ( -106.9259586923700738, -296.7474464306404798, -292.7963462226406364 ) ) ;
#90741 = ORIENTED_EDGE ( 'NONE', *, *, #25784, .F. ) ;
#90742 = CARTESIAN_POINT ( 'NONE',  ( 15.23997291625055972, -291.4984240644922124, -218.9422159366309302 ) ) ;
#90743 = CARTESIAN_POINT ( 'NONE',  ( -65.05058793322571375, -278.0560987127101953, -342.1496786930522944 ) ) ;
#90744 = CARTESIAN_POINT ( 'NONE',  ( 13.49665661008067197, -274.7884575658887343, -217.9735098661038819 ) ) ;
#90745 = CARTESIAN_POINT ( 'NONE',  ( 38.19007794046916615, -274.3047475889360953, -257.0028189701606038 ) ) ;
#90746 = DIRECTION ( 'NONE',  ( 0.000000000000000000, 0.000000000000000000, -1.000000000000000000 ) ) ;
#90747 = CARTESIAN_POINT ( 'NONE',  ( 15.92346366696724758, -272.8062822572314303, -217.4885609906349089 ) ) ;
#90748 = EDGE_CURVE ( 'NONE', #9431, #4576, #90017, .T. ) ;
#90749 = DIRECTION ( 'NONE',  ( 0.000000000000000000, -1.000000000000000000, 0.000000000000000000 ) ) ;
#90750 = CARTESIAN_POINT ( 'NONE',  ( -43.49052031076330138, -253.6529657927480343, -491.6564673409728243 ) ) ;
#90751 = CARTESIAN_POINT ( 'NONE',  ( -40.23284258655100842, -284.1690195968155876, -343.6131989739774326 ) ) ;
#90752 = CARTESIAN_POINT ( 'NONE',  ( 27.45281009266694028, -283.8389541093177399, -310.1552793963434738 ) ) ;
#90753 = CARTESIAN_POINT ( 'NONE',  ( -91.59130234939324566, -284.6022041161181733, -221.2880414379674505 ) ) ;
#90754 = CARTESIAN_POINT ( 'NONE',  ( -37.83534143752670076, -275.4582703718180028, -344.1720588528639269 ) ) ;
#90755 = CARTESIAN_POINT ( 'NONE',  ( 25.18338072479433620, -283.9580495583956576, -310.4741544580930963 ) ) ;
#90756 = CARTESIAN_POINT ( 'NONE',  ( -95.00757145578261031, -276.3899587625733716, -316.2654287131900332 ) ) ;
#90757 = DIRECTION ( 'NONE',  ( 1.000000000000000000, 0.000000000000000000, 0.000000000000000000 ) ) ;
#90758 = CARTESIAN_POINT ( 'NONE',  ( 34.92807391409401419, -276.4692673562082632, -257.9859943910513493 ) ) ;
#90759 = CARTESIAN_POINT ( 'NONE',  ( 9.339199855150265961, -232.1443419142230766, 25.50000000000000000 ) ) ;
#90760 = CARTESIAN_POINT ( 'NONE',  ( -39.59279386983942572, -280.8274204208516380, -193.5425520394794603 ) ) ;
#90761 = ORIENTED_EDGE ( 'NONE', *, *, #49105, .T. ) ;
#90762 = ORIENTED_EDGE ( 'NONE', *, *, #50406, .T. ) ;
#90763 = CARTESIAN_POINT ( 'NONE',  ( 201.2104617360081704, 15.00000000000000711, 10.00000000000000178 ) ) ;
#90764 = CARTESIAN_POINT ( 'NONE',  ( -40.78444846782597466, -287.8698272199731036, -194.6232190237568602 ) ) ;
#90765 = CARTESIAN_POINT ( 'NONE',  ( -98.87464204118074917, -295.2017193826217181, -310.0304370559154563 ) ) ;
#90766 = EDGE_CURVE ( 'NONE', #90187, #44672, #73220, .T. ) ;
#90767 = CARTESIAN_POINT ( 'NONE',  ( -110.6871379944550284, -289.6080601826063798, -293.6383752179008866 ) ) ;
#90769 = CARTESIAN_POINT ( 'NONE',  ( -109.9369931501766473, -288.6035623757123290, -284.8446897221598419 ) ) ;
#90768 = CARTESIAN_POINT ( 'NONE',  ( 32.40479769056452852, -285.8176067488831791, -246.8919688947097484 ) ) ;
#90770 = CARTESIAN_POINT ( 'NONE',  ( -109.3213669527072796, -285.9455691458234696, -256.0063950772644148 ) ) ;
#90771 = CARTESIAN_POINT ( 'NONE',  ( 35.69330733689766788, -273.3323524578737533, -253.2497194818602679 ) ) ;
#90772 = CARTESIAN_POINT ( 'NONE',  ( 15.75648205511122413, -285.1888796384633338, -215.7074496420666492 ) ) ;
#90773 = CARTESIAN_POINT ( 'NONE',  ( -94.07536742764946780, -299.2332506693597338, -221.2296079597851701 ) ) ;
#90774 = CARTESIAN_POINT ( 'NONE',  ( 35.60398651599691533, -285.3195529151811911, -252.2239949935032257 ) ) ;
#90775 = EDGE_CURVE ( 'NONE', #87609, #1443, #15921, .T. ) ;
#90776 = CARTESIAN_POINT ( 'NONE',  ( -59.81720391746119958, -280.6950983122616776, -200.6064174696220732 ) ) ;
#90777 = CARTESIAN_POINT ( 'NONE',  ( -40.24189749623339196, -291.0886579452007936, -345.4845886921014539 ) ) ;
#90778 = CARTESIAN_POINT ( 'NONE',  ( 196.7806748523260012, 275.0000000000000568, -12.67104836398113044 ) ) ;
#90779 = CARTESIAN_POINT ( 'NONE',  ( 156.4851178187871312, 16.95599219719193229, -7.000000000000000000 ) ) ;
#90780 = CARTESIAN_POINT ( 'NONE',  ( -47.41494026100687620, -297.0993814537765729, -345.2466575045077093 ) ) ;
#90781 = CARTESIAN_POINT ( 'NONE',  ( -95.47504139763903197, -277.2049161283542276, -222.9742496968694070 ) ) ;
#90782 = CARTESIAN_POINT ( 'NONE',  ( 37.26761126129164836, -292.5189842737098616, -251.9869656163303375 ) ) ;
#90783 = CARTESIAN_POINT ( 'NONE',  ( -102.1797782835470372, -294.4761343281002155, -305.6097212797882889 ) ) ;
#90784 = CARTESIAN_POINT ( 'NONE',  ( 22.52487147336448103, -279.6455000491359328, -227.7320541480066822 ) ) ;
#90785 = CARTESIAN_POINT ( 'NONE',  ( 24.25741404626410613, -273.0617666028388726, -228.5427492967688465 ) ) ;
#90786 = CARTESIAN_POINT ( 'NONE',  ( 32.26272471197889047, -294.5541223951385064, -246.6132427903760629 ) ) ;
#90787 = CARTESIAN_POINT ( 'NONE',  ( -4.771743288812468897, -297.1233781216987495, -337.9199732462171255 ) ) ;
#90788 = CARTESIAN_POINT ( 'NONE',  ( -98.52482178799844803, -295.6443190632586493, -224.7396090861023197 ) ) ;
#90789 = CARTESIAN_POINT ( 'NONE',  ( 1.235417138314658825, -292.7842079968534676, -335.8269872350154515 ) ) ;
#90790 = CARTESIAN_POINT ( 'NONE',  ( -97.25155038459429591, -292.5706966546655963, -227.5410149624957228 ) ) ;
#90791 = CARTESIAN_POINT ( 'NONE',  ( 184.7149167944524493, -12.49482340714361506, 13.00000000000000178 ) ) ;
#90792 = CARTESIAN_POINT ( 'NONE',  ( -32.15602269518463174, -292.9220355325602441, -197.3710042110249674 ) ) ;
#90793 = VECTOR ( 'NONE', #41827, 1000.000000000000000 ) ;
#90794 = DIRECTION ( 'NONE',  ( -0.000000000000000000, -0.000000000000000000, -1.000000000000000000 ) ) ;
#90796 = CARTESIAN_POINT ( 'NONE',  ( 32.75017600945747631, -293.8225269863071958, -290.8052846791266575 ) ) ;
#90795 = CARTESIAN_POINT ( 'NONE',  ( -75.93759716164696272, -281.5845770773004801, -335.1422854697101457 ) ) ;
#90797 = CARTESIAN_POINT ( 'NONE',  ( 29.76189961588162802, -282.0433402970852512, -308.2336156541696255 ) ) ;
#90798 = CARTESIAN_POINT ( 'NONE',  ( -27.37904345720521349, -282.5957119380627773, -346.7459110438595076 ) ) ;
#90799 = CARTESIAN_POINT ( 'NONE',  ( -51.11323504701555009, -287.2282702317662597, -343.9693374711361002 ) ) ;
#90800 = DIRECTION ( 'NONE',  ( 0.000000000000000000, 0.000000000000000000, 1.000000000000000000 ) ) ;
#90801 = CARTESIAN_POINT ( 'NONE',  ( 36.86950565664233181, -280.2568201587477574, -288.1764287928633621 ) ) ;
#90802 = CARTESIAN_POINT ( 'NONE',  ( 39.29470688452499871, -286.5234531919795700, -274.4203385729160232 ) ) ;
#90803 = CARTESIAN_POINT ( 'NONE',  ( 196.6777378159611089, 42.34889665583091301, 12.85090812620430789 ) ) ;
#90804 = CARTESIAN_POINT ( 'NONE',  ( 35.26662907435790117, -294.9790120047310324, -257.0822072083031458 ) ) ;
#90805 = CARTESIAN_POINT ( 'NONE',  ( 7.906858141154913255, -277.8730543295356483, -331.9991500484283620 ) ) ;
#90806 = CARTESIAN_POINT ( 'NONE',  ( -49.14114707759480893, -279.5643449837300523, -198.2996127361045922 ) ) ;
#90807 = CARTESIAN_POINT ( 'NONE',  ( 15.43662031107284527, -292.9399943472093355, -214.2214419023893015 ) ) ;
#90808 = CARTESIAN_POINT ( 'NONE',  ( -95.18405559082212619, -281.9647369262138454, -318.9977694731877591 ) ) ;
#90809 = CARTESIAN_POINT ( 'NONE',  ( 27.70098935140995877, -292.1546597211358289, -236.7031769777707382 ) ) ;
#90810 = CARTESIAN_POINT ( 'NONE',  ( -72.32446760326256197, -295.5895106967657284, -203.9622226827561349 ) ) ;
#90811 = ORIENTED_EDGE ( 'NONE', *, *, #67295, .F. ) ;
#90812 = DIRECTION ( 'NONE',  ( 0.000000000000000000, -1.000000000000000000, 0.000000000000000000 ) ) ;
#90813 = CARTESIAN_POINT ( 'NONE',  ( 25.84274323658424066, -293.5626646024749675, -307.0451002940258149 ) ) ;
#90814 = CARTESIAN_POINT ( 'NONE',  ( 200.3359402460285139, 61.72811464988816255, 8.999999999999998224 ) ) ;
#90815 = CARTESIAN_POINT ( 'NONE',  ( -105.5795714935544112, -294.2666405000204009, -254.7536222014695397 ) ) ;
#90816 = CARTESIAN_POINT ( 'NONE',  ( -43.25962040804878939, -297.0380362544216837, -193.7718148774431768 ) ) ;
#90817 = CARTESIAN_POINT ( 'NONE',  ( 24.90182803548134416, -280.2719941749095938, -313.5817110121290057 ) ) ;
#90818 = CARTESIAN_POINT ( 'NONE',  ( 23.45926181923605114, -288.2439211521247557, -223.9010684759691685 ) ) ;
#90819 = CARTESIAN_POINT ( 'NONE',  ( -53.41059323400035197, -289.0973876626331958, -341.5706024550187294 ) ) ;
#90820 = CARTESIAN_POINT ( 'NONE',  ( -43.24349816381648992, -278.6481559529793799, -343.8177482659192492 ) ) ;
#90821 = CARTESIAN_POINT ( 'NONE',  ( -111.6861101016002067, -294.6657313476734430, -263.1154739724864271 ) ) ;
#90822 = CARTESIAN_POINT ( 'NONE',  ( -110.3774713696544012, -274.2950787127233525, -259.4179901304113400 ) ) ;
#90823 = CARTESIAN_POINT ( 'NONE',  ( -94.77328336420495702, -276.7049539764182100, -316.0839746052255919 ) ) ;
#90824 = ORIENTED_EDGE ( 'NONE', *, *, #75312, .T. ) ;
#90825 = CARTESIAN_POINT ( 'NONE',  ( -33.33159068575541539, -297.7677945479111372, -193.3824812397034236 ) ) ;
#90826 = CARTESIAN_POINT ( 'NONE',  ( -78.95963072396740756, -291.5377859905910896, -332.1423800828387130 ) ) ;
#90827 = CARTESIAN_POINT ( 'NONE',  ( 16.90561464842478046, -294.4088868646498440, -216.7735773249501676 ) ) ;
#90828 = DIRECTION ( 'NONE',  ( 0.000000000000000000, 0.000000000000000000, -1.000000000000000000 ) ) ;
#90829 = ADVANCED_FACE ( 'NONE', ( #37665 ), #52350, .T. ) ;
#90830 = CARTESIAN_POINT ( 'NONE',  ( -94.37564041733163833, -291.8491158251868001, -224.6135265382596060 ) ) ;
#90831 = CARTESIAN_POINT ( 'NONE',  ( -48.18343439339476220, -250.0149903365356749, -455.0345092807172023 ) ) ;
#90832 = CARTESIAN_POINT ( 'NONE',  ( -114.1314867415316030, -297.1412005554776670, -275.3410497286744203 ) ) ;
#90833 = CARTESIAN_POINT ( 'NONE',  ( -76.51008214538381935, -289.6740885983111298, -205.4458354417788541 ) ) ;
#90834 = CARTESIAN_POINT ( 'NONE',  ( 30.76082294611260082, -299.2162576857911063, -193.3785011460888654 ) ) ;
#90835 = CARTESIAN_POINT ( 'NONE',  ( 194.2870706637141325, 250.0000000000000568, 14.58823529411763431 ) ) ;
#90836 = CARTESIAN_POINT ( 'NONE',  ( 195.2729366661233144, 26.72345838548328345, 14.94480962496910159 ) ) ;
#90837 = CARTESIAN_POINT ( 'NONE',  ( -102.6327255629189352, -292.5935519350809955, -230.7650273092966984 ) ) ;
#90838 = CARTESIAN_POINT ( 'NONE',  ( 25.22466315766300227, -296.6948066931273047, -320.2154176792147382 ) ) ;
#90839 = CARTESIAN_POINT ( 'NONE',  ( -69.58743246951203787, -287.6268861102293499, -202.8174215943278398 ) ) ;
#90840 = CARTESIAN_POINT ( 'NONE',  ( -43.15570500971156065, -287.6989405396924440, -346.5503799566787961 ) ) ;
#90841 = CARTESIAN_POINT ( 'NONE',  ( -46.37546007465596887, -271.9370851207518740, -196.0750519516181782 ) ) ;
#90842 = CARTESIAN_POINT ( 'NONE',  ( -62.53968889775161699, -275.6418600410761996, -200.3155930780314122 ) ) ;
#90843 = CARTESIAN_POINT ( 'NONE',  ( -96.93554681567800912, -288.0177496538732953, -314.9905557626221935 ) ) ;
#90844 = CARTESIAN_POINT ( 'NONE',  ( -112.0768018849169749, -280.2543386846155613, -282.8098145750989261 ) ) ;
#90845 = ORIENTED_EDGE ( 'NONE', *, *, #60850, .F. ) ;
#90847 = CARTESIAN_POINT ( 'NONE',  ( 11.37992084315340513, -280.0977708659839891, -215.8625279289563537 ) ) ;
#90846 = CARTESIAN_POINT ( 'NONE',  ( 15.25938121658180435, -280.8206030763413423, -219.6714554728410178 ) ) ;
#90848 = CARTESIAN_POINT ( 'NONE',  ( 39.32149395882056808, -276.6059440806427574, -268.3002489213911872 ) ) ;
#90849 = CARTESIAN_POINT ( 'NONE',  ( 8.322209442178680305, -279.4561546196263748, -208.7905692509054063 ) ) ;
#90850 = CARTESIAN_POINT ( 'NONE',  ( -90.35769054958068125, -228.8493742786694440, -345.0038117470676866 ) ) ;
#90851 = CARTESIAN_POINT ( 'NONE',  ( -2.674560634404023585, -275.4404502270335797, -201.8555152988813290 ) ) ;
#90852 = CARTESIAN_POINT ( 'NONE',  ( -94.57934650329326587, -274.7617333585757251, -219.8976699130175803 ) ) ;
#90853 = EDGE_CURVE ( 'NONE', #443, #31059, #45223, .T. ) ;
#90854 = CARTESIAN_POINT ( 'NONE',  ( -106.6662871844225293, -299.4805209788416391, -237.0123917617630980 ) ) ;
#90855 = ORIENTED_EDGE ( 'NONE', *, *, #89476, .F. ) ;
#90856 = CARTESIAN_POINT ( 'NONE',  ( 104.1717476309105166, -299.5541904835127980, -197.7570935515975350 ) ) ;
#90857 = CARTESIAN_POINT ( 'NONE',  ( 17.11104174832909663, -287.9317725444258258, -221.2595437054770002 ) ) ;
#90858 = CARTESIAN_POINT ( 'NONE',  ( 19.51344350397417315, -288.6195272223346819, -219.8705124428961142 ) ) ;
#90859 = CARTESIAN_POINT ( 'NONE',  ( -109.8916939146382816, -289.7826226818954183, -279.3272247022040347 ) ) ;
#90860 = CARTESIAN_POINT ( 'NONE',  ( -49.32894999990031693, -285.4110634945222387, -194.3085259379780325 ) ) ;
#90861 = CARTESIAN_POINT ( 'NONE',  ( 165.4284657918965991, 2.965303559109565334, -9.000000000000001776 ) ) ;
#90862 = CARTESIAN_POINT ( 'NONE',  ( -23.93999431430018987, -281.2779635836222383, -342.9340791629549585 ) ) ;
#90863 = CARTESIAN_POINT ( 'NONE',  ( 35.22304619055572772, -289.6164337645341220, -286.0804274914435155 ) ) ;
#90864 = CARTESIAN_POINT ( 'NONE',  ( -36.20204257885875165, -281.5174831966717193, -344.0456410188638188 ) ) ;
#90865 = CARTESIAN_POINT ( 'NONE',  ( -109.9769243189216468, -279.7206180160303006, -281.5578891740382801 ) ) ;
#90866 = CARTESIAN_POINT ( 'NONE',  ( 17.48555786604638485, -276.7336534365163061, -318.6703679497812800 ) ) ;
#90867 = CARTESIAN_POINT ( 'NONE',  ( -95.16869143061067859, -288.6645133080202754, -320.6010204133932007 ) ) ;
#90868 = CARTESIAN_POINT ( 'NONE',  ( -107.7822010621069495, -285.7486361629958651, -239.5312209689940630 ) ) ;
#90869 = CARTESIAN_POINT ( 'NONE',  ( -93.87878023363248303, -285.7562238965024335, -218.0998392268156181 ) ) ;
#90870 = CARTESIAN_POINT ( 'NONE',  ( 19.35338267844834803, -282.3696860666522070, -316.3663370656909706 ) ) ;
#90871 = ORIENTED_EDGE ( 'NONE', *, *, #25372, .F. ) ;
#90872 = CARTESIAN_POINT ( 'NONE',  ( 140.6539576904058606, 250.5000000000000568, -12.00000000000000000 ) ) ;
#90873 = CARTESIAN_POINT ( 'NONE',  ( -96.51397491429513309, -293.0566706825098322, -223.0436013349047926 ) ) ;
#90874 = CARTESIAN_POINT ( 'NONE',  ( -76.89984542897843767, -290.2192425981789370, -204.8137575633448932 ) ) ;
#90875 = CARTESIAN_POINT ( 'NONE',  ( 34.06585772786585409, -274.3964337372952969, -254.0455763294952476 ) ) ;
#90876 = EDGE_CURVE ( 'NONE', #35594, #38261, #67421, .T. ) ;
#90877 = CARTESIAN_POINT ( 'NONE',  ( -70.77106948570759926, -294.8300760074432105, -339.6272524197201506 ) ) ;
#90878 = CARTESIAN_POINT ( 'NONE',  ( -75.32048722799150653, -290.0161769980778672, -207.1484076620558596 ) ) ;
#90879 = CARTESIAN_POINT ( 'NONE',  ( -2.688886289797828510, -292.8271885715830081, -335.7610912881140166 ) ) ;
#90880 = CARTESIAN_POINT ( 'NONE',  ( -103.1949725731118548, -291.3204147236751282, -302.7721810921186147 ) ) ;
#90881 = CARTESIAN_POINT ( 'NONE',  ( 85.55100297371598117, -298.0521521680024080, -417.1172536214571096 ) ) ;
#90882 = CARTESIAN_POINT ( 'NONE',  ( -62.07930559428666584, -291.3738143728981527, -341.2189367471137302 ) ) ;
#90883 = CARTESIAN_POINT ( 'NONE',  ( 12.09238538302695964, -290.7376934807101634, -213.7369216224489605 ) ) ;
#90884 = CARTESIAN_POINT ( 'NONE',  ( -39.54149075581725725, -297.0799038051904972, -345.3415077715028474 ) ) ;
#90885 = CARTESIAN_POINT ( 'NONE',  ( -65.19377429677207658, -286.6204118655235220, -202.5747882988739832 ) ) ;
#90886 = CARTESIAN_POINT ( 'NONE',  ( -39.04025641984931383, -297.0735797031048264, -345.5085952295960965 ) ) ;
#90887 = CARTESIAN_POINT ( 'NONE',  ( 37.29158456131943922, -277.3990652573534135, -259.9553686505958581 ) ) ;
#90888 = CARTESIAN_POINT ( 'NONE',  ( -48.45164520234993688, -275.9853577955981905, -346.2077291237597478 ) ) ;
#90889 = CARTESIAN_POINT ( 'NONE',  ( -9.173577916030799528, -297.5935730249259450, -193.5263149346576199 ) ) ;
#90890 = CARTESIAN_POINT ( 'NONE',  ( 14.42427113825025131, -274.5522663346434911, -323.3310379801695831 ) ) ;
#90891 = CARTESIAN_POINT ( 'NONE',  ( -38.34925143423605931, -278.1192762904393589, -195.9152880886290973 ) ) ;
#90892 = CARTESIAN_POINT ( 'NONE',  ( -89.53526027299699308, -274.5011211024885256, -218.7572151846734698 ) ) ;
#90893 = EDGE_CURVE ( 'NONE', #59355, #83166, #50780, .T. ) ;
#90894 = CARTESIAN_POINT ( 'NONE',  ( -35.82159879687392845, -298.8744944963281682, -197.1994263732142656 ) ) ;
#90895 = CARTESIAN_POINT ( 'NONE',  ( 208.4306832106271088, -74.55766379199613425, 0.000000000000000000 ) ) ;
#90897 = CARTESIAN_POINT ( 'NONE',  ( 34.37389770579854087, -275.2056226547447864, -256.7275919583309474 ) ) ;
#90896 = CARTESIAN_POINT ( 'NONE',  ( -2.582332419602012319, -286.6148377780398278, -337.2206211381853223 ) ) ;
#90898 = CARTESIAN_POINT ( 'NONE',  ( 12.41582732293890246, -288.3809887253688089, -329.1249543273815448 ) ) ;
#90899 = CARTESIAN_POINT ( 'NONE',  ( -20.50516476239022978, -288.5084943617802082, -345.5308504021601834 ) ) ;
#90900 = CARTESIAN_POINT ( 'NONE',  ( -109.2230788738129519, -298.2411465925107450, -293.0200560701889003 ) ) ;
#90901 = CARTESIAN_POINT ( 'NONE',  ( 25.96493789897412086, -292.0908665092681531, -310.3620141877276524 ) ) ;
#90902 = CARTESIAN_POINT ( 'NONE',  ( 24.97033517346224940, -281.3469747147189537, -315.3430872376789011 ) ) ;
#90903 = CARTESIAN_POINT ( 'NONE',  ( 199.6150009768959990, 276.0000000000000568, -2.367926910627516257 ) ) ;
#90904 = CARTESIAN_POINT ( 'NONE',  ( -64.55037024555267067, -277.6969516674083707, -200.4157805965516559 ) ) ;
#90905 = CARTESIAN_POINT ( 'NONE',  ( 201.9220344434848755, 287.7612796304733251, -5.053264882194825169 ) ) ;
#90906 = CARTESIAN_POINT ( 'NONE',  ( -50.83946396662989287, -288.0232270138000104, -342.5583561058506348 ) ) ;
#90907 = DIRECTION ( 'NONE',  ( 0.000000000000000000, 0.000000000000000000, 1.000000000000000000 ) ) ;
#90908 = LINE ( 'NONE', #76284, #39699 ) ;
#90909 = CARTESIAN_POINT ( 'NONE',  ( -98.37445577226301907, -289.1458171220278928, -226.6842835789189223 ) ) ;
#90910 = CARTESIAN_POINT ( 'NONE',  ( 3.296293995157008716, -276.1289521222244616, -208.8244452752689710 ) ) ;
#90911 = CARTESIAN_POINT ( 'NONE',  ( 38.29064913625064293, -283.1145278293249703, -281.2401821678823239 ) ) ;
#90913 = CARTESIAN_POINT ( 'NONE',  ( -95.11644008230761926, -283.9236814554523107, -315.0030360031106511 ) ) ;
#90912 = CARTESIAN_POINT ( 'NONE',  ( -45.91712290401081731, -295.9640262681513150, -195.4954454363450509 ) ) ;
#90914 = CARTESIAN_POINT ( 'NONE',  ( 19.44203619691334595, -276.3193363431988132, -223.5531890834425042 ) ) ;
#90915 = CARTESIAN_POINT ( 'NONE',  ( 33.74585797779515417, -276.5833196329759289, -287.7101884586494975 ) ) ;
#90916 = CARTESIAN_POINT ( 'NONE',  ( 35.39151566224521872, -285.8940188409931693, -290.8827277049616669 ) ) ;
#90917 = CARTESIAN_POINT ( 'NONE',  ( -49.73721027179915666, -285.2102801604158344, -344.3821793724244458 ) ) ;
#90918 = CARTESIAN_POINT ( 'NONE',  ( -110.6503002674750462, -271.5085867383893969, -267.6120100036642953 ) ) ;
#90919 = ORIENTED_EDGE ( 'NONE', *, *, #84689, .T. ) ;
#90920 = CARTESIAN_POINT ( 'NONE',  ( 202.9738562182569694, 295.9636489450776367, -54.00000000004089173 ) ) ;
#90921 = CARTESIAN_POINT ( 'NONE',  ( 39.22636708985139364, -293.2775039075388577, -261.7280272684386659 ) ) ;
#90922 = CARTESIAN_POINT ( 'NONE',  ( -86.83518275965906241, -287.3399921341148229, -214.4149863381441889 ) ) ;
#90923 = DIRECTION ( 'NONE',  ( 0.000000000000000000, 0.000000000000000000, -1.000000000000000000 ) ) ;
#90924 = CARTESIAN_POINT ( 'NONE',  ( -99.86837403722181250, -282.6952119285918457, -220.4570493818173702 ) ) ;
#90925 = CARTESIAN_POINT ( 'NONE',  ( -65.04641470917056267, -276.6020875286535556, -342.0874201227497338 ) ) ;
#90926 = CARTESIAN_POINT ( 'NONE',  ( -84.68376105807472243, -288.0916404625320411, -330.1374955571340593 ) ) ;
#90927 = AXIS2_PLACEMENT_3D ( 'NONE', #31102, #81269, #15026 ) ;
#90928 = CARTESIAN_POINT ( 'NONE',  ( 3.793132658930512324, -284.0078407313470734, -331.5672188670558853 ) ) ;
#90929 = CARTESIAN_POINT ( 'NONE',  ( -37.79375931541365219, -278.8179959488529676, -344.3857002797081464 ) ) ;
#90930 = CARTESIAN_POINT ( 'NONE',  ( -85.71522420497031192, -285.1321412110997358, -329.5101539820667540 ) ) ;
#90931 = CARTESIAN_POINT ( 'NONE',  ( -42.97864262341066421, -281.9196614872113287, -343.5917704835240443 ) ) ;
#90932 = CARTESIAN_POINT ( 'NONE',  ( -35.64233728854296146, -282.0736016031649456, -195.3676253642103688 ) ) ;
#90933 = CARTESIAN_POINT ( 'NONE',  ( 13.96289506352593968, -274.9150602436251347, -212.8717651666284496 ) ) ;
#90934 = CARTESIAN_POINT ( 'NONE',  ( -42.80828766433214838, -276.9526666038566987, -347.1668236639632710 ) ) ;
#90935 = CARTESIAN_POINT ( 'NONE',  ( -20.49904834449667135, -296.7544872381379832, -342.9238354863966265 ) ) ;
#90936 = FACE_OUTER_BOUND ( 'NONE', #48140, .T. ) ;
#90937 = DIRECTION ( 'NONE',  ( -1.000000000000000000, 0.000000000000000000, 0.000000000000000000 ) ) ;
#90938 = B_SPLINE_CURVE_WITH_KNOTS ( 'NONE', 3,
 ( #80227, #52724, #67434, #1616, #16756, #1160, #36671, #30043 ),
 .UNSPECIFIED., .F., .F.,
 ( 4, 2, 2, 4 ),
 ( 0.000000000000000000, 0.0008414166960586483236, 0.001682833392117296647, 0.003365666784234650107 ),
 .UNSPECIFIED. ) ;
#90939 = CARTESIAN_POINT ( 'NONE',  ( -83.45253666998696929, -293.8158712047854806, -330.5446349255972223 ) ) ;
#90940 = CARTESIAN_POINT ( 'NONE',  ( 23.84846012060114617, -274.5070845725301183, -230.4392852291380791 ) ) ;
#90941 = CARTESIAN_POINT ( 'NONE',  ( -105.2640068955297323, -274.2177937244799182, -234.8265337162724222 ) ) ;
#90942 = CARTESIAN_POINT ( 'NONE',  ( 25.80374816565178264, -288.7876104632247234, -231.7524871848097519 ) ) ;
#90943 = CARTESIAN_POINT ( 'NONE',  ( -88.12940577804570808, -297.2675718264882789, -327.3820825954441034 ) ) ;
#90944 = CARTESIAN_POINT ( 'NONE',  ( -111.2050540018490210, -297.5015775282732307, -290.6641639078940216 ) ) ;
#90945 = CARTESIAN_POINT ( 'NONE',  ( -104.4792870326641179, -292.1153715076559934, -303.4152077143706379 ) ) ;
#90946 = CARTESIAN_POINT ( 'NONE',  ( 10.46688989592492902, -278.7133933244763284, -212.7230083858162288 ) ) ;
#90947 = CARTESIAN_POINT ( 'NONE',  ( -79.89773116671057096, -281.3916629014598243, -209.2849489982502007 ) ) ;
#90948 = CARTESIAN_POINT ( 'NONE',  ( -96.76839655048529210, -294.0142223202572609, -315.2127163558214420 ) ) ;
#90949 = CARTESIAN_POINT ( 'NONE',  ( -2.185909994324898520, -284.4522182847655358, -337.4757654372749585 ) ) ;
#90950 = CARTESIAN_POINT ( 'NONE',  ( 27.93963876518999001, -286.0198847891174978, -236.8938997667564195 ) ) ;
#90951 = CARTESIAN_POINT ( 'NONE',  ( 66.62391514549891269, 46.68937456676394504, -318.3441884561316328 ) ) ;
#90952 = VERTEX_POINT ( 'NONE', #38124 ) ;
#90953 = CARTESIAN_POINT ( 'NONE',  ( -99.62513603848654498, -284.7450927796080009, -232.1483733957276741 ) ) ;
#90954 = ORIENTED_EDGE ( 'NONE', *, *, #3216, .T. ) ;
#90955 = CARTESIAN_POINT ( 'NONE',  ( 26.01744633488269542, -282.0585456217152114, -227.0583995882606985 ) ) ;
#90956 = CARTESIAN_POINT ( 'NONE',  ( -96.30095538914154929, -273.4895104961962602, -227.1970191276514868 ) ) ;
#90957 = CARTESIAN_POINT ( 'NONE',  ( -36.55402132116073233, -284.8567619757328089, -193.7492668471912509 ) ) ;
#90958 = CARTESIAN_POINT ( 'NONE',  ( -25.44391599102797841, -281.1415039320959295, -194.5240363863448749 ) ) ;
#90959 = CARTESIAN_POINT ( 'NONE',  ( 0.000000000000000000, 0.000000000000000000, 0.000000000000000000 ) ) ;
#90960 = CARTESIAN_POINT ( 'NONE',  ( -73.45475546091442709, -281.1021299245235241, -203.1261023922344577 ) ) ;
#90961 = CARTESIAN_POINT ( 'NONE',  ( -3.670690328810089831, -280.8176344348310067, -201.1222776717011129 ) ) ;
#90962 = CARTESIAN_POINT ( 'NONE',  ( -37.30987171927208834, -289.5523547857346784, -200.3611179825600459 ) ) ;
#90963 = CARTESIAN_POINT ( 'NONE',  ( -107.0744119028121446, -263.0355450277866680, -317.7147900177194515 ) ) ;
#90964 = ORIENTED_EDGE ( 'NONE', *, *, #78083, .T. ) ;
#90965 = CARTESIAN_POINT ( 'NONE',  ( -90.56350721584459507, -275.2960776685794144, -217.7543914547774477 ) ) ;
#90966 = CARTESIAN_POINT ( 'NONE',  ( -56.85822679724589079, -169.0278465697174965, -364.1129473661134170 ) ) ;
#90967 = CARTESIAN_POINT ( 'NONE',  ( 12.42068220339687201, -278.7695057721749663, -214.7234319704571419 ) ) ;
#90968 = CARTESIAN_POINT ( 'NONE',  ( 36.43266382504649670, -295.0815434048254815, -252.1589961239934610 ) ) ;
#90969 = CARTESIAN_POINT ( 'NONE',  ( -75.71862088245707412, -294.9273395214373750, -332.6383384075426761 ) ) ;
#90970 = CARTESIAN_POINT ( 'NONE',  ( -13.87924978881762605, -291.8561594351979807, -197.0314506111629100 ) ) ;
#90971 = DIRECTION ( 'NONE',  ( -0.000000000000000000, 1.000000000000000000, -0.000000000000000000 ) ) ;
#90973 = CARTESIAN_POINT ( 'NONE',  ( 34.78212824373949985, -285.7479476038117241, -254.7216231532430868 ) ) ;
#90972 = CARTESIAN_POINT ( 'NONE',  ( -113.7772916893482460, -295.1007373478690852, -272.4355454230632745 ) ) ;
#90974 = CARTESIAN_POINT ( 'NONE',  ( 28.26054437331280411, -295.8792769279868935, -305.2159700821398474 ) ) ;
#90975 = CARTESIAN_POINT ( 'NONE',  ( -96.30746453854132483, -285.2561239612773534, -314.2277580023124415 ) ) ;
#90976 = VERTEX_POINT ( 'NONE', #31060 ) ;
#90977 = CARTESIAN_POINT ( 'NONE',  ( 36.14793964560384865, -294.7747314882244041, -292.7244531363716646 ) ) ;
#90978 = CARTESIAN_POINT ( 'NONE',  ( -37.53439365007844231, -283.5470123371905515, -343.4348423231849097 ) ) ;
#90979 = CARTESIAN_POINT ( 'NONE',  ( -101.3052182973872135, -294.7888971317916571, -312.6077246920299899 ) ) ;
#90980 = CARTESIAN_POINT ( 'NONE',  ( -108.2221289034982448, -291.7331115021885921, -240.6942402119126996 ) ) ;
#90981 = CARTESIAN_POINT ( 'NONE',  ( -110.3744728098186272, -291.3512578876907924, -245.9922651095259312 ) ) ;
#90982 = CARTESIAN_POINT ( 'NONE',  ( 27.03146753365539467, -288.1893873390139902, -304.8939219615119214 ) ) ;
#90983 = ORIENTED_EDGE ( 'NONE', *, *, #69967, .T. ) ;
#90984 = CARTESIAN_POINT ( 'NONE',  ( 212.3569123273291268, -147.7221692137691775, -10.75739200365177695 ) ) ;
#90985 = CARTESIAN_POINT ( 'NONE',  ( -73.98780908681760593, -297.3936101085948280, -336.7325192630561332 ) ) ;
#90986 = CARTESIAN_POINT ( 'NONE',  ( -27.03467378457320791, -272.9752015756983496, -194.4016130329067664 ) ) ;
#90987 = CARTESIAN_POINT ( 'NONE',  ( -46.47395240873320432, -278.9923007490727969, -197.6461717106695630 ) ) ;
#90988 = EDGE_LOOP ( 'NONE', ( #56296, #85674, #45945, #2147 ) ) ;
#90989 = CARTESIAN_POINT ( 'NONE',  ( 26.88264667651773365, -274.5022752184702313, -227.9965079793375935 ) ) ;
#90990 = CARTESIAN_POINT ( 'NONE',  ( -60.71765597359786426, -296.2233062917712232, -200.4195762110577448 ) ) ;
#90991 = CARTESIAN_POINT ( 'NONE',  ( -5.729471905000831811, -278.4924110004315025, -337.5430645637092084 ) ) ;
#90992 = CARTESIAN_POINT ( 'NONE',  ( -36.70202390154909011, -272.1998557082716843, -196.1160446736603546 ) ) ;
#90993 = CIRCLE ( 'NONE', #41046, 0.5000000000000068834 ) ;
#90994 = CARTESIAN_POINT ( 'NONE',  ( -84.72279142167131738, -296.9270242044190127, -326.4828334562519672 ) ) ;
#90995 = CARTESIAN_POINT ( 'NONE',  ( -44.61337079273804562, -299.0377937805861848, -197.3629462935431889 ) ) ;
#90996 = CARTESIAN_POINT ( 'NONE',  ( 221.8344101925596306, 0.000000000000000000, 7.000000000000000000 ) ) ;
#90997 = CARTESIAN_POINT ( 'NONE',  ( -51.67037220917357132, -299.4720675092139572, -195.4666458739050938 ) ) ;
#90998 = CIRCLE ( 'NONE', #72856, 0.5000000000000004441 ) ;
#90999 = CARTESIAN_POINT ( 'NONE',  ( -112.5377879941094932, -270.6443013071351515, -264.7236331678293482 ) ) ;
#91000 = CARTESIAN_POINT ( 'NONE',  ( 8.906924158677348657, -293.3572351563867073, -213.6831234149605336 ) ) ;
#91001 = CARTESIAN_POINT ( 'NONE',  ( -110.8961156397808736, -289.0803073707435260, -273.9194953613602479 ) ) ;
#91002 = DIRECTION ( 'NONE',  ( -0.000000000000000000, -0.000000000000000000, -1.000000000000000000 ) ) ;
#91003 = CARTESIAN_POINT ( 'NONE',  ( 37.88389657842101599, -275.8416498948889739, -254.1546182187037743 ) ) ;
#91004 = CARTESIAN_POINT ( 'NONE',  ( 8.941184956592957533, -298.9805435559529201, -197.3372685744649004 ) ) ;
#91005 = CIRCLE ( 'NONE', #80485, 4.003189038634634045 ) ;
#91006 = CARTESIAN_POINT ( 'NONE',  ( -76.65637301785764635, -281.5090867736279847, -206.0141283328111399 ) ) ;
#91007 = CARTESIAN_POINT ( 'NONE',  ( -61.09457678357784260, -282.0388957169064952, -343.1426432866175560 ) ) ;
#91008 = CARTESIAN_POINT ( 'NONE',  ( -28.62084665960789920, -276.2930346226852407, -346.8165820222291700 ) ) ;
#91009 = CARTESIAN_POINT ( 'NONE',  ( -108.1824613252785241, -283.9901089479374718, -252.0803007027579383 ) ) ;
#91010 = CARTESIAN_POINT ( 'NONE',  ( 36.61701703255067741, -279.7248558625624923, -283.8539762258984638 ) ) ;
#91011 = EDGE_CURVE ( 'NONE', #58102, #89245, #88787, .T. ) ;
#91012 = CARTESIAN_POINT ( 'NONE',  ( -21.79196610406816603, -272.8300934221427951, -198.4335107151910904 ) ) ;
#91013 = CARTESIAN_POINT ( 'NONE',  ( -43.25950329511469050, -279.1269158913100341, -345.1779740246709025 ) ) ;
#91014 = DIRECTION ( 'NONE',  ( 0.9849620900324523864, 0.000000000000000000, -0.1727706028203384037 ) ) ;
#91015 = DIRECTION ( 'NONE',  ( 0.000000000000000000, -1.000000000000000000, 0.000000000000000000 ) ) ;
#91016 = CARTESIAN_POINT ( 'NONE',  ( -43.18911350981500163, -296.2192791470083080, -194.5472608965895347 ) ) ;
#91017 = CARTESIAN_POINT ( 'NONE',  ( -45.42649278897774678, -279.1543904682803827, -345.1435258453242341 ) ) ;
#91018 = CARTESIAN_POINT ( 'NONE',  ( -110.9623265619114960, -286.6890812506171642, -253.3517803642619697 ) ) ;
#91019 = VERTEX_POINT ( 'NONE', #45691 ) ;
#91020 = CARTESIAN_POINT ( 'NONE',  ( 201.2849759805918382, 65.05171340438522520, 7.254661561168179951 ) ) ;
#91021 = CARTESIAN_POINT ( 'NONE',  ( 35.27335428891451841, -285.7936672454010250, -289.1747137788573241 ) ) ;
#91022 = DIRECTION ( 'NONE',  ( 0.000000000000000000, -1.000000000000000000, 0.000000000000000000 ) ) ;
#91023 = CARTESIAN_POINT ( 'NONE',  ( -63.72598563317177423, -294.1987284430902037, -338.9058479885759994 ) ) ;
#91024 = CARTESIAN_POINT ( 'NONE',  ( -20.87806073709151278, -286.9781783829336632, -342.7476778913273279 ) ) ;
#91025 = CARTESIAN_POINT ( 'NONE',  ( 5.045406874201050940, -57.93311274753654061, -355.0152878038887820 ) ) ;
#91026 = CARTESIAN_POINT ( 'NONE',  ( -101.9006828987354396, -294.0403003511833617, -308.6359176066416126 ) ) ;
#91027 = CARTESIAN_POINT ( 'NONE',  ( 19.78071763164805930, -285.3397938032260299, -219.6892490331134127 ) ) ;
#91028 = CARTESIAN_POINT ( 'NONE',  ( 36.31709171146466275, -283.0927441229456463, -265.7979175481778498 ) ) ;
#91029 = CARTESIAN_POINT ( 'NONE',  ( 34.64182307317286558, -280.1045315314523236, -294.8626598633476306 ) ) ;
#91030 = CARTESIAN_POINT ( 'NONE',  ( -42.66391403310464625, -289.1210224538163516, -343.2174499769024578 ) ) ;
#91031 = CARTESIAN_POINT ( 'NONE',  ( -19.40839153056193922, -281.7125310320872700, -198.9377478122382001 ) ) ;
#91032 = CARTESIAN_POINT ( 'NONE',  ( 31.21804926254937129, -282.0133906499681871, -244.6783577494234976 ) ) ;
#91033 = CARTESIAN_POINT ( 'NONE',  ( 24.18720744861784056, -288.9434811833316417, -226.8348540555814736 ) ) ;
#91034 = EDGE_LOOP ( 'NONE', ( #71937, #27824, #66460, #82524 ) ) ;
#91035 = CARTESIAN_POINT ( 'NONE',  ( -111.0371254260475951, -272.8343313104732033, -247.8632948686687598 ) ) ;
#91036 = CARTESIAN_POINT ( 'NONE',  ( -89.79945792042572350, -291.7768664939889618, -323.4650768636202542 ) ) ;
#91037 = DIRECTION ( 'NONE',  ( 0.000000000000000000, -1.000000000000000000, 0.000000000000000000 ) ) ;
#91038 = CARTESIAN_POINT ( 'NONE',  ( 25.18497378105907814, -289.4090924074130839, -220.4570493818173702 ) ) ;
#91039 = ORIENTED_EDGE ( 'NONE', *, *, #2612, .F. ) ;
#91040 = CARTESIAN_POINT ( 'NONE',  ( -2.344454827926801599, -274.5899576281215673, -336.8834544615656910 ) ) ;
#91041 = CARTESIAN_POINT ( 'NONE',  ( 183.0442525570908288, 264.6571197653884155, 7.500000000000000000 ) ) ;
#91042 = CARTESIAN_POINT ( 'NONE',  ( -66.63592358114750880, -293.8293853576281549, -340.7192490205051740 ) ) ;
#91043 = CARTESIAN_POINT ( 'NONE',  ( -41.86589471663139506, -297.5012553282984413, -197.4397897920632943 ) ) ;
#91044 = CARTESIAN_POINT ( 'NONE',  ( 20.06566681875769476, -289.7193814246786019, -316.5682816580791723 ) ) ;
#91045 = CARTESIAN_POINT ( 'NONE',  ( -23.85921338480430620, -284.6376923185221699, -343.1360900701230321 ) ) ;
#91046 = CARTESIAN_POINT ( 'NONE',  ( -110.6718409995223880, -292.2488860229383931, -248.8832984209662413 ) ) ;
#91047 = CARTESIAN_POINT ( 'NONE',  ( -108.3345838939889063, -291.5030512620212448, -298.8796860788661434 ) ) ;
#91048 = CARTESIAN_POINT ( 'NONE',  ( -49.77756589736652160, -287.8938299337074795, -196.3463920217268708 ) ) ;
#91049 = CARTESIAN_POINT ( 'NONE',  ( -91.05968924537954479, -279.4814748918863643, -215.1199673354214212 ) ) ;
#91050 = CARTESIAN_POINT ( 'NONE',  ( -102.5936827914308367, -295.1383954749189797, -232.1595972374336441 ) ) ;
#91051 = CARTESIAN_POINT ( 'NONE',  ( 21.60864494763040611, -282.0524715603884829, -319.8975371101256542 ) ) ;
#91052 = CARTESIAN_POINT ( 'NONE',  ( 31.43114174712345488, -277.7823219462227939, -298.4472752451638939 ) ) ;
#91053 = CARTESIAN_POINT ( 'NONE',  ( -109.1418805571601069, -281.0519495502701943, -270.3937649182068412 ) ) ;
#91054 = CARTESIAN_POINT ( 'NONE',  ( -34.36374767811492603, -275.1546732049775414, -346.0673745386463338 ) ) ;
#91056 = TOROIDAL_SURFACE ( 'NONE', #36623, 5.603083949679977138, 0.5000000000000000000 ) ;
#91055 = DIRECTION ( 'NONE',  ( 0.000000000000000000, 0.000000000000000000, 1.000000000000000000 ) ) ;
#91057 = CARTESIAN_POINT ( 'NONE',  ( 33.51680014956395581, -280.8244020716071532, -252.5040533427466585 ) ) ;
#91058 = AXIS2_PLACEMENT_3D ( 'NONE', #25499, #82789, #90800 ) ;
#91059 = CARTESIAN_POINT ( 'NONE',  ( -100.1311941326400756, -279.1741332383115832, -314.2415026836567904 ) ) ;
#91060 = CARTESIAN_POINT ( 'NONE',  ( -100.7952176068186390, -284.1834553710351656, -227.0645613887585057 ) ) ;
#91061 = CARTESIAN_POINT ( 'NONE',  ( 28.37615571674690429, -294.8556181682639021, -236.3150105082035282 ) ) ;
#91062 = CARTESIAN_POINT ( 'NONE',  ( 22.98685494044593369, -276.5242338031296754, -223.7898501736800085 ) ) ;
#91063 = EDGE_CURVE ( 'NONE', #70513, #87609, #45206, .T. ) ;
#91064 = MECHANICAL_DESIGN_GEOMETRIC_PRESENTATION_REPRESENTATION (  '', ( #83513 ), #62396 ) ;
#91065 = CARTESIAN_POINT ( 'NONE',  ( 35.25665166065600431, -276.5595717540737724, -246.0534453020507044 ) ) ;
#91066 = CARTESIAN_POINT ( 'NONE',  ( 200.4816938276917995, 61.72811464988816965, 9.999999999999998224 ) ) ;
#91068 = EDGE_CURVE ( 'NONE', #54877, #26035, #41640, .T. ) ;
#91067 = CARTESIAN_POINT ( 'NONE',  ( 15.59641786974552602, -276.1100503125019259, -320.6259731733720173 ) ) ;
#91069 = CARTESIAN_POINT ( 'NONE',  ( -105.3962054462466682, -298.9631972037566356, -239.1137557168918875 ) ) ;
#91070 = CARTESIAN_POINT ( 'NONE',  ( -111.6973325211808827, -282.4375830948256976, -279.2514923850187074 ) ) ;
#91071 = CIRCLE ( 'NONE', #77529, 4.999999999999986677 ) ;
#91072 = CARTESIAN_POINT ( 'NONE',  ( 38.30524771211417345, -293.0405107081077176, -256.1033631084205808 ) ) ;
#91073 = CARTESIAN_POINT ( 'NONE',  ( -34.67420589349448790, -290.6192782274403612, -346.5144166086029145 ) ) ;
#91074 = CARTESIAN_POINT ( 'NONE',  ( 33.61083317389190483, -292.2300831402139920, -251.9230027739928346 ) ) ;
#91075 = ORIENTED_EDGE ( 'NONE', *, *, #38515, .F. ) ;
#91076 = CARTESIAN_POINT ( 'NONE',  ( -34.96045181805560276, -290.6562108069092574, -193.9744086591702512 ) ) ;
#91077 = CARTESIAN_POINT ( 'NONE',  ( 32.65056747212670274, -292.9414288816075214, -249.3741081516795077 ) ) ;
#91078 = ORIENTED_EDGE ( 'NONE', *, *, #90766, .F. ) ;
#91079 = CARTESIAN_POINT ( 'NONE',  ( -80.35582246825275377, -290.6993753544941796, -333.9176085439250983 ) ) ;
#91080 = CARTESIAN_POINT ( 'NONE',  ( -98.01354234815093491, -279.4507005038909142, -229.6386417458874689 ) ) ;
#91081 = CARTESIAN_POINT ( 'NONE',  ( -8.517028216829702458, -293.6040592334197186, -341.4851578888133190 ) ) ;
#91082 = CARTESIAN_POINT ( 'NONE',  ( -69.75743829522463102, -286.2879006786095033, -200.6149081534760796 ) ) ;
#91083 = CARTESIAN_POINT ( 'NONE',  ( 39.07011525867798696, -288.0074677189782051, -280.1162930545701784 ) ) ;
#91084 = CARTESIAN_POINT ( 'NONE',  ( -56.32030779146403887, -283.6368112949385818, -340.8728186984362196 ) ) ;
#91085 = CARTESIAN_POINT ( 'NONE',  ( -39.92122854846482483, -139.4860003333291445, -364.6914301237072777 ) ) ;
#91086 = CARTESIAN_POINT ( 'NONE',  ( -79.00533470335423658, -207.5829368166174334, -355.8876102332309301 ) ) ;
#91087 = CARTESIAN_POINT ( 'NONE',  ( 197.8626310074445200, 286.4972087208413427, -96.32890240008197225 ) ) ;
#91088 = CARTESIAN_POINT ( 'NONE',  ( 23.19167250009359549, -274.1789077803798591, -229.2495619357918315 ) ) ;
#91089 = CARTESIAN_POINT ( 'NONE',  ( -41.88943974837088291, -276.0310939175988665, -343.5416851109322920 ) ) ;
#91090 = CARTESIAN_POINT ( 'NONE',  ( -114.1727638941521263, -295.9976242917600757, -275.3291459829642349 ) ) ;
#91091 = CARTESIAN_POINT ( 'NONE',  ( -110.3257646060037445, -272.4678080593321852, -270.3600440800341289 ) ) ;
#91092 = CARTESIAN_POINT ( 'NONE',  ( 31.40475345457193512, -274.6722214393019499, -304.0558796073630106 ) ) ;
#91093 = CARTESIAN_POINT ( 'NONE',  ( -31.27873901767373610, -275.8898888938586538, -196.5837043736565022 ) ) ;
#91094 = ORIENTED_EDGE ( 'NONE', *, *, #61391, .T. ) ;
#91095 = CARTESIAN_POINT ( 'NONE',  ( -92.95750875811738467, -274.3565290613117327, -217.5368902609039310 ) ) ;
#91096 =( BOUNDED_SURFACE ( )  B_SPLINE_SURFACE ( 3, 2, ( 
 ( #72588, #7710, #87239 ),
 ( #22386, #51258, #41938 ),
 ( #84557, #37064, #29964 ),
 ( #70850, #92131, #12618 ),
 ( #41464, #5523, #34393 ),
 ( #63300, #27286, #45068 ),
 ( #38897, #39821, #53111 ),
 ( #1535, #61187, #30420 ),
 ( #25177, #53598, #73968 ),
 ( #82470, #30899, #16670 ),
 ( #18075, #32281, #37962 ),
 ( #2005, #90024, #17617 ),
 ( #59790, #88631, #45525 ),
 ( #81990, #66869, #54051 ),
 ( #59311, #9082, #74427 ),
 ( #31815, #23778, #31359 ) ),
 .UNSPECIFIED., .F., .F., .F. ) 
 B_SPLINE_SURFACE_WITH_KNOTS ( ( 4, 2, 2, 2, 2, 2, 2, 4 ),
 ( 3, 3 ),
 ( 5.128070023563283009, 5.416848844467358148, 5.561238254919396162, 5.705627665371434176, 5.850017075823472190, 5.994406486275510204, 6.138795896727548218, 6.283185307179586232 ),
 ( 0.000000000000000000, 1.000000000000000000 ),
 .UNSPECIFIED. ) 
 GEOMETRIC_REPRESENTATION_ITEM ( )  RATIONAL_B_SPLINE_SURFACE ( (
 ( 1.000000000000000000, 0.9583671019092242505, 1.000000000000000000),
 ( 1.000000000000000000, 0.9398658125638100769, 1.000000000000000000),
 ( 1.000000000000000000, 0.9157002655843566874, 1.000000000000000000),
 ( 1.000000000000000000, 0.8756259400453313413, 1.000000000000000000),
 ( 1.000000000000000000, 0.8616433317033089789, 1.000000000000000000),
 ( 1.000000000000000000, 0.8334785261034494130, 1.000000000000000000),
 ( 1.000000000000000000, 0.8192978668688222221, 1.000000000000000000),
 ( 1.000000000000000000, 0.7919708659745230417, 1.000000000000000000),
 ( 1.000000000000000000, 0.7788285231915303974, 1.000000000000000000),
 ( 1.000000000000000000, 0.7549177526733705790, 1.000000000000000000),
 ( 1.000000000000000000, 0.7441566529437987354, 1.000000000000000000),
 ( 1.000000000000000000, 0.7262859251462959742, 1.000000000000000000),
 ( 1.000000000000000000, 0.7191857644035468677, 1.000000000000000000),
 ( 1.000000000000000000, 0.7095926089624788879, 1.000000000000000000),
 ( 1.000000000000000000, 0.7070960980132534601, 1.000000000000000000),
 ( 1.000000000000000000, 0.7071067811865473507, 1.000000000000000000) ) ) 
 REPRESENTATION_ITEM ( '' )  SURFACE ( )  );
#91097 = CARTESIAN_POINT ( 'NONE',  ( 32.33038704787760764, -287.7526768366848273, -248.3240480478373229 ) ) ;
#91098 = AXIS2_PLACEMENT_3D ( 'NONE', #52178, #81060, #24700 ) ;
#91099 = CARTESIAN_POINT ( 'NONE',  ( -61.53101358248718356, -296.1612786942654338, -343.3484580988664447 ) ) ;
#91100 = CARTESIAN_POINT ( 'NONE',  ( -111.5310139230105619, -296.7889641599716697, -290.7442635200258110 ) ) ;
#91101 = CARTESIAN_POINT ( 'NONE',  ( -72.12270919521363055, -295.6924067306260326, -334.5570150915633576 ) ) ;
#91102 = ORIENTED_EDGE ( 'NONE', *, *, #9083, .T. ) ;
#91103 =( BOUNDED_SURFACE ( )  B_SPLINE_SURFACE ( 3, 2, ( 
 ( #49243, #78138, #76718, #71029, #51096, #36896, #93714, #7546, #71503, #51547, #43075, #86143, #79983, #14214, #86603, #87528, #65813, #923, #35969, #44451, #79537, #42588, #36430, #92784, #35516, #64889, #43982, #73358, #7098, #72429, #50649, #29339, #15581, #29803, #28869, #8005, #15120, #49700, #21772, #58684, #87077, #20831, #27953, #71979, #22675, #14676, #85684, #56843, #43532, #57757, #80436, #65346, #22226, #78596, #453, #35032, #13738, #58233, #63946, #6635, #72880, #64430, #93256, #28410, #57301, #21293, #50166, #79063, #15649, #30795, #81426, #22289, #50710, #51613, #80047, #15187, #36034, #8990, #80501, #65876, #44047, #51160, #72043, #8075, #88057, #72948, #985, #37869, #58295, #73423, #44519, #36963, #57819, #29866, #8533, #7159, #23214, #37412, #58751, #14738, #64951, #79597, #87593, #87138, #22739, #21835, #66321, #7605, #1436, #30321, #52550, #66774, #59211, #1905, #43593, #52094, #72489, #80978, #36493, #16121, #520, #43139, #44972 ),
 ( #73873, #59694, #88537, #23686, #52, #28933, #86670, #65410, #29404, #24137, #17979, #74331, #17045, #17523, #25537, #25999, #82373, #53959, #32184, #10857, #90838, #76210, #46373, #83289, #32661, #31264, #68172, #11339, #68644, #2386, #9455, #89451, #47292, #61088, #67254, #38341, #89929, #10392, #40191, #25085, #3776, #60151, #82826, #69110, #88990, #24609, #4235, #62003, #39257, #3293, #53015, #75733, #90382, #39720, #9932, #18435, #45911, #75273, #81892, #74817, #60613, #54418, #38806, #67710, #33115, #2840, #46831, #54884, #16575, #31722, #45430, #53497, #34530, #27424, #40651, #70987, #20789, #26486, #48713, #48241, #34989, #85179, #18919, #91324, #11800, #56314, #71458, #28367, #62967, #55376, #92267, #26952, #55841, #76673, #49661, #20329, #12766, #84696, #91801, #47773, #77617, #63906, #19843, #41608, #78556, #5191, #49199, #78094, #70530, #4698, #5655, #13236, #69570, #92741, #42072, #63438, #84228, #33575, #19375, #6119, #34065, #27912, #62484 ),
 ( #93215, #13693, #56799, #42545, #77143, #85641, #12274, #6594, #41117, #35471, #70049, #83763, #64389, #43490, #50120, #72386, #28831, #14632, #50604, #58190, #8881, #21729, #16014, #65301, #66214, #87032, #37308, #51978, #1794, #15078, #72835, #57258, #79496, #58641, #407, #80393, #15537, #7058, #86102, #44410, #21251, #35928, #7503, #79017, #14170, #43034, #881, #71936, #36388, #29295, #80867, #64846, #22184, #93673, #73317, #22633, #57714, #7961, #30212, #51052, #86559, #79940, #43938, #36856, #65772, #29761, #87483, #8429, #51505, #1330, #59103, #87944, #23095, #44866, #73769, #37761, #66666, #45321, #59579, #81783, #60505, #2734, #3188, #16933, #89340, #39607, #75168, #68063, #81320, #17872, #61448, #67141, #24495, #88882, #75627, #32072, #88430, #38228, #52446, #60969, #18331, #69003, #9826, #2275, #39151, #67606, #31614, #23579, #90279, #89820, #53376, #82262, #38699, #16467, #17415, #10750, #46264, #10281, #25430, #45794, #24981, #53855, #82720 ),
 ( #74224, #46724, #9343, #60044, #74705, #68531, #3668, #24030, #54308, #83183, #32556, #47187, #76099, #31158, #52906, #11232, #40086, #30679, #33464, #63325, #12647, #25889, #63792, #20209, #6006, #62857, #70422, #40544, #20679, #12163, #55266, #49087, #77032, #55730, #56685, #34881, #92621, #5071, #13581, #48600, #11693, #5548, #61896, #4591, #33953, #13126, #42433, #69929, #41492, #19732, #92156, #78445, #27792, #91690, #70875, #77985, #18812, #84582, #85532, #56199, #83648, #90730, #41006, #49550, #77500, #54771, #47669, #69459, #26842, #19271, #34418, #76570, #48129, #62367, #27313, #85058, #4134, #33005, #41962, #91210, #26378, #84121, #71823, #88659, #78899, #52671, #28714, #71343, #74455, #58878, #64273, #87724, #42909, #22875, #64729, #73549, #24265, #35815, #31387, #80633, #81552, #8658, #16700, #67380, #17177, #30448, #88192, #6473, #93556, #73997, #15789, #2038, #30928, #21136, #35351, #59818, #93102, #50006, #51740, #28257, #57145, #85986, #16245 ),
 ( #14046, #44648, #6942, #23808, #37990, #37536, #23352, #45555, #66447, #1565, #59340, #52219, #81102, #45095, #9114, #66898, #9588, #38476, #2510, #60277, #89114, #53140, #82020, #83408, #2960, #33235, #76801, #82499, #10979, #10515, #90962, #47427, #74946, #53629, #67835, #18560, #33706, #84349, #25205, #17647, #54540, #82948, #18102, #38926, #11927, #76337, #68772, #46955, #54078, #10056, #39849, #26126, #75857, #3901, #40776, #61218, #11463, #40314, #32778, #60735, #61666, #69229, #31846, #55022, #4358, #90498, #46498, #89575, #39384, #25658, #91458, #68299, #4823, #62131, #83892, #19043, #47899, #69694, #46041, #62618, #26609, #24747, #3420, #55500, #75401, #32315, #90052, #63091, #19498, #6720, #77268, #91919, #63560, #41243, #70185, #57833, #56920, #34187, #92387, #12894, #43155, #12397, #34648, #5319, #42667, #78674, #27074, #64027, #86221, #78214, #48365, #55960, #20452, #77743, #84814, #19964, #70646, #49319, #85303, #85759, #5774, #13353, #28485 ),
 ( #27547, #13815, #48837, #41732, #79146, #35593, #7174, #56440, #42194, #71107, #36048, #6239, #35108, #72057, #64966, #92868, #28031, #20909, #68, #49778, #71583, #64508, #28947, #93334, #57379, #21371, #50241, #14295, #73886, #1917, #79611, #29420, #73436, #65890, #36508, #38354, #15202, #7622, #88071, #72503, #22303, #44061, #23227, #22754, #51174, #52562, #81441, #52108, #80514, #9469, #87154, #80061, #1449, #65423, #87607, #72962, #80991, #30335, #14752, #16589, #9003, #88551, #51628, #59225, #58310, #67268, #1002, #8090, #86685, #23698, #36978, #43607, #29882, #58765, #15665, #44533, #8546, #2399, #37426, #45444, #66336, #30809, #16133, #66787, #74345, #31279, #44985, #37882, #21851, #59708, #50726, #535, #83304, #18450, #9947, #60164, #47309, #24150, #38819, #10407, #81906, #17059, #4715, #3793, #74834, #39271, #53511, #83779, #53029, #75287, #45924, #76224, #25552, #67725, #10871, #33130, #25100, #89003, #2854, #61104, #24626, #31736, #60627 ),
 ( #17537, #89943, #69124, #39734, #32675, #89465, #11355, #90854, #82389, #53973, #46388, #40208, #61562, #68188, #3309, #32198, #90394, #47789, #82841, #17994, #46847, #68657, #75748, #54432, #4251, #26018, #62019, #54901, #18934, #76691, #11816, #40668, #69586, #63452, #85195, #28383, #48731, #63921, #6134, #27439, #48258, #12785, #35005, #62502, #13708, #71003, #56332, #5209, #26502, #41135, #34544, #77635, #78111, #12290, #41626, #91817, #92759, #20805, #43049, #57274, #13251, #86117, #34082, #92283, #62985, #49674, #70068, #42560, #84713, #27926, #70546, #56815, #85657, #77160, #33594, #78570, #91340, #26969, #5669, #84244, #19394, #71953, #71477, #55860, #20344, #19861, #21266, #49215, #42086, #6609, #35489, #64403, #93230, #50137, #79036, #14188, #45341, #7072, #7980, #65319, #21746, #35944, #58207, #36874, #72853, #73335, #87052, #65789, #16033, #51524, #44429, #57730, #87963, #37779, #43506, #898, #426, #51999, #8446, #64862, #14650, #28846, #37325 ) ),
 .UNSPECIFIED., .T., .F., .T. ) 
 B_SPLINE_SURFACE_WITH_KNOTS ( ( 4, 3, 4 ),
 ( 3, 2, 2, 2, 2, 2, 2, 2, 2, 2, 2, 2, 2, 2, 2, 2, 2, 2, 2, 2, 2, 2, 2, 2, 2, 2, 2, 2, 2, 2, 2, 2, 2, 2, 2, 2, 2, 2, 2, 2, 2, 2, 2, 2, 2, 2, 2, 2, 2, 2, 2, 2, 2, 2, 2, 2, 2, 2, 2, 2, 2, 3 ),
 ( 0.000000000000000000, 0.5000000000000000000, 1.000000000000000000 ),
 ( -0.05855608392607185297, 0.000000000000000000, 0.01428571428571428527, 0.02857142857142857054, 0.04285714285714285754, 0.05714285714285714107, 0.07142857142857142461, 0.08571428571428571508, 0.1000000000000000056, 0.1142857142857142821, 0.1285714285714285587, 0.1428571428571428492, 0.1571428571428571397, 0.1714285714285714302, 0.1857142857142857206, 0.2000000000000000111, 0.2142857142857142738, 0.2285714285714285643, 0.2428571428571428548, 0.2571428571428571175, 0.2714285714285714080, 0.2857142857142856984, 0.2999999999999999889, 0.3142857142857142794, 0.3285714285714285698, 0.3428571428571428603, 0.3571428571428571508, 0.3714285714285714413, 0.3857142857142857317, 0.4000000000000000222, 0.4142857142857143127, 0.4285714285714285476, 0.4428571428571428381, 0.4571428571428571286, 0.4714285714285714191, 0.4857142857142857095, 0.5000000000000000000, 0.5142857142857142350, 0.5285714285714285809, 0.5428571428571428159, 0.5571428571428571619, 0.5714285714285713969, 0.5857142857142857428, 0.5999999999999999778, 0.6142857142857143238, 0.6285714285714285587, 0.6428571428571429047, 0.6571428571428571397, 0.6714285714285713746, 0.6857142857142857206, 0.6999999999999999556, 0.7142857142857143016, 0.7285714285714285365, 0.7428571428571428825, 0.7571428571428571175, 0.7714285714285714635, 0.7857142857142856984, 0.8000000000000000444, 0.8142857142857142794, 0.8285714285714286254, 0.8428571428571428603, 0.8500000000000000888 ),
 .UNSPECIFIED. ) 
 GEOMETRIC_REPRESENTATION_ITEM ( )  RATIONAL_B_SPLINE_SURFACE ( (
 ( 1.000000000000000000, 1.000000000000000000, 1.000000000000000000, 0.9749279121818236193, 1.000000000000000000, 0.9749279121818236193, 1.000000000000000000, 0.9749279121818236193, 1.000000000000000000, 0.9749279121818236193, 1.000000000000000000, 0.9749279121818236193, 1.000000000000000000, 0.9749279121818236193, 1.000000000000000000, 0.9749279121818236193, 1.000000000000000000, 0.9749279121818236193, 1.000000000000000000, 0.9749279121818236193, 1.000000000000000000, 0.9749279121818236193, 1.000000000000000000, 0.9749279121818236193, 1.000000000000000000, 0.9749279121818236193, 1.000000000000000000, 0.9749279121818236193, 1.000000000000000000, 0.9749279121818236193, 1.000000000000000000, 0.9749279121818236193, 1.000000000000000000, 0.9749279121818236193, 1.000000000000000000, 0.9749279121818236193, 1.000000000000000000, 0.9749279121818236193, 1.000000000000000000, 0.9749279121818236193, 1.000000000000000000, 0.9749279121818236193, 1.000000000000000000, 0.9749279121818236193, 1.000000000000000000, 0.9749279121818236193, 1.000000000000000000, 0.9749279121818236193, 1.000000000000000000, 0.9749279121818236193, 1.000000000000000000, 0.9749279121818236193, 1.000000000000000000, 0.9749279121818236193, 1.000000000000000000, 0.9749279121818236193, 1.000000000000000000, 0.9749279121818236193, 1.000000000000000000, 0.9749279121818236193, 1.000000000000000000, 0.9749279121818236193, 1.000000000000000000, 0.9749279121818236193, 1.000000000000000000, 0.9749279121818236193, 1.000000000000000000, 0.9749279121818236193, 1.000000000000000000, 0.9749279121818236193, 1.000000000000000000, 0.9749279121818236193, 1.000000000000000000, 0.9749279121818236193, 1.000000000000000000, 0.9749279121818236193, 1.000000000000000000, 0.9749279121818236193, 1.000000000000000000, 0.9749279121818236193, 1.000000000000000000, 0.9749279121818236193, 1.000000000000000000, 0.9749279121818236193, 1.000000000000000000, 0.9749279121818236193, 1.000000000000000000, 0.9749279121818236193, 1.000000000000000000, 0.9749279121818236193, 1.000000000000000000, 0.9749279121818236193, 1.000000000000000000, 0.9749279121818236193, 1.000000000000000000, 0.9749279121818236193, 1.000000000000000000, 0.9749279121818236193, 1.000000000000000000, 0.9749279121818236193, 1.000000000000000000, 0.9749279121818236193, 1.000000000000000000, 0.9749279121818236193, 1.000000000000000000, 0.9749279121818236193, 1.000000000000000000, 0.9749279121818236193, 1.000000000000000000, 0.9749279121818236193, 1.000000000000000000, 0.9749279121818236193, 1.000000000000000000, 0.9749279121818236193, 1.000000000000000000, 0.9749279121818236193, 1.000000000000000000, 0.9749279121818236193, 1.000000000000000000, 0.9749279121818236193, 1.000000000000000000, 0.9874639560909115321, 0.9874639560909117542),
 ( 0.3333333333333333703, 0.3333333333333333703, 0.3333333333333333703, 0.3249759707272745768, 0.3333333333333333703, 0.3249759707272745768, 0.3333333333333333703, 0.3249759707272745768, 0.3333333333333333703, 0.3249759707272745768, 0.3333333333333333703, 0.3249759707272745768, 0.3333333333333333703, 0.3249759707272745768, 0.3333333333333333703, 0.3249759707272745768, 0.3333333333333333703, 0.3249759707272745768, 0.3333333333333333703, 0.3249759707272745768, 0.3333333333333333703, 0.3249759707272745768, 0.3333333333333333703, 0.3249759707272745768, 0.3333333333333333703, 0.3249759707272745768, 0.3333333333333333703, 0.3249759707272745768, 0.3333333333333333703, 0.3249759707272745768, 0.3333333333333333703, 0.3249759707272745768, 0.3333333333333333703, 0.3249759707272745768, 0.3333333333333333703, 0.3249759707272745768, 0.3333333333333333703, 0.3249759707272745768, 0.3333333333333333703, 0.3249759707272745768, 0.3333333333333333703, 0.3249759707272745768, 0.3333333333333333703, 0.3249759707272745768, 0.3333333333333333703, 0.3249759707272745768, 0.3333333333333333703, 0.3249759707272745768, 0.3333333333333333703, 0.3249759707272745768, 0.3333333333333333703, 0.3249759707272745768, 0.3333333333333333703, 0.3249759707272745768, 0.3333333333333333703, 0.3249759707272745768, 0.3333333333333333703, 0.3249759707272745768, 0.3333333333333333703, 0.3249759707272745768, 0.3333333333333333703, 0.3249759707272745768, 0.3333333333333333703, 0.3249759707272745768, 0.3333333333333333703, 0.3249759707272745768, 0.3333333333333333703, 0.3249759707272745768, 0.3333333333333333703, 0.3249759707272745768, 0.3333333333333333703, 0.3249759707272745768, 0.3333333333333333703, 0.3249759707272745768, 0.3333333333333333703, 0.3249759707272745768, 0.3333333333333333703, 0.3249759707272745768, 0.3333333333333333703, 0.3249759707272745768, 0.3333333333333333703, 0.3249759707272745768, 0.3333333333333333703, 0.3249759707272745768, 0.3333333333333333703, 0.3249759707272745768, 0.3333333333333333703, 0.3249759707272745768, 0.3333333333333333703, 0.3249759707272745768, 0.3333333333333333703, 0.3249759707272745768, 0.3333333333333333703, 0.3249759707272745768, 0.3333333333333333703, 0.3249759707272745768, 0.3333333333333333703, 0.3249759707272745768, 0.3333333333333333703, 0.3249759707272745768, 0.3333333333333333703, 0.3249759707272745768, 0.3333333333333333703, 0.3249759707272745768, 0.3333333333333333703, 0.3249759707272745768, 0.3333333333333333703, 0.3249759707272745768, 0.3333333333333333703, 0.3249759707272745768, 0.3333333333333333703, 0.3249759707272745768, 0.3333333333333333703, 0.3249759707272745768, 0.3333333333333333703, 0.3249759707272745768, 0.3333333333333333703, 0.3249759707272745768, 0.3333333333333333703, 0.3249759707272745768, 0.3333333333333333703, 0.3291546520303039181, 0.3291546520303039736),
 ( 0.3333333333333333703, 0.3333333333333333703, 0.3333333333333333703, 0.3249759707272745768, 0.3333333333333333703, 0.3249759707272745768, 0.3333333333333333703, 0.3249759707272745768, 0.3333333333333333703, 0.3249759707272745768, 0.3333333333333333703, 0.3249759707272745768, 0.3333333333333333703, 0.3249759707272745768, 0.3333333333333333703, 0.3249759707272745768, 0.3333333333333333703, 0.3249759707272745768, 0.3333333333333333703, 0.3249759707272745768, 0.3333333333333333703, 0.3249759707272745768, 0.3333333333333333703, 0.3249759707272745768, 0.3333333333333333703, 0.3249759707272745768, 0.3333333333333333703, 0.3249759707272745768, 0.3333333333333333703, 0.3249759707272745768, 0.3333333333333333703, 0.3249759707272745768, 0.3333333333333333703, 0.3249759707272745768, 0.3333333333333333703, 0.3249759707272745768, 0.3333333333333333703, 0.3249759707272745768, 0.3333333333333333703, 0.3249759707272745768, 0.3333333333333333703, 0.3249759707272745768, 0.3333333333333333703, 0.3249759707272745768, 0.3333333333333333703, 0.3249759707272745768, 0.3333333333333333703, 0.3249759707272745768, 0.3333333333333333703, 0.3249759707272745768, 0.3333333333333333703, 0.3249759707272745768, 0.3333333333333333703, 0.3249759707272745768, 0.3333333333333333703, 0.3249759707272745768, 0.3333333333333333703, 0.3249759707272745768, 0.3333333333333333703, 0.3249759707272745768, 0.3333333333333333703, 0.3249759707272745768, 0.3333333333333333703, 0.3249759707272745768, 0.3333333333333333703, 0.3249759707272745768, 0.3333333333333333703, 0.3249759707272745768, 0.3333333333333333703, 0.3249759707272745768, 0.3333333333333333703, 0.3249759707272745768, 0.3333333333333333703, 0.3249759707272745768, 0.3333333333333333703, 0.3249759707272745768, 0.3333333333333333703, 0.3249759707272745768, 0.3333333333333333703, 0.3249759707272745768, 0.3333333333333333703, 0.3249759707272745768, 0.3333333333333333703, 0.3249759707272745768, 0.3333333333333333703, 0.3249759707272745768, 0.3333333333333333703, 0.3249759707272745768, 0.3333333333333333703, 0.3249759707272745768, 0.3333333333333333703, 0.3249759707272745768, 0.3333333333333333703, 0.3249759707272745768, 0.3333333333333333703, 0.3249759707272745768, 0.3333333333333333703, 0.3249759707272745768, 0.3333333333333333703, 0.3249759707272745768, 0.3333333333333333703, 0.3249759707272745768, 0.3333333333333333703, 0.3249759707272745768, 0.3333333333333333703, 0.3249759707272745768, 0.3333333333333333703, 0.3249759707272745768, 0.3333333333333333703, 0.3249759707272745768, 0.3333333333333333703, 0.3249759707272745768, 0.3333333333333333703, 0.3249759707272745768, 0.3333333333333333703, 0.3249759707272745768, 0.3333333333333333703, 0.3249759707272745768, 0.3333333333333333703, 0.3249759707272745768, 0.3333333333333333703, 0.3291546520303039181, 0.3291546520303039736),
 ( 1.000000000000000000, 1.000000000000000000, 1.000000000000000000, 0.9749279121818236193, 1.000000000000000000, 0.9749279121818236193, 1.000000000000000000, 0.9749279121818236193, 1.000000000000000000, 0.9749279121818236193, 1.000000000000000000, 0.9749279121818236193, 1.000000000000000000, 0.9749279121818236193, 1.000000000000000000, 0.9749279121818236193, 1.000000000000000000, 0.9749279121818236193, 1.000000000000000000, 0.9749279121818236193, 1.000000000000000000, 0.9749279121818236193, 1.000000000000000000, 0.9749279121818236193, 1.000000000000000000, 0.9749279121818236193, 1.000000000000000000, 0.9749279121818236193, 1.000000000000000000, 0.9749279121818236193, 1.000000000000000000, 0.9749279121818236193, 1.000000000000000000, 0.9749279121818236193, 1.000000000000000000, 0.9749279121818236193, 1.000000000000000000, 0.9749279121818236193, 1.000000000000000000, 0.9749279121818236193, 1.000000000000000000, 0.9749279121818236193, 1.000000000000000000, 0.9749279121818236193, 1.000000000000000000, 0.9749279121818236193, 1.000000000000000000, 0.9749279121818236193, 1.000000000000000000, 0.9749279121818236193, 1.000000000000000000, 0.9749279121818236193, 1.000000000000000000, 0.9749279121818236193, 1.000000000000000000, 0.9749279121818236193, 1.000000000000000000, 0.9749279121818236193, 1.000000000000000000, 0.9749279121818236193, 1.000000000000000000, 0.9749279121818236193, 1.000000000000000000, 0.9749279121818236193, 1.000000000000000000, 0.9749279121818236193, 1.000000000000000000, 0.9749279121818236193, 1.000000000000000000, 0.9749279121818236193, 1.000000000000000000, 0.9749279121818236193, 1.000000000000000000, 0.9749279121818236193, 1.000000000000000000, 0.9749279121818236193, 1.000000000000000000, 0.9749279121818236193, 1.000000000000000000, 0.9749279121818236193, 1.000000000000000000, 0.9749279121818236193, 1.000000000000000000, 0.9749279121818236193, 1.000000000000000000, 0.9749279121818236193, 1.000000000000000000, 0.9749279121818236193, 1.000000000000000000, 0.9749279121818236193, 1.000000000000000000, 0.9749279121818236193, 1.000000000000000000, 0.9749279121818236193, 1.000000000000000000, 0.9749279121818236193, 1.000000000000000000, 0.9749279121818236193, 1.000000000000000000, 0.9749279121818236193, 1.000000000000000000, 0.9749279121818236193, 1.000000000000000000, 0.9749279121818236193, 1.000000000000000000, 0.9749279121818236193, 1.000000000000000000, 0.9749279121818236193, 1.000000000000000000, 0.9749279121818236193, 1.000000000000000000, 0.9749279121818236193, 1.000000000000000000, 0.9749279121818236193, 1.000000000000000000, 0.9749279121818236193, 1.000000000000000000, 0.9749279121818236193, 1.000000000000000000, 0.9749279121818236193, 1.000000000000000000, 0.9874639560909115321, 0.9874639560909117542),
 ( 0.3333333333333333703, 0.3333333333333333703, 0.3333333333333333703, 0.3249759707272745768, 0.3333333333333333703, 0.3249759707272745768, 0.3333333333333333703, 0.3249759707272745768, 0.3333333333333333703, 0.3249759707272745768, 0.3333333333333333703, 0.3249759707272745768, 0.3333333333333333703, 0.3249759707272745768, 0.3333333333333333703, 0.3249759707272745768, 0.3333333333333333703, 0.3249759707272745768, 0.3333333333333333703, 0.3249759707272745768, 0.3333333333333333703, 0.3249759707272745768, 0.3333333333333333703, 0.3249759707272745768, 0.3333333333333333703, 0.3249759707272745768, 0.3333333333333333703, 0.3249759707272745768, 0.3333333333333333703, 0.3249759707272745768, 0.3333333333333333703, 0.3249759707272745768, 0.3333333333333333703, 0.3249759707272745768, 0.3333333333333333703, 0.3249759707272745768, 0.3333333333333333703, 0.3249759707272745768, 0.3333333333333333703, 0.3249759707272745768, 0.3333333333333333703, 0.3249759707272745768, 0.3333333333333333703, 0.3249759707272745768, 0.3333333333333333703, 0.3249759707272745768, 0.3333333333333333703, 0.3249759707272745768, 0.3333333333333333703, 0.3249759707272745768, 0.3333333333333333703, 0.3249759707272745768, 0.3333333333333333703, 0.3249759707272745768, 0.3333333333333333703, 0.3249759707272745768, 0.3333333333333333703, 0.3249759707272745768, 0.3333333333333333703, 0.3249759707272745768, 0.3333333333333333703, 0.3249759707272745768, 0.3333333333333333703, 0.3249759707272745768, 0.3333333333333333703, 0.3249759707272745768, 0.3333333333333333703, 0.3249759707272745768, 0.3333333333333333703, 0.3249759707272745768, 0.3333333333333333703, 0.3249759707272745768, 0.3333333333333333703, 0.3249759707272745768, 0.3333333333333333703, 0.3249759707272745768, 0.3333333333333333703, 0.3249759707272745768, 0.3333333333333333703, 0.3249759707272745768, 0.3333333333333333703, 0.3249759707272745768, 0.3333333333333333703, 0.3249759707272745768, 0.3333333333333333703, 0.3249759707272745768, 0.3333333333333333703, 0.3249759707272745768, 0.3333333333333333703, 0.3249759707272745768, 0.3333333333333333703, 0.3249759707272745768, 0.3333333333333333703, 0.3249759707272745768, 0.3333333333333333703, 0.3249759707272745768, 0.3333333333333333703, 0.3249759707272745768, 0.3333333333333333703, 0.3249759707272745768, 0.3333333333333333703, 0.3249759707272745768, 0.3333333333333333703, 0.3249759707272745768, 0.3333333333333333703, 0.3249759707272745768, 0.3333333333333333703, 0.3249759707272745768, 0.3333333333333333703, 0.3249759707272745768, 0.3333333333333333703, 0.3249759707272745768, 0.3333333333333333703, 0.3249759707272745768, 0.3333333333333333703, 0.3249759707272745768, 0.3333333333333333703, 0.3249759707272745768, 0.3333333333333333703, 0.3249759707272745768, 0.3333333333333333703, 0.3291546520303039181, 0.3291546520303039736),
 ( 0.3333333333333333703, 0.3333333333333333703, 0.3333333333333333703, 0.3249759707272745768, 0.3333333333333333703, 0.3249759707272745768, 0.3333333333333333703, 0.3249759707272745768, 0.3333333333333333703, 0.3249759707272745768, 0.3333333333333333703, 0.3249759707272745768, 0.3333333333333333703, 0.3249759707272745768, 0.3333333333333333703, 0.3249759707272745768, 0.3333333333333333703, 0.3249759707272745768, 0.3333333333333333703, 0.3249759707272745768, 0.3333333333333333703, 0.3249759707272745768, 0.3333333333333333703, 0.3249759707272745768, 0.3333333333333333703, 0.3249759707272745768, 0.3333333333333333703, 0.3249759707272745768, 0.3333333333333333703, 0.3249759707272745768, 0.3333333333333333703, 0.3249759707272745768, 0.3333333333333333703, 0.3249759707272745768, 0.3333333333333333703, 0.3249759707272745768, 0.3333333333333333703, 0.3249759707272745768, 0.3333333333333333703, 0.3249759707272745768, 0.3333333333333333703, 0.3249759707272745768, 0.3333333333333333703, 0.3249759707272745768, 0.3333333333333333703, 0.3249759707272745768, 0.3333333333333333703, 0.3249759707272745768, 0.3333333333333333703, 0.3249759707272745768, 0.3333333333333333703, 0.3249759707272745768, 0.3333333333333333703, 0.3249759707272745768, 0.3333333333333333703, 0.3249759707272745768, 0.3333333333333333703, 0.3249759707272745768, 0.3333333333333333703, 0.3249759707272745768, 0.3333333333333333703, 0.3249759707272745768, 0.3333333333333333703, 0.3249759707272745768, 0.3333333333333333703, 0.3249759707272745768, 0.3333333333333333703, 0.3249759707272745768, 0.3333333333333333703, 0.3249759707272745768, 0.3333333333333333703, 0.3249759707272745768, 0.3333333333333333703, 0.3249759707272745768, 0.3333333333333333703, 0.3249759707272745768, 0.3333333333333333703, 0.3249759707272745768, 0.3333333333333333703, 0.3249759707272745768, 0.3333333333333333703, 0.3249759707272745768, 0.3333333333333333703, 0.3249759707272745768, 0.3333333333333333703, 0.3249759707272745768, 0.3333333333333333703, 0.3249759707272745768, 0.3333333333333333703, 0.3249759707272745768, 0.3333333333333333703, 0.3249759707272745768, 0.3333333333333333703, 0.3249759707272745768, 0.3333333333333333703, 0.3249759707272745768, 0.3333333333333333703, 0.3249759707272745768, 0.3333333333333333703, 0.3249759707272745768, 0.3333333333333333703, 0.3249759707272745768, 0.3333333333333333703, 0.3249759707272745768, 0.3333333333333333703, 0.3249759707272745768, 0.3333333333333333703, 0.3249759707272745768, 0.3333333333333333703, 0.3249759707272745768, 0.3333333333333333703, 0.3249759707272745768, 0.3333333333333333703, 0.3249759707272745768, 0.3333333333333333703, 0.3249759707272745768, 0.3333333333333333703, 0.3249759707272745768, 0.3333333333333333703, 0.3249759707272745768, 0.3333333333333333703, 0.3291546520303039181, 0.3291546520303039736),
 ( 1.000000000000000000, 1.000000000000000000, 1.000000000000000000, 0.9749279121818236193, 1.000000000000000000, 0.9749279121818236193, 1.000000000000000000, 0.9749279121818236193, 1.000000000000000000, 0.9749279121818236193, 1.000000000000000000, 0.9749279121818236193, 1.000000000000000000, 0.9749279121818236193, 1.000000000000000000, 0.9749279121818236193, 1.000000000000000000, 0.9749279121818236193, 1.000000000000000000, 0.9749279121818236193, 1.000000000000000000, 0.9749279121818236193, 1.000000000000000000, 0.9749279121818236193, 1.000000000000000000, 0.9749279121818236193, 1.000000000000000000, 0.9749279121818236193, 1.000000000000000000, 0.9749279121818236193, 1.000000000000000000, 0.9749279121818236193, 1.000000000000000000, 0.9749279121818236193, 1.000000000000000000, 0.9749279121818236193, 1.000000000000000000, 0.9749279121818236193, 1.000000000000000000, 0.9749279121818236193, 1.000000000000000000, 0.9749279121818236193, 1.000000000000000000, 0.9749279121818236193, 1.000000000000000000, 0.9749279121818236193, 1.000000000000000000, 0.9749279121818236193, 1.000000000000000000, 0.9749279121818236193, 1.000000000000000000, 0.9749279121818236193, 1.000000000000000000, 0.9749279121818236193, 1.000000000000000000, 0.9749279121818236193, 1.000000000000000000, 0.9749279121818236193, 1.000000000000000000, 0.9749279121818236193, 1.000000000000000000, 0.9749279121818236193, 1.000000000000000000, 0.9749279121818236193, 1.000000000000000000, 0.9749279121818236193, 1.000000000000000000, 0.9749279121818236193, 1.000000000000000000, 0.9749279121818236193, 1.000000000000000000, 0.9749279121818236193, 1.000000000000000000, 0.9749279121818236193, 1.000000000000000000, 0.9749279121818236193, 1.000000000000000000, 0.9749279121818236193, 1.000000000000000000, 0.9749279121818236193, 1.000000000000000000, 0.9749279121818236193, 1.000000000000000000, 0.9749279121818236193, 1.000000000000000000, 0.9749279121818236193, 1.000000000000000000, 0.9749279121818236193, 1.000000000000000000, 0.9749279121818236193, 1.000000000000000000, 0.9749279121818236193, 1.000000000000000000, 0.9749279121818236193, 1.000000000000000000, 0.9749279121818236193, 1.000000000000000000, 0.9749279121818236193, 1.000000000000000000, 0.9749279121818236193, 1.000000000000000000, 0.9749279121818236193, 1.000000000000000000, 0.9749279121818236193, 1.000000000000000000, 0.9749279121818236193, 1.000000000000000000, 0.9749279121818236193, 1.000000000000000000, 0.9749279121818236193, 1.000000000000000000, 0.9749279121818236193, 1.000000000000000000, 0.9749279121818236193, 1.000000000000000000, 0.9749279121818236193, 1.000000000000000000, 0.9749279121818236193, 1.000000000000000000, 0.9749279121818236193, 1.000000000000000000, 0.9874639560909115321, 0.9874639560909117542) ) ) 
 REPRESENTATION_ITEM ( '' )  SURFACE ( )  );
#91104 = CARTESIAN_POINT ( 'NONE',  ( 18.82351850331043863, -278.1715975867599582, -320.9253439018280005 ) ) ;
#91105 = ORIENTED_EDGE ( 'NONE', *, *, #34233, .T. ) ;
#91106 = CARTESIAN_POINT ( 'NONE',  ( -40.99919221731766328, -279.5149707911952532, -193.4964550853976561 ) ) ;
#91107 = CARTESIAN_POINT ( 'NONE',  ( 20.21480145023641839, -277.1303281130089431, -315.6655045440019194 ) ) ;
#91108 = CARTESIAN_POINT ( 'NONE',  ( 7.659227149099407939, -278.2078693657250597, -331.6544610544016223 ) ) ;
#91109 = CARTESIAN_POINT ( 'NONE',  ( -79.33105313509143741, -275.6355789438951547, -332.9963122945742384 ) ) ;
#91110 = CARTESIAN_POINT ( 'NONE',  ( -14.05175544632568041, -274.8549589020640838, -201.1110860814869170 ) ) ;
#91111 = CARTESIAN_POINT ( 'NONE',  ( -61.22139527606407938, -293.9429678346589299, -340.0221344507196477 ) ) ;
#91112 = CARTESIAN_POINT ( 'NONE',  ( 85.55100297371609486, -373.0521521680024648, -521.1711561948568487 ) ) ;
#91113 = CARTESIAN_POINT ( 'NONE',  ( 30.66448207899649603, -281.5782029110057465, -234.2658066876924181 ) ) ;
#91114 = CARTESIAN_POINT ( 'NONE',  ( -110.1681798653654880, -278.6433785491622643, -276.0809966728783706 ) ) ;
#91115 = CARTESIAN_POINT ( 'NONE',  ( 16.32799796159937245, -286.9944393058921150, -324.9587260141474303 ) ) ;
#91116 = CARTESIAN_POINT ( 'NONE',  ( -21.79489099465742186, -276.2515857259405720, -196.9901607077368340 ) ) ;
#91117 = DIRECTION ( 'NONE',  ( -5.551115123125777653E-14, 0.000000000000000000, 1.000000000000000000 ) ) ;
#91118 = AXIS2_PLACEMENT_3D ( 'NONE', #12820, #41660, #34578 ) ;
#91119 = CARTESIAN_POINT ( 'NONE',  ( -48.09479457895627519, -288.3894816949112396, -342.7791843982212185 ) ) ;
#91120 = CARTESIAN_POINT ( 'NONE',  ( -90.37385592451531124, -283.1274661494136353, -326.1198924788092199 ) ) ;
#91121 = CARTESIAN_POINT ( 'NONE',  ( -0.7705315264256661356, -280.7991299456670617, -334.7080187723231006 ) ) ;
#91123 = CARTESIAN_POINT ( 'NONE',  ( -80.11715233710630457, -283.5483958948841519, -209.3751547080865691 ) ) ;
#91122 = CARTESIAN_POINT ( 'NONE',  ( 26.98261595473158181, -279.6420769262680324, -234.6153871012163847 ) ) ;
#91124 = CARTESIAN_POINT ( 'NONE',  ( -49.77975540794616194, -287.8937990868191150, -196.3475945179768587 ) ) ;
#91125 = CARTESIAN_POINT ( 'NONE',  ( -68.70682381515995019, -280.8354766992522400, -204.0033036554774526 ) ) ;
#91126 = LINE ( 'NONE', #76959, #62450 ) ;
#91127 = CIRCLE ( 'NONE', #88099, 3.491568894204821749 ) ;
#91128 = CARTESIAN_POINT ( 'NONE',  ( -66.26823076813668933, -293.6736317085897667, -201.1638891686486375 ) ) ;
#91129 = CARTESIAN_POINT ( 'NONE',  ( -71.14053061027676961, -275.7320125167084370, -338.4170734547194002 ) ) ;
#91130 = AXIS2_PLACEMENT_3D ( 'NONE', #4847, #76360, #3923 ) ;
#91131 = CARTESIAN_POINT ( 'NONE',  ( -64.36311352750779236, -278.0656231866486792, -338.3393588691618561 ) ) ;
#91132 = CARTESIAN_POINT ( 'NONE',  ( -110.4303697114122116, -286.3267434986474882, -287.9675886507163796 ) ) ;
#91133 = CIRCLE ( 'NONE', #53378, 2.000000000000001776 ) ;
#91134 = AXIS2_PLACEMENT_3D ( 'NONE', #16010, #36851, #81779 ) ;
#91135 = CARTESIAN_POINT ( 'NONE',  ( 104.1717476309105166, -299.5541904835127980, -195.3611179825600175 ) ) ;
#91136 = CARTESIAN_POINT ( 'NONE',  ( -111.1533240022837816, -292.2663411257876760, -286.5215135008785410 ) ) ;
#91137 = CIRCLE ( 'NONE', #60980, 1.000000000000000888 ) ;
#91138 = CARTESIAN_POINT ( 'NONE',  ( -38.21988350492071618, -293.0630105629219315, -345.3685269068163848 ) ) ;
#91139 = CARTESIAN_POINT ( 'NONE',  ( -30.88720699871515762, -285.3289064184366453, -193.7808977009793523 ) ) ;
#91140 = DIRECTION ( 'NONE',  ( -0.000000000000000000, 1.000000000000000000, -0.000000000000000000 ) ) ;
#91141 = CARTESIAN_POINT ( 'NONE',  ( 35.51155968610129321, -274.1101725387546253, -260.6840310026798306 ) ) ;
#91142 = CARTESIAN_POINT ( 'NONE',  ( -41.12548022622988242, -293.2398284290188144, -344.5126089476709694 ) ) ;
#91143 = CARTESIAN_POINT ( 'NONE',  ( 195.6782526186922269, 40.73232731989658362, 14.69414600581795050 ) ) ;
#91144 = CARTESIAN_POINT ( 'NONE',  ( 197.8477145984406889, 64.61450673763175701, 7.741079165001056417 ) ) ;
#91145 = CARTESIAN_POINT ( 'NONE',  ( -70.57807687372837790, -290.1017145325866977, -201.6730475722353049 ) ) ;
#91146 = CARTESIAN_POINT ( 'NONE',  ( -41.38693288121886837, -287.6005376149668677, -196.6594299747017374 ) ) ;
#91147 = CARTESIAN_POINT ( 'NONE',  ( 21.60467206546135088, -286.4441540502930366, -318.3325962722149711 ) ) ;
#91148 = CIRCLE ( 'NONE', #86645, 0.9999999999999998890 ) ;
#91149 = CARTESIAN_POINT ( 'NONE',  ( -101.5139699641699451, -286.4675323826448334, -234.2386648065198074 ) ) ;
#91150 = CARTESIAN_POINT ( 'NONE',  ( 154.1415209985679269, 20.37991841447901820, -11.45812909362559040 ) ) ;
#91151 = CARTESIAN_POINT ( 'NONE',  ( 0.2428599936132283532, -287.3690090560045292, -207.5326206330393575 ) ) ;
#91152 = CARTESIAN_POINT ( 'NONE',  ( 36.15142411509117437, -295.3186181277409332, -253.6550036725486734 ) ) ;
#91153 = CARTESIAN_POINT ( 'NONE',  ( -39.93842410471280857, -275.1643568117752920, -345.8893103126946471 ) ) ;
#91154 = CARTESIAN_POINT ( 'NONE',  ( 19.86433370714091851, -276.5849809431883273, -321.8902041055885093 ) ) ;
#91155 = AXIS2_PLACEMENT_3D ( 'NONE', #37710, #51455, #23980 ) ;
#91156 = CARTESIAN_POINT ( 'NONE',  ( 25.31281544100516001, -291.0638748786709016, -228.0348577190633534 ) ) ;
#91157 = CARTESIAN_POINT ( 'NONE',  ( -77.49251644047828336, -279.5295137937271761, -204.5961810932253115 ) ) ;
#91158 = CARTESIAN_POINT ( 'NONE',  ( -69.19687180141157512, -297.4530941586672270, -337.8814147295076395 ) ) ;
#91159 = CARTESIAN_POINT ( 'NONE',  ( -23.68628624284178130, -44.55766379199612004, 22.50000000000000000 ) ) ;
#91160 = DIRECTION ( 'NONE',  ( 0.000000000000000000, 0.000000000000000000, 1.000000000000000000 ) ) ;
#91161 = CARTESIAN_POINT ( 'NONE',  ( -11.83523223400857205, -285.0761274482836143, -201.4360603221494159 ) ) ;
#91162 = CARTESIAN_POINT ( 'NONE',  ( -81.57403355917152510, -275.8009975677020407, -329.9796231370935402 ) ) ;
#91163 = CARTESIAN_POINT ( 'NONE',  ( 33.44863614909306904, -279.2294068253228261, -245.4322969748367882 ) ) ;
#91164 = DIRECTION ( 'NONE',  ( 0.9764705882352960886, 0.000000000000000000, -0.2156506209390900708 ) ) ;
#91165 = CARTESIAN_POINT ( 'NONE',  ( 25.58388106276237295, -273.4569774017685972, -227.1745515018921822 ) ) ;
#91166 = CARTESIAN_POINT ( 'NONE',  ( -107.9208395050715552, -277.6496055655351824, -289.3999665096213789 ) ) ;
#91167 = CARTESIAN_POINT ( 'NONE',  ( 4.223254074979974071, -296.0005677408698261, -331.2139103030986576 ) ) ;
#91168 = CIRCLE ( 'NONE', #14098, 23.00000000000000711 ) ;
#91169 = CARTESIAN_POINT ( 'NONE',  ( -38.15278955346298062, -278.9625449387969525, -193.6745178159125658 ) ) ;
#91170 = CARTESIAN_POINT ( 'NONE',  ( -34.27939665490124099, -295.9539623870759328, -343.5323605991071645 ) ) ;
#91171 = CARTESIAN_POINT ( 'NONE',  ( -104.8265627010655834, -298.3373609539154927, -234.2057751478373007 ) ) ;
#91172 = CARTESIAN_POINT ( 'NONE',  ( -92.74302058066339782, -297.0623615167057778, -222.8056558867747867 ) ) ;
#91173 = CARTESIAN_POINT ( 'NONE',  ( -66.11723532431140882, -293.6757415129305286, -201.0870750876899820 ) ) ;
#91174 = CARTESIAN_POINT ( 'NONE',  ( -100.9976888636195582, -285.2912086263243623, -226.9435482991604829 ) ) ;
#91175 = CARTESIAN_POINT ( 'NONE',  ( 36.74267169341347739, -273.4892675108972071, -254.4311332663733936 ) ) ;
#91176 = CARTESIAN_POINT ( 'NONE',  ( 30.36167868341750165, -287.8611994579429165, -307.1503073310834679 ) ) ;
#91177 = CARTESIAN_POINT ( 'NONE',  ( -110.7542260487683166, -280.7063025978318365, -256.8537924575717852 ) ) ;
#91178 = CARTESIAN_POINT ( 'NONE',  ( 35.19174914420086964, -286.7450961431770793, -280.5670182140430597 ) ) ;
#91179 = CARTESIAN_POINT ( 'NONE',  ( -110.6169402856506565, -288.3466611573664977, -286.3529856975630423 ) ) ;
#91180 = ORIENTED_EDGE ( 'NONE', *, *, #62216, .F. ) ;
#91181 = CARTESIAN_POINT ( 'NONE',  ( 134.9260051231060800, 178.6636279401649858, -236.0341445084446548 ) ) ;
#91182 = CARTESIAN_POINT ( 'NONE',  ( -23.77989730216035724, -288.3819591849186850, -342.2046832395990918 ) ) ;
#91183 = CARTESIAN_POINT ( 'NONE',  ( -61.14728354254373954, -284.2949582614295423, -343.3968618803212394 ) ) ;
#91184 = CARTESIAN_POINT ( 'NONE',  ( -98.15449028097435757, -290.2381848154611816, -223.4930305982076959 ) ) ;
#91185 = CARTESIAN_POINT ( 'NONE',  ( 38.83995597524599930, -283.1107051754440249, -267.0713769925428096 ) ) ;
#91186 = ADVANCED_FACE ( 'NONE', ( #49196 ), #27909, .T. ) ;
#91187 = CARTESIAN_POINT ( 'NONE',  ( -59.17751767948421815, -281.0904549733824069, -197.0365290405921428 ) ) ;
#91188 = CARTESIAN_POINT ( 'NONE',  ( 28.97357045158723210, -280.9723223964496128, -239.7230077796126579 ) ) ;
#91189 = CARTESIAN_POINT ( 'NONE',  ( 0.4398160855076280740, -276.5556580843460210, -205.5575686543582492 ) ) ;
#91190 = CARTESIAN_POINT ( 'NONE',  ( -34.85464314124794782, -295.0217161261292063, -347.3209422257600636 ) ) ;
#91191 = CARTESIAN_POINT ( 'NONE',  ( -98.08548462581161687, -289.1660821441731173, -226.8912489125631851 ) ) ;
#91192 = CARTESIAN_POINT ( 'NONE',  ( 52.15744429099725465, -298.1187141199046664, -197.0689410925062361 ) ) ;
#91193 = ORIENTED_EDGE ( 'NONE', *, *, #33593, .T. ) ;
#91194 = ORIENTED_EDGE ( 'NONE', *, *, #78924, .T. ) ;
#91195 = CARTESIAN_POINT ( 'NONE',  ( -94.51261618817551380, -285.8088720643203828, -318.0350160593292230 ) ) ;
#91196 = CIRCLE ( 'NONE', #74524, 20.00000000000000355 ) ;
#91197 = CARTESIAN_POINT ( 'NONE',  ( -70.66109363059125315, -296.5608803184114208, -339.4502423935154525 ) ) ;
#91198 = CARTESIAN_POINT ( 'NONE',  ( 14.00217284268275186, -282.9598814247329415, -322.4679566670448594 ) ) ;
#91199 = CARTESIAN_POINT ( 'NONE',  ( 24.17190392111125874, -275.2236974222782919, -316.2838436256404862 ) ) ;
#91200 = CARTESIAN_POINT ( 'NONE',  ( -88.58773585299572062, -292.0066231195654041, -213.0273878685330260 ) ) ;
#91201 = CARTESIAN_POINT ( 'NONE',  ( -33.76160766181091333, -284.2363424040913173, -194.6809460743868101 ) ) ;
#91202 = CARTESIAN_POINT ( 'NONE',  ( 8.834851233142318350, -292.9990086904267059, -208.7034376754828884 ) ) ;
#91204 = CARTESIAN_POINT ( 'NONE',  ( -94.11804822104657831, -290.2361271288630746, -316.2798917477898044 ) ) ;
#91203 = AXIS2_PLACEMENT_3D ( 'NONE', #40361, #33286, #33760 ) ;
#91205 = CARTESIAN_POINT ( 'NONE',  ( 115.2448031289451222, -299.5541904835127980, -198.2496582146980302 ) ) ;
#91206 = CIRCLE ( 'NONE', #59480, 2.500000000000002220 ) ;
#91207 = DIRECTION ( 'NONE',  ( 1.000000000000000000, 0.000000000000000000, 0.000000000000000000 ) ) ;
#91208 = CARTESIAN_POINT ( 'NONE',  ( -82.19941185436130127, -219.0997270613688670, -349.0470628824017467 ) ) ;
#91209 = CARTESIAN_POINT ( 'NONE',  ( -83.44872848485381667, -285.1911182727992013, -331.2292047662632513 ) ) ;
#91210 = CARTESIAN_POINT ( 'NONE',  ( 39.58706461736021254, -279.0523547857347921, -270.3937649182068981 ) ) ;
#91211 = ORIENTED_EDGE ( 'NONE', *, *, #19481, .F. ) ;
#91212 = CARTESIAN_POINT ( 'NONE',  ( 35.00641068001061029, -280.6278915892891632, -282.1923028971748408 ) ) ;
#91213 = CARTESIAN_POINT ( 'NONE',  ( -28.60765223002002600, -276.6111153869907184, -346.8964454929711110 ) ) ;
#91214 = CARTESIAN_POINT ( 'NONE',  ( -109.7528847541661889, -280.7961214315325833, -251.4255698042724418 ) ) ;
#91215 = CARTESIAN_POINT ( 'NONE',  ( -37.45856812746255571, -140.9159241237307185, -362.6039797469185260 ) ) ;
#91216 = CARTESIAN_POINT ( 'NONE',  ( -1.396452039911038723, -279.0940891009174152, -202.9330419764321221 ) ) ;
#91218 = CARTESIAN_POINT ( 'NONE',  ( -63.10747744129525927, -283.7351743835561138, -200.2490867062971915 ) ) ;
#91217 = AXIS2_PLACEMENT_3D ( 'NONE', #74384, #2891, #60668 ) ;
#91219 = CARTESIAN_POINT ( 'NONE',  ( -37.62665763008747888, -299.8087642997211901, -194.3749822932419704 ) ) ;
#91220 = MANIFOLD_SOLID_BREP ( 'Cut-Extrude10', #29514 ) ;
#91221 = CARTESIAN_POINT ( 'NONE',  ( 18.88446801193410352, -294.7056354384393444, -317.0152331080279282 ) ) ;
#91222 = VERTEX_POINT ( 'NONE', #13690 ) ;
#91223 = CARTESIAN_POINT ( 'NONE',  ( -105.1516594518534617, -289.6161362530509109, -241.8905698363981287 ) ) ;
#91224 = CARTESIAN_POINT ( 'NONE',  ( -5.319649073906242975, -277.2931421010299573, -340.2746433786214197 ) ) ;
#91225 = CARTESIAN_POINT ( 'NONE',  ( 33.50918050270857407, -275.3201304803966991, -252.7783788944213939 ) ) ;
#91226 = CARTESIAN_POINT ( 'NONE',  ( 24.23990536485205283, -273.8623176863985123, -224.6533683608712124 ) ) ;
#91227 = DIRECTION ( 'NONE',  ( 0.000000000000000000, -1.000000000000000000, 0.000000000000000000 ) ) ;
#91228 = CARTESIAN_POINT ( 'NONE',  ( -112.3407595013127604, -270.5879613108983222, -267.5593803803137689 ) ) ;
#91229 = VECTOR ( 'NONE', #19436, 1000.000000000000000 ) ;
#91230 = CARTESIAN_POINT ( 'NONE',  ( 208.6208076322478746, 32.98517505407394168, 15.00000000000000000 ) ) ;
#91231 = CARTESIAN_POINT ( 'NONE',  ( -43.28564603558642432, -274.0543938782848272, -506.4777364308019401 ) ) ;
#91232 = VECTOR ( 'NONE', #17370, 1000.000000000000000 ) ;
#91233 = CARTESIAN_POINT ( 'NONE',  ( 1.275780383236181370, -283.6032046678731717, -332.7334504865265785 ) ) ;
#91234 = CARTESIAN_POINT ( 'NONE',  ( 15.07100037025026040, -284.0848382429485355, -325.3782320343473202 ) ) ;
#91235 = CARTESIAN_POINT ( 'NONE',  ( -95.20220198837948544, -283.2723736632433997, -315.0587855295223676 ) ) ;
#91236 = CARTESIAN_POINT ( 'NONE',  ( 33.63499765952607845, -273.6854549047521914, -249.9607960373914750 ) ) ;
#91237 = CARTESIAN_POINT ( 'NONE',  ( 22.30758168845396838, -282.8029982556293476, -226.1489109688006636 ) ) ;
#91238 = CARTESIAN_POINT ( 'NONE',  ( -99.77267198196132370, -276.4953160061438098, -309.6110597349018576 ) ) ;
#91239 = CARTESIAN_POINT ( 'NONE',  ( 183.0442525570908288, 300.2961574867697436, -7.500000000000000000 ) ) ;
#91240 = CARTESIAN_POINT ( 'NONE',  ( 17.50772282984454620, -275.9390178205849224, -221.6467668302588265 ) ) ;
#91241 = CARTESIAN_POINT ( 'NONE',  ( 194.3451372756567537, 40.15325844710437053, 14.51211662731439844 ) ) ;
#91242 = CARTESIAN_POINT ( 'NONE',  ( -22.60718213729673565, -281.0388419842026906, -194.8944267758628541 ) ) ;
#91243 = CIRCLE ( 'NONE', #50382, 1.500000000000001332 ) ;
#91244 = ORIENTED_EDGE ( 'NONE', *, *, #90537, .T. ) ;
#91245 = CARTESIAN_POINT ( 'NONE',  ( 197.9834613664959591, 18.87240044341487533, 11.15593255764673408 ) ) ;
#91246 = CARTESIAN_POINT ( 'NONE',  ( -29.61287910174063143, -288.0094571674408144, -194.9915564524682168 ) ) ;
#91247 = CARTESIAN_POINT ( 'NONE',  ( -68.59558629629512438, -294.6708202636175429, -336.5246824996507939 ) ) ;
#91248 = CARTESIAN_POINT ( 'NONE',  ( -114.1498885402841807, -289.8541943165051862, -274.0779686834404743 ) ) ;
#91249 = CARTESIAN_POINT ( 'NONE',  ( 19.45358290260161738, -285.1274609166684399, -222.8832804056557393 ) ) ;
#91251 = CARTESIAN_POINT ( 'NONE',  ( -99.13335567182939201, -289.3504158651628586, -229.5278475491807626 ) ) ;
#91250 = CARTESIAN_POINT ( 'NONE',  ( 9.418773466919910575, -285.2845214201378781, -213.5382966463484422 ) ) ;
#91252 = CARTESIAN_POINT ( 'NONE',  ( -106.9135861263490312, -286.0680764986466897, -246.8163411235290141 ) ) ;
#91253 = CARTESIAN_POINT ( 'NONE',  ( 0.02781816129643214022, -274.5550432056894010, -335.4470851720672613 ) ) ;
#91254 = CARTESIAN_POINT ( 'NONE',  ( 13.72600977953973533, -285.1532728594528976, -213.7347662021486201 ) ) ;
#91255 = CARTESIAN_POINT ( 'NONE',  ( -96.66802440740052305, -299.1813919990765385, -224.4558752512333228 ) ) ;
#91256 = CARTESIAN_POINT ( 'NONE',  ( 27.13926965407637937, -285.0347991584364991, -231.6312483817269197 ) ) ;
#91257 = CARTESIAN_POINT ( 'NONE',  ( 18.13494964482363514, -281.8144718828905297, -222.5323560032991850 ) ) ;
#91258 = CARTESIAN_POINT ( 'NONE',  ( -81.74855100402548658, -291.6555331162216476, -331.0081296070798089 ) ) ;
#91259 = CYLINDRICAL_SURFACE ( 'NONE', #6660, 5.000000000000000888 ) ;
#91260 = CARTESIAN_POINT ( 'NONE',  ( 155.4526335419795373, 18.61728136335800343, -8.651974842892215634 ) ) ;
#91261 = CARTESIAN_POINT ( 'NONE',  ( -50.19799470182257295, -297.1350241498703895, -344.8722944920820623 ) ) ;
#91262 = CARTESIAN_POINT ( 'NONE',  ( -77.88208727294285438, -277.5077983827608819, -207.2002697336634185 ) ) ;
#91263 = CARTESIAN_POINT ( 'NONE',  ( -3.383483752952189949, -291.6862626266616871, -201.4191233759826218 ) ) ;
#91264 = CARTESIAN_POINT ( 'NONE',  ( -108.3783306260521471, -294.6904311970313870, -290.3670556954279505 ) ) ;
#91265 = CARTESIAN_POINT ( 'NONE',  ( 8.085731424016778135, -281.1012431243286755, -328.1979967438466588 ) ) ;
#91266 = CARTESIAN_POINT ( 'NONE',  ( -13.58314515275353784, -272.4428463835358798, -199.8143585816483210 ) ) ;
#91267 = CARTESIAN_POINT ( 'NONE',  ( 25.25921100355509452, -294.3389911268475316, -231.7629899049199480 ) ) ;
#91268 = CARTESIAN_POINT ( 'NONE',  ( -4.771743288812468897, -291.1233781216987495, -337.9199732462171255 ) ) ;
#91269 = CARTESIAN_POINT ( 'NONE',  ( -97.73767100012669573, -294.4038934749632972, -316.9983826705367278 ) ) ;
#91270 = CARTESIAN_POINT ( 'NONE',  ( -8.789871987137727771, -292.9236992624399818, -340.8353620211534007 ) ) ;
#91271 = CARTESIAN_POINT ( 'NONE',  ( -110.5609595067740543, -292.0738732060030998, -262.9912487543835482 ) ) ;
#91272 = LINE ( 'NONE', #55329, #25940 ) ;
#91273 = CARTESIAN_POINT ( 'NONE',  ( -67.87788778166178361, -292.4436131836936283, -203.8631964398795162 ) ) ;
#91274 = CARTESIAN_POINT ( 'NONE',  ( 189.9243309297870610, 275.0000000000000568, 15.22542485937351664 ) ) ;
#91276 = CARTESIAN_POINT ( 'NONE',  ( -17.43259608145457307, -292.3161704390975615, -200.0758581772058449 ) ) ;
#91275 = CARTESIAN_POINT ( 'NONE',  ( 1.230095228631854498, -280.5598161610066086, -335.0961425483314997 ) ) ;
#91277 = CIRCLE ( 'NONE', #50480, 0.5000000000000009992 ) ;
#91278 = CARTESIAN_POINT ( 'NONE',  ( 17.22311194634449549, -280.8043158201616620, -215.9569753895094095 ) ) ;
#91279 = CARTESIAN_POINT ( 'NONE',  ( -86.09225791230193181, -283.3738707646173225, -329.9356713351689336 ) ) ;
#91280 = CARTESIAN_POINT ( 'NONE',  ( 11.28777492635730084, -286.3767784430328334, -327.3084558805859956 ) ) ;
#91281 = CARTESIAN_POINT ( 'NONE',  ( -85.68378825524501963, -281.8692161328968382, -326.6985655031110696 ) ) ;
#91282 = CARTESIAN_POINT ( 'NONE',  ( 24.04559783597816747, -279.4242473727307470, -225.0366499457509804 ) ) ;
#91283 = AXIS2_PLACEMENT_3D ( 'NONE', #84284, #54945, #48298 ) ;
#91284 = CARTESIAN_POINT ( 'NONE',  ( 28.44050858424596839, -285.9551399711476734, -230.8354079063705626 ) ) ;
#91285 = CARTESIAN_POINT ( 'NONE',  ( -83.63170945779074827, -373.0521521680024648, -521.1711561948568487 ) ) ;
#91286 = CARTESIAN_POINT ( 'NONE',  ( 35.11364362255328331, -295.3352736961820142, -284.3847972003716222 ) ) ;
#91287 = CARTESIAN_POINT ( 'NONE',  ( -38.51754974594984304, -278.4918911310675185, -346.7628435698167095 ) ) ;
#91288 = CARTESIAN_POINT ( 'NONE',  ( -80.83537442462778699, -277.3278865263428656, -329.0159369053936302 ) ) ;
#91289 = CARTESIAN_POINT ( 'NONE',  ( -100.0322822802275624, -291.3109982988033266, -225.6521601112227984 ) ) ;
#91290 = AXIS2_PLACEMENT_3D ( 'NONE', #2342, #73380, #74770 ) ;
#91291 = CARTESIAN_POINT ( 'NONE',  ( 10.56045666592079257, -280.4767086457568439, -328.8642206116721809 ) ) ;
#91292 = AXIS2_PLACEMENT_3D ( 'NONE', #81212, #66110, #2155 ) ;
#91293 = ADVANCED_FACE ( 'NONE', ( #70984 ), #19372, .F. ) ;
#91294 = CARTESIAN_POINT ( 'NONE',  ( 16.92056002333560727, -291.9077598748362448, -221.1032366057138461 ) ) ;
#91295 = CARTESIAN_POINT ( 'NONE',  ( -99.08921189694146392, -295.1292966939730036, -227.7680830393643134 ) ) ;
#91296 = ORIENTED_EDGE ( 'NONE', *, *, #4934, .T. ) ;
#91297 = CARTESIAN_POINT ( 'NONE',  ( 201.2509219215140206, 65.09645894978946501, -2.617322427804798401 ) ) ;
#91298 = CARTESIAN_POINT ( 'NONE',  ( 35.35722735411813744, -292.9575275240945871, -262.6016047728442686 ) ) ;
#91299 = DIRECTION ( 'NONE',  ( 1.000000000000000000, 0.000000000000000000, 0.000000000000000000 ) ) ;
#91300 = CARTESIAN_POINT ( 'NONE',  ( -92.08974858914540107, -287.4094976428775112, -313.9805196606274080 ) ) ;
#91301 = CARTESIAN_POINT ( 'NONE',  ( 30.54179879548563292, -297.9412943616089251, -193.6069287863579689 ) ) ;
#91302 = CARTESIAN_POINT ( 'NONE',  ( -2.929649398343377786, -278.6415350863802018, -202.8476154217746341 ) ) ;
#91303 = CARTESIAN_POINT ( 'NONE',  ( -57.64131366847546190, -287.1106933631196512, -196.5414649848554802 ) ) ;
#91304 = CARTESIAN_POINT ( 'NONE',  ( -45.36455647170634364, -288.9899505576246383, -342.9189141218286068 ) ) ;
#91305 = CARTESIAN_POINT ( 'NONE',  ( -111.0856700441927813, -280.0683763114077465, -270.6600037201490636 ) ) ;
#91306 = CARTESIAN_POINT ( 'NONE',  ( -110.2027499684331389, -294.3629977138155027, -286.5819139941789899 ) ) ;
#91307 = CARTESIAN_POINT ( 'NONE',  ( -93.84163265591229219, -297.6418946340604634, -318.1900699764167371 ) ) ;
#91308 = CIRCLE ( 'NONE', #50511, 0.4999999999999929501 ) ;
#91309 = CARTESIAN_POINT ( 'NONE',  ( -85.37663542332029465, -276.5281358890228489, -325.9241800736950836 ) ) ;
#91310 = ORIENTED_EDGE ( 'NONE', *, *, #9906, .T. ) ;
#91311 = CARTESIAN_POINT ( 'NONE',  ( -108.0766608621983238, -272.7745362790577133, -239.8031790565791823 ) ) ;
#91312 = CARTESIAN_POINT ( 'NONE',  ( -45.49638112859755523, -291.0764482653454479, -344.3531133248914102 ) ) ;
#91313 = CARTESIAN_POINT ( 'NONE',  ( 36.97648645787506183, -294.9389158397447090, -253.4727261746196234 ) ) ;
#91314 = CARTESIAN_POINT ( 'NONE',  ( 201.3748867796775528, 292.7342570268831992, -53.99999999997705658 ) ) ;
#91315 = ADVANCED_FACE ( 'NONE', ( #71455 ), #77967, .F. ) ;
#91316 = CARTESIAN_POINT ( 'NONE',  ( -10.67920029253470204, -289.3465400325216592, -338.4815843186699453 ) ) ;
#91317 = CARTESIAN_POINT ( 'NONE',  ( -48.18343439339133027, -254.6143759403197180, -455.9956540770752440 ) ) ;
#91318 = CARTESIAN_POINT ( 'NONE',  ( -111.4915245893550804, -296.9480044736803848, -290.7355215118308251 ) ) ;
#91319 = CARTESIAN_POINT ( 'NONE',  ( -70.33802008173235265, -289.7614756711588484, -202.1588573561230362 ) ) ;
#91320 = CARTESIAN_POINT ( 'NONE',  ( -35.47680861834266608, -298.4081822115830391, -193.3821595793300787 ) ) ;
#91321 = CYLINDRICAL_SURFACE ( 'NONE', #7989, 4.999999999999990230 ) ;
#91322 = CARTESIAN_POINT ( 'NONE',  ( 208.6208076322478746, 32.98517505407394168, 12.09245862095555601 ) ) ;
#91323 = CARTESIAN_POINT ( 'NONE',  ( -51.53717440752282641, -290.7506691636865526, -345.3357554339218041 ) ) ;
#91324 = CARTESIAN_POINT ( 'NONE',  ( 13.79469577742117714, -283.1948066931273615, -206.1857440867352693 ) ) ;
#91325 = CARTESIAN_POINT ( 'NONE',  ( -3.694709121519613504, -279.8330995285274412, -201.2004483965756094 ) ) ;
#91326 = CARTESIAN_POINT ( 'NONE',  ( -70.82503165676855872, -287.6096530861794349, -203.4222750548792362 ) ) ;
#91327 = CARTESIAN_POINT ( 'NONE',  ( 34.30806571156131923, -285.7886311819240746, -243.8108383795934913 ) ) ;
#91328 = CARTESIAN_POINT ( 'NONE',  ( -70.27541464969006313, -271.6169354844466852, -203.1644002145726233 ) ) ;
#91329 = CARTESIAN_POINT ( 'NONE',  ( -65.12857643057765245, -275.6064080204309334, -201.2879484714622436 ) ) ;
#91330 = CARTESIAN_POINT ( 'NONE',  ( -105.3735108725226155, -288.2316181851806505, -300.7041839076871383 ) ) ;
#91331 = CARTESIAN_POINT ( 'NONE',  ( -95.19049134432600567, -279.7423914618739786, -319.3078431985452994 ) ) ;
#91332 = VERTEX_POINT ( 'NONE', #92264 ) ;
#91334 = CARTESIAN_POINT ( 'NONE',  ( 25.22782187993439962, -280.3799719185362278, -232.4615809328921614 ) ) ;
#91333 = CARTESIAN_POINT ( 'NONE',  ( -27.55837506603365483, -280.1797575460331586, -197.9684690198365615 ) ) ;
#91335 = CARTESIAN_POINT ( 'NONE',  ( 36.20096867460583212, -276.9062808670003051, -292.1553155748598556 ) ) ;
#91336 = CARTESIAN_POINT ( 'NONE',  ( 39.22244748885121624, -280.3777167532342673, -272.7983330314016257 ) ) ;
#91337 = CARTESIAN_POINT ( 'NONE',  ( 159.3109176245238245, 219.1064649780328750, -202.8775829912029280 ) ) ;
#91338 = CARTESIAN_POINT ( 'NONE',  ( 38.25828488781869652, -276.3253445144696343, -256.9645685401634978 ) ) ;
#91339 = CARTESIAN_POINT ( 'NONE',  ( -36.91930833898076969, -299.4826080567211761, -193.9502423678791558 ) ) ;
#91340 = CARTESIAN_POINT ( 'NONE',  ( 21.31550574532285580, -284.6948066931273615, -317.0979686699210447 ) ) ;
#91341 = VERTEX_POINT ( 'NONE', #64843 ) ;
#91342 = B_SPLINE_CURVE_WITH_KNOTS ( 'NONE', 3,
 ( #78962, #51002, #42493, #14579, #93617, #50066, #42020, #64337 ),
 .UNSPECIFIED., .F., .F.,
 ( 4, 2, 2, 4 ),
 ( 0.000000000000000000, 0.001936817825059323562, 0.002905226737588965501, 0.003873635650118607658 ),
 .UNSPECIFIED. ) ;
#91343 = AXIS2_PLACEMENT_3D ( 'NONE', #85459, #56605, #28183 ) ;
#91344 = CARTESIAN_POINT ( 'NONE',  ( 175.2296996224750103, 134.0000000000000284, 0.000000000000000000 ) ) ;
#91345 = CARTESIAN_POINT ( 'NONE',  ( 8.182605621984954780, -289.4920466269820167, -327.8220930752488016 ) ) ;
#91346 = CARTESIAN_POINT ( 'NONE',  ( 37.55421881697458986, -289.1487409091860172, -257.4560094781718931 ) ) ;
#91347 = CARTESIAN_POINT ( 'NONE',  ( -109.5210734596103492, -289.7471891699900652, -282.0170710087725183 ) ) ;
#91348 = CARTESIAN_POINT ( 'NONE',  ( -78.48425815463491517, -285.0216988905369817, -205.3471439294624759 ) ) ;
#91349 = CARTESIAN_POINT ( 'NONE',  ( -21.01072962688938617, -108.8955080185006210, -362.6946229046635040 ) ) ;
#91350 = CARTESIAN_POINT ( 'NONE',  ( 35.12362110089673450, -279.7688346066968279, -256.3224183162952272 ) ) ;
#91351 = CARTESIAN_POINT ( 'NONE',  ( 34.21367010567445988, -289.1557266186640049, -250.5951251473379386 ) ) ;
#91352 = CARTESIAN_POINT ( 'NONE',  ( -26.66124085334093152, -281.3938430229496817, -343.3281659134847246 ) ) ;
#91353 = CARTESIAN_POINT ( 'NONE',  ( -110.3922834572073839, -279.7559256732691324, -278.8633887699262459 ) ) ;
#91354 = AXIS2_PLACEMENT_3D ( 'NONE', #26901, #61504, #25491 ) ;
#91355 = CARTESIAN_POINT ( 'NONE',  ( 0.9089829729819068893, -277.0195155218212335, -332.6690506112148000 ) ) ;
#91356 = CARTESIAN_POINT ( 'NONE',  ( -113.9712288262322346, -289.3723632383288873, -268.3497450973521268 ) ) ;
#91357 = CARTESIAN_POINT ( 'NONE',  ( -71.00473057962327061, -286.4220070058735814, -201.2889875521412932 ) ) ;
#91358 = CARTESIAN_POINT ( 'NONE',  ( -113.7592462846896098, -285.1563676991896727, -261.4232467280049832 ) ) ;
#91359 = CARTESIAN_POINT ( 'NONE',  ( 35.42920495873281794, -281.8031003738838649, -276.7490280684600634 ) ) ;
#91360 = ORIENTED_EDGE ( 'NONE', *, *, #26082, .F. ) ;
#91361 = DIRECTION ( 'NONE',  ( 0.000000000000000000, 0.000000000000000000, -1.000000000000000000 ) ) ;
#91362 = CARTESIAN_POINT ( 'NONE',  ( -111.4370641330658884, -292.6143455651869658, -254.4826574411059994 ) ) ;
#91363 = VECTOR ( 'NONE', #36798, 1000.000000000000000 ) ;
#91364 = CARTESIAN_POINT ( 'NONE',  ( -92.44519403408897062, -289.9689683647503671, -217.2112604745847761 ) ) ;
#91365 = AXIS2_PLACEMENT_3D ( 'NONE', #47908, #76811, #11936 ) ;
#91366 = CARTESIAN_POINT ( 'NONE',  ( 34.12023193887684869, -274.8222826603795852, -286.4368627690673748 ) ) ;
#91367 = CARTESIAN_POINT ( 'NONE',  ( -66.89294582374272125, -294.7779473027160293, -341.3685172502521255 ) ) ;
#91368 = CARTESIAN_POINT ( 'NONE',  ( -32.08872379525112706, -290.5994559305301550, -196.8425005282266795 ) ) ;
#91369 = CARTESIAN_POINT ( 'NONE',  ( 16.88654316452136683, -292.5061405806956714, -320.7324554999404995 ) ) ;
#91370 = CARTESIAN_POINT ( 'NONE',  ( -90.87189489401639264, -291.0378026248541232, -320.6513421059987650 ) ) ;
#91371 = CARTESIAN_POINT ( 'NONE',  ( 41.08708295871279859, -293.9068999365417199, -430.6442049081568939 ) ) ;
#91372 = AXIS2_PLACEMENT_3D ( 'NONE', #42228, #33269, #27109 ) ;
#91373 = CARTESIAN_POINT ( 'NONE',  ( -70.98585459882744431, -291.4962940501667958, -337.3914955929608368 ) ) ;
#91374 = CARTESIAN_POINT ( 'NONE',  ( 37.61481403398626355, -291.4800287185485104, -264.7442319228222800 ) ) ;
#91375 = CARTESIAN_POINT ( 'NONE',  ( 34.76391171601918728, -295.2862059498849590, -249.6808263262046523 ) ) ;
#91376 = CARTESIAN_POINT ( 'NONE',  ( -79.45434985963177610, -286.4093413322513015, -210.3828023599744483 ) ) ;
#91377 = CARTESIAN_POINT ( 'NONE',  ( -50.12994296856311394, -297.2150176951487310, -344.4846158138618648 ) ) ;
#91378 = B_SPLINE_CURVE_WITH_KNOTS ( 'NONE', 3,
 ( #66522, #38069, #1641, #30521, #23429, #88735 ),
 .UNSPECIFIED., .F., .F.,
 ( 4, 2, 4 ),
 ( 0.000000000000000000, 0.0009572278725339521555, 0.001914455745067904311 ),
 .UNSPECIFIED. ) ;
#91379 = CARTESIAN_POINT ( 'NONE',  ( 27.08296080288267405, -277.0094941831310962, -231.1734411330798480 ) ) ;
#91380 = CARTESIAN_POINT ( 'NONE',  ( 23.19477141265485187, -274.9773544239545231, -317.3221813760087571 ) ) ;
#91381 = CIRCLE ( 'NONE', #43015, 4.025000000000000355 ) ;
#91382 = CARTESIAN_POINT ( 'NONE',  ( -37.59684428451090810, -297.2462054656445503, -193.5230172586575463 ) ) ;
#91383 = CARTESIAN_POINT ( 'NONE',  ( 12.41255121800860195, -274.5880988281972463, -325.2256112020459682 ) ) ;
#91384 = CARTESIAN_POINT ( 'NONE',  ( -84.32809708462389153, -277.4801400354160705, -212.5571462392275350 ) ) ;
#91385 = CARTESIAN_POINT ( 'NONE',  ( -38.10178674089300443, -275.2474962233858378, -196.9679795125657620 ) ) ;
#91386 = CARTESIAN_POINT ( 'NONE',  ( 35.17655009341229544, -273.8195672833140861, -246.1170485126670258 ) ) ;
#91387 = AXIS2_PLACEMENT_3D ( 'NONE', #34986, #21724, #6115 ) ;
#91388 = CARTESIAN_POINT ( 'NONE',  ( -50.55936929982452455, -296.6495469438519876, -342.7535771014049146 ) ) ;
#91389 = DIRECTION ( 'NONE',  ( 1.000000000000000000, 0.000000000000000000, 0.000000000000000000 ) ) ;
#91390 = CARTESIAN_POINT ( 'NONE',  ( -91.97226346387476781, -298.0492980665790697, -221.6979565887256456 ) ) ;
#91391 = CARTESIAN_POINT ( 'NONE',  ( 144.2857639756989272, -299.5541904835127980, -189.7068768330456123 ) ) ;
#91393 = CARTESIAN_POINT ( 'NONE',  ( -109.8855308749134565, -272.4929590503043073, -262.2129510063363114 ) ) ;
#91392 = CARTESIAN_POINT ( 'NONE',  ( 15.51390208675261206, -286.3298282326177855, -324.1429823475340299 ) ) ;
#91394 = CARTESIAN_POINT ( 'NONE',  ( -4.773947465373244547, -286.4693557288148895, -200.5876166622115306 ) ) ;
#91395 = CARTESIAN_POINT ( 'NONE',  ( -34.67180554375087809, -288.6861812110296910, -347.2936595661045658 ) ) ;
#91396 = CARTESIAN_POINT ( 'NONE',  ( -102.4418378916558368, -299.0378136671908464, -232.3059051094763845 ) ) ;
#91397 = CARTESIAN_POINT ( 'NONE',  ( -53.57119342235846915, -293.2605465335681174, -343.4666668331450410 ) ) ;
#91398 = CARTESIAN_POINT ( 'NONE',  ( 29.15197281433721344, -280.2475261933602724, -231.8546214042688121 ) ) ;
#91399 = CARTESIAN_POINT ( 'NONE',  ( 197.4836817735085219, 42.27872732282707346, 11.66666666666666785 ) ) ;
#91400 = CARTESIAN_POINT ( 'NONE',  ( -85.83314923546242881, -277.3809199723460779, -213.0785918205089331 ) ) ;
#91401 = CARTESIAN_POINT ( 'NONE',  ( 197.3748232817349049, 275.5000000000000568, -12.45182892472559821 ) ) ;
#91402 = CARTESIAN_POINT ( 'NONE',  ( -8.074190450822188225, -287.4550872398936576, -337.7247563930061460 ) ) ;
#91403 = DIRECTION ( 'NONE',  ( 0.000000000000000000, -1.000000000000000000, 0.000000000000000000 ) ) ;
#91404 = CARTESIAN_POINT ( 'NONE',  ( -45.60749175891414353, -287.1567656726519431, -344.9042419878641113 ) ) ;
#91405 = CARTESIAN_POINT ( 'NONE',  ( -88.69691714495186829, -298.9172910876927745, -217.2889761594862534 ) ) ;
#91406 = CARTESIAN_POINT ( 'NONE',  ( -3.140170789521716355, -284.0345894978480601, -338.7047296111546189 ) ) ;
#91408 = CARTESIAN_POINT ( 'NONE',  ( 35.51986069168074778, -281.4928733653972586, -265.8674607962465188 ) ) ;
#91407 = CARTESIAN_POINT ( 'NONE',  ( -36.53656519700641070, -296.0822964683450209, -195.0061795729632479 ) ) ;
#91409 = CARTESIAN_POINT ( 'NONE',  ( -29.94857384365038655, -275.5728354481232714, -197.1442032660336565 ) ) ;
#91410 = CARTESIAN_POINT ( 'NONE',  ( 35.74521643761639211, -285.8765823952537062, -289.5344543542438487 ) ) ;
#91411 = CARTESIAN_POINT ( 'NONE',  ( -3.320735039392577637, -282.5014870460266252, -203.5068572701394203 ) ) ;
#91412 = EDGE_CURVE ( 'NONE', #27913, #14834, #77140, .T. ) ;
#91413 = CARTESIAN_POINT ( 'NONE',  ( -92.24055986044469080, -272.1637059934034255, -221.7777743942119741 ) ) ;
#91414 = EDGE_LOOP ( 'NONE', ( #28351, #61989, #55267, #52806 ) ) ;
#91415 = LINE ( 'NONE', #75356, #63496 ) ;
#91416 = CARTESIAN_POINT ( 'NONE',  ( -3.230692910975983878, -294.4474816213648865, -339.4078823316145872 ) ) ;
#91417 = CARTESIAN_POINT ( 'NONE',  ( -102.4377971812799473, -287.0220629819997953, -233.7264399450374128 ) ) ;
#91418 = CARTESIAN_POINT ( 'NONE',  ( 207.2842799582832356, 30.47689859374760957, 11.99999999999999822 ) ) ;
#91419 = CARTESIAN_POINT ( 'NONE',  ( -115.3430155898818299, -281.8380690714489560, -288.1317622949166548 ) ) ;
#91420 = CARTESIAN_POINT ( 'NONE',  ( -99.52511600978857587, -277.1489645395939192, -315.5208588358211728 ) ) ;
#91421 = CARTESIAN_POINT ( 'NONE',  ( -65.17400966114645655, -287.8095927481670628, -341.3520853129774082 ) ) ;
#91422 = CARTESIAN_POINT ( 'NONE',  ( -76.47909747796536806, -285.1057547709830260, -332.8632061046549779 ) ) ;
#91423 = CARTESIAN_POINT ( 'NONE',  ( -36.43153153290948865, -278.8007696303426428, -344.3814981817356511 ) ) ;
#91424 = CARTESIAN_POINT ( 'NONE',  ( -110.1187585382362073, -285.6819420671899366, -293.6874052234516626 ) ) ;
#91425 = CARTESIAN_POINT ( 'NONE',  ( -29.41695064357652356, -281.7445980916448889, -343.3798948244461258 ) ) ;
#91426 = CARTESIAN_POINT ( 'NONE',  ( -71.88488443299729624, -281.5957443661278035, -203.7751089242213709 ) ) ;
#91427 = CARTESIAN_POINT ( 'NONE',  ( -58.12365645485358812, -273.9576432399149439, -196.1631927018343049 ) ) ;
#91428 = CARTESIAN_POINT ( 'NONE',  ( -111.4410944336392646, -278.1230939708128176, -291.2962503696851968 ) ) ;
#91429 = CARTESIAN_POINT ( 'NONE',  ( -110.2910888526954238, -298.2797381086804194, -285.2468074337051007 ) ) ;
#91430 = AXIS2_PLACEMENT_3D ( 'NONE', #46396, #17066, #25559 ) ;
#91431 = DIRECTION ( 'NONE',  ( 0.000000000000000000, 0.000000000000000000, -1.000000000000000000 ) ) ;
#91432 = EDGE_CURVE ( 'NONE', #51603, #72522, #16043, .T. ) ;
#91433 = CARTESIAN_POINT ( 'NONE',  ( 151.4851178187871312, 20.00000000000000000, -3.492110388858666870 ) ) ;
#91434 = CARTESIAN_POINT ( 'NONE',  ( -109.6273850336243640, -294.9835581504654556, -247.4918916308654104 ) ) ;
#91435 = CARTESIAN_POINT ( 'NONE',  ( 33.57042190436544615, -274.8278629516498199, -252.7696600922499499 ) ) ;
#91436 = CARTESIAN_POINT ( 'NONE',  ( -109.7316728875863419, -274.0747173661319493, -245.3071649613955287 ) ) ;
#91437 = CARTESIAN_POINT ( 'NONE',  ( 34.98149332624754493, -289.1076732822409099, -254.6343985227521500 ) ) ;
#91438 =( GEOMETRIC_REPRESENTATION_CONTEXT ( 3 ) GLOBAL_UNCERTAINTY_ASSIGNED_CONTEXT ( ( #70329 ) ) GLOBAL_UNIT_ASSIGNED_CONTEXT ( ( #7172, #77265, #63088 ) ) REPRESENTATION_CONTEXT ( 'NONE', 'WORKASPACE' ) );
#91439 = CARTESIAN_POINT ( 'NONE',  ( -33.45065499230291550, -296.5241534160896890, -346.5815171601796010 ) ) ;
#91440 = CARTESIAN_POINT ( 'NONE',  ( 37.66993831308591467, -294.5611509607925314, -254.7642519674529353 ) ) ;
#91441 = CARTESIAN_POINT ( 'NONE',  ( -91.91266301801832128, -291.8327591059735937, -321.6426059308977869 ) ) ;
#91442 = CARTESIAN_POINT ( 'NONE',  ( -101.0145819251898018, -277.0820326412294321, -230.9457474183267323 ) ) ;
#91443 = CARTESIAN_POINT ( 'NONE',  ( -109.0112319980739102, -280.7336544809712677, -250.1943641411609178 ) ) ;
#91444 = CARTESIAN_POINT ( 'NONE',  ( -83.26705830995341273, -293.7662832120388998, -329.0116276548634460 ) ) ;
#91445 = CARTESIAN_POINT ( 'NONE',  ( 8.480889543366975758, -284.2925163690293289, -330.6984675567716749 ) ) ;
#91446 = CIRCLE ( 'NONE', #9810, 8.000000000000000000 ) ;
#91447 = CARTESIAN_POINT ( 'NONE',  ( -37.26680993935310227, -284.9734014890042886, -197.0395521222929176 ) ) ;
#91448 = CARTESIAN_POINT ( 'NONE',  ( 162.9306247839069215, 218.7636628492012107, -204.5803896349958109 ) ) ;
#91449 = ORIENTED_EDGE ( 'NONE', *, *, #22764, .T. ) ;
#91450 = CARTESIAN_POINT ( 'NONE',  ( -68.78019434174719038, -285.2938222749552324, -204.4405076615336441 ) ) ;
#91451 = ORIENTED_EDGE ( 'NONE', *, *, #37177, .F. ) ;
#91452 = CARTESIAN_POINT ( 'NONE',  ( 39.40104397242586742, -282.6262614602422332, -269.9182741761944726 ) ) ;
#91453 = CARTESIAN_POINT ( 'NONE',  ( -107.9616278149003676, -273.1329137884198417, -251.5953418252914844 ) ) ;
#91454 = CARTESIAN_POINT ( 'NONE',  ( -60.37582708712996293, -284.5550092692473640, -197.2480630011450558 ) ) ;
#91455 = CARTESIAN_POINT ( 'NONE',  ( -2.507655499072967142, -281.4427498508011354, -201.9402264107646374 ) ) ;
#91456 = CARTESIAN_POINT ( 'NONE',  ( -22.71818901303054616, -281.7560159376803313, -195.4150260402975334 ) ) ;
#91457 = CARTESIAN_POINT ( 'NONE',  ( 23.66136972373545433, -281.5779690507591226, -223.5214694981244747 ) ) ;
#91458 = CARTESIAN_POINT ( 'NONE',  ( -67.74223827176246004, -280.9809262143061233, -333.4151289067050357 ) ) ;
#91459 = CARTESIAN_POINT ( 'NONE',  ( -89.20268650580214853, -231.0846910060161576, -347.9280380252721443 ) ) ;
#91460 = ORIENTED_EDGE ( 'NONE', *, *, #89262, .F. ) ;
#91461 = CARTESIAN_POINT ( 'NONE',  ( -91.54158464531045070, -275.2782973075043174, -218.7439046091689363 ) ) ;
#91462 = CARTESIAN_POINT ( 'NONE',  ( -114.2130971324556441, -273.2892385179353028, -270.3705028573608615 ) ) ;
#91463 = CARTESIAN_POINT ( 'NONE',  ( -107.0412691870660922, -276.9229084974386410, -243.4991220509693335 ) ) ;
#91464 = CARTESIAN_POINT ( 'NONE',  ( -2.540179950329658709, -294.2661110412163907, -202.7978267517777908 ) ) ;
#91465 = CARTESIAN_POINT ( 'NONE',  ( -66.10086824468920952, -294.7873696022830927, -337.5682821665109827 ) ) ;
#91466 = CARTESIAN_POINT ( 'NONE',  ( -5.906338203719967872, -291.9620620304044110, -200.1233049616625124 ) ) ;
#91467 = CARTESIAN_POINT ( 'NONE',  ( -88.01845085739296337, -229.9137135291527159, -344.5856900492037767 ) ) ;
#91469 = CARTESIAN_POINT ( 'NONE',  ( 28.93739615278737531, -286.3869320849117344, -302.8191186786874596 ) ) ;
#91468 = CARTESIAN_POINT ( 'NONE',  ( -113.1876926100662075, -295.2437508701562479, -261.0879461010388241 ) ) ;
#91470 = CARTESIAN_POINT ( 'NONE',  ( 18.92387230723247171, -296.0908895032135320, -318.8062327677308190 ) ) ;
#91471 = CARTESIAN_POINT ( 'NONE',  ( 36.17413427506936330, -286.2101645750043986, -268.3153303142756840 ) ) ;
#91472 = CARTESIAN_POINT ( 'NONE',  ( -85.17011665110520369, -285.0442949659156966, -326.1615306116070201 ) ) ;
#91473 = EDGE_LOOP ( 'NONE', ( #14171, #79527, #81972, #66135, #46238, #84108 ) ) ;
#91474 = CARTESIAN_POINT ( 'NONE',  ( -47.72347311982773022, -292.8646121133641032, -194.2480429103480333 ) ) ;
#91475 = CARTESIAN_POINT ( 'NONE',  ( -51.02327871930491199, -283.7239513089365914, -342.1818311753037278 ) ) ;
#91476 = CARTESIAN_POINT ( 'NONE',  ( -113.9694323779194605, -295.3208984764758611, -272.4436056596489948 ) ) ;
#91477 = CARTESIAN_POINT ( 'NONE',  ( -111.8405351030341848, -291.5915210528933130, -251.4910140995811787 ) ) ;
#91478 = CARTESIAN_POINT ( 'NONE',  ( -25.03746414870094128, -292.6973995371104706, -194.4128943032258690 ) ) ;
#91479 = CARTESIAN_POINT ( 'NONE',  ( 28.80905960562859747, -287.3019639123954789, -239.4891729331150714 ) ) ;
#91480 = VERTEX_POINT ( 'NONE', #20786 ) ;
#91481 = CARTESIAN_POINT ( 'NONE',  ( 160.6539576904058606, 293.9636489450775230, 0.000000000000000000 ) ) ;
#91482 = CARTESIAN_POINT ( 'NONE',  ( -81.13806443618545927, -297.5001987460254895, -332.2489965217478129 ) ) ;
#91483 = CARTESIAN_POINT ( 'NONE',  ( -14.97251956371161263, -297.0115246069310615, -193.8591426424625865 ) ) ;
#91484 = CARTESIAN_POINT ( 'NONE',  ( -71.03929899225272493, -278.6548075280031185, -205.3248338465427025 ) ) ;
#91485 = CARTESIAN_POINT ( 'NONE',  ( 22.71425433338012212, -274.4148920279678237, -222.2485482977347715 ) ) ;
#91486 = CARTESIAN_POINT ( 'NONE',  ( 1.538203921088562742, -278.3873637134157661, -333.6609051914350630 ) ) ;
#91487 = CARTESIAN_POINT ( 'NONE',  ( 19.96727743928017063, -273.0341798151374064, -223.1748215228151935 ) ) ;
#91488 = CARTESIAN_POINT ( 'NONE',  ( -10.32966836467748628, -295.8966728383643954, -338.6068551764698782 ) ) ;
#91489 = CARTESIAN_POINT ( 'NONE',  ( -95.54283132745888452, -298.2564638759285458, -225.7665143323638972 ) ) ;
#91490 = CARTESIAN_POINT ( 'NONE',  ( -47.50449942084240007, -296.7794073300615878, -345.8803733062347874 ) ) ;
#91491 = CARTESIAN_POINT ( 'NONE',  ( -92.91484279393951340, -271.2798075829547884, -219.4497106490539693 ) ) ;
#91492 = CARTESIAN_POINT ( 'NONE',  ( -33.51137945871451507, -292.7530184164127149, -197.3470924747991546 ) ) ;
#91493 = CARTESIAN_POINT ( 'NONE',  ( -95.42676766480094841, -288.4951942623794707, -315.5644434295701899 ) ) ;
#91494 = DIRECTION ( 'NONE',  ( 0.000000000000000000, 0.000000000000000000, 1.000000000000000000 ) ) ;
#91495 = CARTESIAN_POINT ( 'NONE',  ( 36.52500573981465948, -275.7722603408423652, -248.6520603133711518 ) ) ;
#91496 = CARTESIAN_POINT ( 'NONE',  ( -84.09162628998343791, -297.7223299358935833, -214.2011407828729261 ) ) ;
#91497 = CARTESIAN_POINT ( 'NONE',  ( -61.54375299023272561, -281.7193171916490542, -198.9431522441431923 ) ) ;
#91498 = CARTESIAN_POINT ( 'NONE',  ( 37.06481366238827491, -280.4617349392677284, -288.2205692750201251 ) ) ;
#91499 = CARTESIAN_POINT ( 'NONE',  ( -70.26491466348439019, -276.8232310769152491, -339.8692397099854361 ) ) ;
#91500 = CARTESIAN_POINT ( 'NONE',  ( -7.196263891439274474, -281.8434792663929898, -337.0371020368896779 ) ) ;
#91501 = CARTESIAN_POINT ( 'NONE',  ( 8.080217619880164293, -280.4325612955711335, -330.2516665827125166 ) ) ;
#91502 = ADVANCED_FACE ( 'NONE', ( #6591 ), #6116, .T. ) ;
#91503 = CARTESIAN_POINT ( 'NONE',  ( 11.95459705568524456, -273.3277364390233402, -215.6550468585326712 ) ) ;
#91504 = CARTESIAN_POINT ( 'NONE',  ( -6.857282316264694089, -278.6522482819830770, -338.9001472053624866 ) ) ;
#91505 = CARTESIAN_POINT ( 'NONE',  ( 209.6287663260175975, 29.00782453271232697, 10.50000000000000000 ) ) ;
#91506 = DIRECTION ( 'NONE',  ( 1.000000000000000000, 0.000000000000000000, 0.000000000000000000 ) ) ;
#91507 = CARTESIAN_POINT ( 'NONE',  ( -45.99197099733657979, -296.1837418153170916, -194.8684241207276955 ) ) ;
#91508 = CARTESIAN_POINT ( 'NONE',  ( -109.4738409625824005, -290.8946200070876671, -243.2656314837360298 ) ) ;
#91509 = CARTESIAN_POINT ( 'NONE',  ( 7.176259856942059479, -278.4478500041583402, -330.9910744772145108 ) ) ;
#91510 = CARTESIAN_POINT ( 'NONE',  ( 21.43844668523864172, -272.9118451248900215, -223.7584271836043683 ) ) ;
#91511 = FACE_OUTER_BOUND ( 'NONE', #58221, .T. ) ;
#91512 = CARTESIAN_POINT ( 'NONE',  ( -99.81985490410760065, -287.0443997037538111, -227.7740099923798027 ) ) ;
#91513 = ORIENTED_EDGE ( 'NONE', *, *, #250, .T. ) ;
#91514 = DIRECTION ( 'NONE',  ( -0.000000000000000000, 1.000000000000000000, -0.000000000000000000 ) ) ;
#91515 = CARTESIAN_POINT ( 'NONE',  ( 17.49309829754145440, -286.2684429627485088, -321.5476067367169435 ) ) ;
#91516 = DIRECTION ( 'NONE',  ( 0.000000000000000000, 0.000000000000000000, -1.000000000000000000 ) ) ;
#91517 = CARTESIAN_POINT ( 'NONE',  ( -39.71718064777807200, -293.8775345210710270, -343.7322390492487330 ) ) ;
#91518 = CARTESIAN_POINT ( 'NONE',  ( 23.00937639164871129, -285.0966077774099290, -227.0469595182767080 ) ) ;
#91519 = CARTESIAN_POINT ( 'NONE',  ( 157.7670607448636702, 18.75975317436435574, -10.28854280544447697 ) ) ;
#91520 = CARTESIAN_POINT ( 'NONE',  ( -66.86320858918466570, -293.4388402704298642, -339.3066123174010613 ) ) ;
#91521 = CARTESIAN_POINT ( 'NONE',  ( 15.83005975248296160, -285.2688731667498701, -215.6302153513252335 ) ) ;
#91522 = CARTESIAN_POINT ( 'NONE',  ( -110.4168739231098044, -280.2915565306478811, -259.6879277718881553 ) ) ;
#91523 = CARTESIAN_POINT ( 'NONE',  ( 29.77621589810125968, -288.2753172226339871, -233.3296375582851852 ) ) ;
#91524 = CARTESIAN_POINT ( 'NONE',  ( 36.87094569955860379, -279.9996485591304349, -286.7446456762218077 ) ) ;
#91525 = CARTESIAN_POINT ( 'NONE',  ( -66.32902935581385861, -289.4424156244938331, -337.4131546158085371 ) ) ;
#91526 = CARTESIAN_POINT ( 'NONE',  ( -65.05470993436355798, -281.1080922550962669, -202.1895402891388756 ) ) ;
#91527 = CARTESIAN_POINT ( 'NONE',  ( 11.40582208700768518, -281.5517825427929779, -215.8058175580083287 ) ) ;
#91528 = CARTESIAN_POINT ( 'NONE',  ( -33.82975818805260815, -288.0760300475851636, -195.0877955600566622 ) ) ;
#91529 = ORIENTED_EDGE ( 'NONE', *, *, #93048, .T. ) ;
#91530 = CARTESIAN_POINT ( 'NONE',  ( -15.77735919573738954, -274.3235032201508261, -196.3870452591940250 ) ) ;
#91531 = CARTESIAN_POINT ( 'NONE',  ( -108.1391329845408222, -292.8392824673886139, -246.7058795961908118 ) ) ;
#91532 = DIRECTION ( 'NONE',  ( 0.000000000000000000, 1.000000000000000000, 0.000000000000000000 ) ) ;
#91533 = CARTESIAN_POINT ( 'NONE',  ( -112.3452863284742875, -275.1604526064900824, -261.9424758988611188 ) ) ;
#91534 = ORIENTED_EDGE ( 'NONE', *, *, #48886, .F. ) ;
#91535 = CARTESIAN_POINT ( 'NONE',  ( -4.601070507658654662, -272.4822888427931957, -202.6854445685419819 ) ) ;
#91536 = DIRECTION ( 'NONE',  ( 0.000000000000000000, 1.000000000000000000, 0.000000000000000000 ) ) ;
#91537 = CARTESIAN_POINT ( 'NONE',  ( -76.68680171292136549, -293.9689646864444512, -335.6789566600926946 ) ) ;
#91538 = CARTESIAN_POINT ( 'NONE',  ( -104.8166454803574794, -296.4352407168179866, -242.3411217084400562 ) ) ;
#91539 = MANIFOLD_SOLID_BREP ( 'Fillet14', #41575 ) ;
#91540 = CARTESIAN_POINT ( 'NONE',  ( -3.026432016498052491, -290.1106147667691744, -335.6339768666276200 ) ) ;
#91541 = CARTESIAN_POINT ( 'NONE',  ( 14.65228333007634554, -284.0684307898442285, -323.1077696386612388 ) ) ;
#91542 = CARTESIAN_POINT ( 'NONE',  ( -54.35264091286074262, -290.6916595935194891, -344.9085905796628140 ) ) ;
#91543 = CARTESIAN_POINT ( 'NONE',  ( -111.1614163470662504, -292.1212322598742617, -250.2129138352427447 ) ) ;
#91544 = CARTESIAN_POINT ( 'NONE',  ( -98.21256529863494222, -287.1488889457705227, -226.5243796244758130 ) ) ;
#91545 = CARTESIAN_POINT ( 'NONE',  ( -59.30417266740785465, -279.9421459336763860, -196.5596965568990981 ) ) ;
#91546 = CARTESIAN_POINT ( 'NONE',  ( -85.49675451179396646, -293.7919961329496346, -328.5883017756792128 ) ) ;
#91547 = CARTESIAN_POINT ( 'NONE',  ( -74.27785059713075100, -283.3621963305916438, -337.9833280790210779 ) ) ;
#91548 = CARTESIAN_POINT ( 'NONE',  ( 28.95392921547570708, -276.9667457095656005, -236.9581988374690411 ) ) ;
#91549 = CARTESIAN_POINT ( 'NONE',  ( 31.03373250439201669, -301.4082689599840705, -195.3320873922940848 ) ) ;
#91550 = CARTESIAN_POINT ( 'NONE',  ( 14.17943005956878189, -274.5805609200348840, -326.2856185780856890 ) ) ;
#91551 = DIRECTION ( 'NONE',  ( 0.000000000000000000, 0.000000000000000000, 1.000000000000000000 ) ) ;
#91552 = CARTESIAN_POINT ( 'NONE',  ( 25.60887001799556728, -281.5699379870615076, -307.5449553459628760 ) ) ;
#91553 = CARTESIAN_POINT ( 'NONE',  ( -71.38054830402484185, -278.6967495891598787, -338.9859351782491785 ) ) ;
#91554 = CARTESIAN_POINT ( 'NONE',  ( -36.55576499275309033, -285.1205429722402869, -193.5874352143536612 ) ) ;
#91555 = CARTESIAN_POINT ( 'NONE',  ( -73.13641183575981586, -293.3313159366523450, -205.5214786443138451 ) ) ;
#91556 = CARTESIAN_POINT ( 'NONE',  ( -102.0505484084054046, -274.6842044202846296, -230.1217669854655128 ) ) ;
#91557 = CARTESIAN_POINT ( 'NONE',  ( -78.58985866657772590, -274.8242253368149477, -205.9259747048038491 ) ) ;
#91558 = CARTESIAN_POINT ( 'NONE',  ( 197.2116943569230330, 250.5000000000000568, -12.42446933126074882 ) ) ;
#91559 = CARTESIAN_POINT ( 'NONE',  ( -6.278554105478609593, -276.4656431564644663, -336.4360772835125317 ) ) ;
#91560 = CARTESIAN_POINT ( 'NONE',  ( -111.8787855641530484, -298.6451428517201521, -263.1476459874509715 ) ) ;
#91561 = CARTESIAN_POINT ( 'NONE',  ( -69.54127732539646445, -283.6272128542339033, -202.7954072085723283 ) ) ;
#91562 = CARTESIAN_POINT ( 'NONE',  ( 26.47775162097885016, -292.6504917385881299, -227.2229252906625163 ) ) ;
#91563 = CARTESIAN_POINT ( 'NONE',  ( 12.83511596333008775, -274.3683832450362274, -325.6954536688811572 ) ) ;
#91564 = CARTESIAN_POINT ( 'NONE',  ( -37.47947447601243454, -290.6539350619147513, -346.5739325317918542 ) ) ;
#91565 = EDGE_CURVE ( 'NONE', #36764, #16269, #21726, .T. ) ;
#91566 = CARTESIAN_POINT ( 'NONE',  ( 13.12587306266063081, -291.6981549386446773, -217.1892256963067211 ) ) ;
#91567 = ORIENTED_EDGE ( 'NONE', *, *, #56930, .F. ) ;
#91568 = CARTESIAN_POINT ( 'NONE',  ( -41.99977039435461990, -290.5692526024471363, -194.0924568252665949 ) ) ;
#91569 = CARTESIAN_POINT ( 'NONE',  ( -106.0539009480764321, -289.8898351486674869, -295.0738868522901157 ) ) ;
#91570 = ORIENTED_EDGE ( 'NONE', *, *, #70292, .T. ) ;
#91571 = CARTESIAN_POINT ( 'NONE',  ( 30.09744879894085301, -289.1073502841383629, -306.9887024118148702 ) ) ;
#91572 = CARTESIAN_POINT ( 'NONE',  ( -93.95961154558501960, -279.5379800872693181, -224.2471331884474353 ) ) ;
#91573 = EDGE_CURVE ( 'NONE', #59550, #39273, #28163, .T. ) ;
#91574 = CARTESIAN_POINT ( 'NONE',  ( -79.31930809994936737, -294.5249612173482205, -334.5434593091197826 ) ) ;
#91575 = CARTESIAN_POINT ( 'NONE',  ( -10.03792312476201332, -287.0507189585259198, -198.4168679114301597 ) ) ;
#91576 = CARTESIAN_POINT ( 'NONE',  ( -113.4671669276836781, -285.0328249901880895, -258.5789369413884060 ) ) ;
#91577 = CARTESIAN_POINT ( 'NONE',  ( -32.13996031343946669, -283.3180107188272245, -343.1967506749186327 ) ) ;
#91578 = CARTESIAN_POINT ( 'NONE',  ( -110.2157014284088206, -266.9174177228133544, -307.0198616398569129 ) ) ;
#91579 = CARTESIAN_POINT ( 'NONE',  ( -108.4223761982444358, -261.1587273596273349, -317.0417516531400679 ) ) ;
#91580 = CARTESIAN_POINT ( 'NONE',  ( -63.66200778950266681, -182.2673717872931718, -358.7378838168659740 ) ) ;
#91581 = CARTESIAN_POINT ( 'NONE',  ( 11.66224941634359702, -273.9500759587870107, -215.9678109672791493 ) ) ;
#91582 = CARTESIAN_POINT ( 'NONE',  ( 9.852595745083579715, -275.3043725013017706, -326.4585734480855876 ) ) ;
#91583 = CARTESIAN_POINT ( 'NONE',  ( -100.6964262628418822, -296.6368665958761426, -226.6835801233826544 ) ) ;
#91584 = CARTESIAN_POINT ( 'NONE',  ( 190.0960685029364186, 268.0118023413412516, -137.8165032444274232 ) ) ;
#91585 = CARTESIAN_POINT ( 'NONE',  ( 36.01581549171817187, -274.5118220894777892, -292.1322483152757172 ) ) ;
#91586 = CARTESIAN_POINT ( 'NONE',  ( -108.9258722442364586, -274.5595422837134834, -251.3579791469701092 ) ) ;
#91587 = ORIENTED_EDGE ( 'NONE', *, *, #4532, .T. ) ;
#91588 = CARTESIAN_POINT ( 'NONE',  ( -85.07949011988362997, -298.3525370706499871, -210.2451997996368789 ) ) ;
#91589 = AXIS2_PLACEMENT_3D ( 'NONE', #44309, #14983, #50497 ) ;
#91590 = CARTESIAN_POINT ( 'NONE',  ( -31.86048534033557189, -289.4736123481187064, -343.2674270434939103 ) ) ;
#91591 = PRODUCT_DEFINITION ( 'UNKNOWN', '', #62834, #28627 ) ;
#91592 = CARTESIAN_POINT ( 'NONE',  ( -39.09388820444630142, -295.8764454847183742, -347.1796616945701999 ) ) ;
#91593 = CARTESIAN_POINT ( 'NONE',  ( -99.04684290866012475, -297.6564628810481281, -224.3826016525354987 ) ) ;
#91594 = CARTESIAN_POINT ( 'NONE',  ( -17.43463496833863857, -292.4828236523838996, -200.0752807098855612 ) ) ;
#91595 = ORIENTED_EDGE ( 'NONE', *, *, #81578, .F. ) ;
#91596 = CARTESIAN_POINT ( 'NONE',  ( 38.26673009654518154, -277.4821339957850341, -271.1320804500407462 ) ) ;
#91597 = ORIENTED_EDGE ( 'NONE', *, *, #48446, .T. ) ;
#91598 = CARTESIAN_POINT ( 'NONE',  ( 19.11926616122301681, -280.3473024399932569, -218.0955825990215544 ) ) ;
#91599 = CARTESIAN_POINT ( 'NONE',  ( -21.59077009152522919, -277.7866273271833961, -341.9347218537813546 ) ) ;
#91600 = CARTESIAN_POINT ( 'NONE',  ( -1.919964192950602166, -278.3496514733835738, -337.5866684754669791 ) ) ;
#91601 = CARTESIAN_POINT ( 'NONE',  ( -112.1369473547592008, -276.4497868026714968, -279.9447579437610329 ) ) ;
#91602 = CARTESIAN_POINT ( 'NONE',  ( -79.79397176477503706, -298.1122816857189264, -210.8489570339458226 ) ) ;
#91603 = CARTESIAN_POINT ( 'NONE',  ( -104.2467940553128471, -295.5383155970454254, -239.5940671088083889 ) ) ;
#91604 = CARTESIAN_POINT ( 'NONE',  ( 219.8344101925596021, 3.000000000000000000, 9.000000000000001776 ) ) ;
#91605 = CARTESIAN_POINT ( 'NONE',  ( -68.65322629069373761, -280.1439077479072921, -200.0679039868539917 ) ) ;
#91606 = CARTESIAN_POINT ( 'NONE',  ( -99.17396301451606178, -278.1818461641130966, -309.2598048186122242 ) ) ;
#91607 =( REPRESENTATION_RELATIONSHIP ('NONE','NONE', #78428, #71246 ) REPRESENTATION_RELATIONSHIP_WITH_TRANSFORMATION ( #33591 )SHAPE_REPRESENTATION_RELATIONSHIP( ) );
#91608 = CARTESIAN_POINT ( 'NONE',  ( 0.4609520040583713896, -287.2445834700441765, -336.9360728893208830 ) ) ;
#91609 = CARTESIAN_POINT ( 'NONE',  ( -36.24417668106679002, -300.0660164118279454, -195.1940694812736581 ) ) ;
#91610 = DIRECTION ( 'NONE',  ( 1.124465274301078034E-16, 1.000000000000000000, 0.000000000000000000 ) ) ;
#91611 = CARTESIAN_POINT ( 'NONE',  ( -29.16520366839402101, -288.1430477874945382, -343.0642584406153901 ) ) ;
#91612 = CARTESIAN_POINT ( 'NONE',  ( -67.70174011012508686, -277.8880789417145252, -202.8473845359850145 ) ) ;
#91614 = CARTESIAN_POINT ( 'NONE',  ( -48.56954327302700136, -281.2760509465280734, -343.9494984108547442 ) ) ;
#91613 = CARTESIAN_POINT ( 'NONE',  ( -96.87176147297223849, -277.7275030896753378, -227.0997412772513542 ) ) ;
#91615 = CARTESIAN_POINT ( 'NONE',  ( 7.727946979128574867, -288.6671836073599593, -210.3491585421080856 ) ) ;
#91616 = CARTESIAN_POINT ( 'NONE',  ( -106.8255794051055148, -280.0716171944793018, -246.5592039537742721 ) ) ;
#91617 = CARTESIAN_POINT ( 'NONE',  ( 153.8045260737213482, 20.39559083867290568, 12.88430403588788842 ) ) ;
#91618 = CARTESIAN_POINT ( 'NONE',  ( 11.94451510271255223, -294.7373705039797187, -213.8290948968864313 ) ) ;
#91619 = CARTESIAN_POINT ( 'NONE',  ( -112.0731805711758824, -276.6167981050014077, -284.1869860743988170 ) ) ;
#91620 = CARTESIAN_POINT ( 'NONE',  ( 32.61634922327148445, -276.4845052686296185, -291.6121676816976560 ) ) ;
#91621 = CARTESIAN_POINT ( 'NONE',  ( 31.48381616399933236, -283.1575354268622959, -240.1439584408999508 ) ) ;
#91622 = ADVANCED_FACE ( 'NONE', ( #73766, #66211 ), #58638, .F. ) ;
#91623 = ADVANCED_FACE ( 'NONE', ( #51502 ), #8457, .T. ) ;
#91624 = CARTESIAN_POINT ( 'NONE',  ( 196.8320172978770870, 70.49480016127409954, 10.86682040754346090 ) ) ;
#91625 = CARTESIAN_POINT ( 'NONE',  ( -84.25118808361536082, -291.6113564657768507, -329.6631017887759185 ) ) ;
#91626 = CARTESIAN_POINT ( 'NONE',  ( -66.51375320186078000, -293.4338849471275239, -339.5097269361399412 ) ) ;
#91627 = CARTESIAN_POINT ( 'NONE',  ( -110.9562215495007109, -283.4718440125857342, -292.4309300503533109 ) ) ;
#91628 = CARTESIAN_POINT ( 'NONE',  ( 208.1728644033713636, 30.17484991538838912, 14.33122224313838800 ) ) ;
#91629 = CARTESIAN_POINT ( 'NONE',  ( -72.12645278304323426, -272.2671343253006739, -205.5644431610330400 ) ) ;
#91630 = CARTESIAN_POINT ( 'NONE',  ( -30.67280933041948998, -290.2769392037974399, -196.4260696246104203 ) ) ;
#91631 = CARTESIAN_POINT ( 'NONE',  ( 197.7051530045995094, 41.80213891112347113, 12.00000000000000888 ) ) ;
#91632 = CARTESIAN_POINT ( 'NONE',  ( -73.09159571276958900, -290.0670039747904525, -202.9323145836915501 ) ) ;
#91633 = CARTESIAN_POINT ( 'NONE',  ( -42.75290109789580839, -287.5829069618486074, -196.7469999284384414 ) ) ;
#91634 = CARTESIAN_POINT ( 'NONE',  ( 33.91190192797236591, -285.4538162053688097, -243.9622883441582246 ) ) ;
#91635 = CARTESIAN_POINT ( 'NONE',  ( -57.57366874214088881, -287.2112103157493266, -199.5546844910101356 ) ) ;
#91636 = DIRECTION ( 'NONE',  ( -1.000000000000000000, 0.000000000000000000, 0.000000000000000000 ) ) ;
#91637 = CARTESIAN_POINT ( 'NONE',  ( -103.6361057395393885, -285.7733673289069429, -239.2950097593211751 ) ) ;
#91638 = CARTESIAN_POINT ( 'NONE',  ( 26.64214457312336748, -294.9988019725332720, -230.4571164693560945 ) ) ;
#91639 = CARTESIAN_POINT ( 'NONE',  ( 37.50127350561799489, -273.4996481698258890, -259.9763456916354585 ) ) ;
#91640 = CARTESIAN_POINT ( 'NONE',  ( 18.89066463898398851, -276.6026274741958559, -322.9316938232645384 ) ) ;
#91641 = CARTESIAN_POINT ( 'NONE',  ( 5.696469485077396477, -290.7101971354200600, -208.2561250100925747 ) ) ;
#91642 = CARTESIAN_POINT ( 'NONE',  ( -112.7936298316086976, -278.3592080234463424, -285.7887752910229437 ) ) ;
#91643 = CARTESIAN_POINT ( 'NONE',  ( -35.58723491855735688, -297.0099543659138703, -344.9980781415468982 ) ) ;
#91644 = CARTESIAN_POINT ( 'NONE',  ( -43.53335306050103526, -248.9569719664657157, -480.6442262660607980 ) ) ;
#91645 = DIRECTION ( 'NONE',  ( 0.000000000000000000, 0.000000000000000000, -1.000000000000000000 ) ) ;
#91646 = CARTESIAN_POINT ( 'NONE',  ( -102.6691503550455593, -283.6916143707038600, -236.6926204891089185 ) ) ;
#91647 = CARTESIAN_POINT ( 'NONE',  ( 20.44641471730726678, -278.8922418264461953, -222.5538545683616860 ) ) ;
#91648 = DIRECTION ( 'NONE',  ( -0.000000000000000000, -1.000000000000000000, -0.000000000000000000 ) ) ;
#91649 = CARTESIAN_POINT ( 'NONE',  ( -4.110393303378095275, -272.9622495973496257, -201.6562146196084484 ) ) ;
#91650 = CARTESIAN_POINT ( 'NONE',  ( -71.70943302926131935, -276.8675170919686366, -334.8946273709447610 ) ) ;
#91651 = AXIS2_PLACEMENT_3D ( 'NONE', #55263, #26839, #49084 ) ;
#91652 = CARTESIAN_POINT ( 'NONE',  ( -42.41834566421157859, -296.6374639314518049, -343.8793838968330761 ) ) ;
#91653 = CARTESIAN_POINT ( 'NONE',  ( 32.89537836024536688, -280.0781992771161413, -239.5675258839310686 ) ) ;
#91654 = CARTESIAN_POINT ( 'NONE',  ( 16.33974101785182853, -295.2070978176341214, -320.1778955255865071 ) ) ;
#91655 = CARTESIAN_POINT ( 'NONE',  ( -16.62421798375591209, -296.1052394823257146, -344.0643831288477372 ) ) ;
#91656 = CARTESIAN_POINT ( 'NONE',  ( -95.28777342368346126, -297.0103140906840622, -225.9419603996430226 ) ) ;
#91657 = CARTESIAN_POINT ( 'NONE',  ( -110.3808649490486005, -292.7717898374029346, -253.2673950070856677 ) ) ;
#91658 = CARTESIAN_POINT ( 'NONE',  ( -91.90448717070616169, -285.4661207114720582, -216.0297064912361691 ) ) ;
#91659 = CARTESIAN_POINT ( 'NONE',  ( -8.379090772105486806, -274.8166112892657225, -340.3856901209849752 ) ) ;
#91660 = CARTESIAN_POINT ( 'NONE',  ( -34.66894647719743716, -288.8527554178075434, -347.3147169396272602 ) ) ;
#91661 = CARTESIAN_POINT ( 'NONE',  ( -16.48578085765428369, -282.3028996450793784, -198.6891050937911984 ) ) ;
#91662 = CARTESIAN_POINT ( 'NONE',  ( 20.53394647460082822, -285.9808768801356109, -225.4855346527272673 ) ) ;
#91663 = CARTESIAN_POINT ( 'NONE',  ( -63.66242236807559607, -289.7090353403514769, -200.0766450495821687 ) ) ;
#91664 = CARTESIAN_POINT ( 'NONE',  ( 202.1133578493929974, 280.9843981858382449, -111.1516734208197050 ) ) ;
#91665 = CARTESIAN_POINT ( 'NONE',  ( -5.766379998217369796, -285.9864818107648148, -204.4611503838049771 ) ) ;
#91666 = DIRECTION ( 'NONE',  ( -0.000000000000000000, -0.000000000000000000, 1.000000000000000000 ) ) ;
#91667 = CARTESIAN_POINT ( 'NONE',  ( -16.19511271854763024, -283.7266386584992688, -344.2108313378158186 ) ) ;
#91668 = CARTESIAN_POINT ( 'NONE',  ( -64.29492612794344097, -290.7677730558818894, -198.4278374441607582 ) ) ;
#91669 = CARTESIAN_POINT ( 'NONE',  ( 38.00056594634853724, -283.0038771750467390, -258.6184678580630134 ) ) ;
#91670 = CARTESIAN_POINT ( 'NONE',  ( -110.9613867094538904, -279.6047086496683960, -291.1803403766498946 ) ) ;
#91671 = CARTESIAN_POINT ( 'NONE',  ( 35.35255650702463726, -281.2903900979920877, -263.1534556928802999 ) ) ;
#91672 = CARTESIAN_POINT ( 'NONE',  ( -16.09790370714123497, -276.3268667571045398, -198.3785230062812843 ) ) ;
#91673 = CARTESIAN_POINT ( 'NONE',  ( -70.80787226600439510, -295.4813837412916087, -339.7226923413282975 ) ) ;
#91674 = CARTESIAN_POINT ( 'NONE',  ( -84.85707358039164205, -289.4131982856992522, -212.7925841703364824 ) ) ;
#91675 =( BOUNDED_CURVE ( )  B_SPLINE_CURVE ( 3, ( #814, #16862, #51906, #15946 ),
 .UNSPECIFIED., .F., .F. ) 
 B_SPLINE_CURVE_WITH_KNOTS ( ( 4, 4 ),
 ( 4.712388980384689674, 5.553457650952617008 ),
 .UNSPECIFIED. ) 
 CURVE ( )  GEOMETRIC_REPRESENTATION_ITEM ( )  RATIONAL_B_SPLINE_CURVE ( ( 1.000000000000000000, 0.9419139527835183046, 0.9419139527835183046, 1.000000000000000000 ) ) 
 REPRESENTATION_ITEM ( '' )  );
#91676 = CARTESIAN_POINT ( 'NONE',  ( -65.67956025985559165, -296.5929058063541106, -202.7505288912029755 ) ) ;
#91677 = ORIENTED_EDGE ( 'NONE', *, *, #61610, .F. ) ;
#91678 = CARTESIAN_POINT ( 'NONE',  ( -96.93311372400863490, -287.0863581395156530, -225.7497110762313639 ) ) ;
#91679 =( BOUNDED_CURVE ( )  B_SPLINE_CURVE ( 3, ( #88256, #59402, #45156, #7793 ),
 .UNSPECIFIED., .F., .F. ) 
 B_SPLINE_CURVE_WITH_KNOTS ( ( 4, 4 ),
 ( 3.665191429188167760, 4.712388980384689674 ),
 .UNSPECIFIED. ) 
 CURVE ( )  GEOMETRIC_REPRESENTATION_ITEM ( )  RATIONAL_B_SPLINE_CURVE ( ( 1.000000000000000000, 0.9106836025229716469, 0.9106836025229716469, 1.000000000000000000 ) ) 
 REPRESENTATION_ITEM ( '' )  );
#91680 = CARTESIAN_POINT ( 'NONE',  ( -37.80700652970080711, -293.1261177018325839, -193.6716402084201718 ) ) ;
#91681 = CARTESIAN_POINT ( 'NONE',  ( -69.04587751631092374, -284.1319044414154860, -336.2440352460590702 ) ) ;
#91682 = CARTESIAN_POINT ( 'NONE',  ( 9.376661853561191862, -273.7355459901817767, -209.4495848706881134 ) ) ;
#91683 = CARTESIAN_POINT ( 'NONE',  ( -104.5249557294449971, -291.6892164454312137, -232.9482464927356489 ) ) ;
#91684 = CARTESIAN_POINT ( 'NONE',  ( -106.7843600063659864, -283.0858162600539458, -239.9311469303197271 ) ) ;
#91685 = CARTESIAN_POINT ( 'NONE',  ( -30.70332401068005623, -292.4670464085056665, -193.6162868816578850 ) ) ;
#91686 = CARTESIAN_POINT ( 'NONE',  ( 31.85927862664286181, -287.5758766648709752, -247.0520633868182756 ) ) ;
#91687 = CARTESIAN_POINT ( 'NONE',  ( 197.6805213618982009, 68.84011358609819808, 9.477520602874013989 ) ) ;
#91688 = CARTESIAN_POINT ( 'NONE',  ( -97.78953360390984528, -246.5544654070388901, -331.3250685880491915 ) ) ;
#91689 = CARTESIAN_POINT ( 'NONE',  ( 11.06782603903197781, -283.9164310913357667, -329.4144678386594478 ) ) ;
#91690 = CARTESIAN_POINT ( 'NONE',  ( 31.98288692825983404, -284.6237833571634042, -237.0123917617631264 ) ) ;
#91691 = ORIENTED_EDGE ( 'NONE', *, *, #47636, .F. ) ;
#91692 = CARTESIAN_POINT ( 'NONE',  ( 29.25923994371089876, -280.0594779340414107, -239.6037990337738108 ) ) ;
#91693 = CARTESIAN_POINT ( 'NONE',  ( -42.80890441612591957, -276.7860923562897710, -347.1455823539620837 ) ) ;
#91694 = CARTESIAN_POINT ( 'NONE',  ( -32.87849668878786247, -282.1086894124832725, -195.6609958751906220 ) ) ;
#91695 = CARTESIAN_POINT ( 'NONE',  ( 66.77714209949721180, 46.10201122810671137, -317.1972835727068514 ) ) ;
#91696 = CARTESIAN_POINT ( 'NONE',  ( 33.78266960039268696, -279.7684819353552825, -242.2893835750898006 ) ) ;
#91697 = CARTESIAN_POINT ( 'NONE',  ( -104.9651022474555049, -282.9910903011765413, -238.6329437063494936 ) ) ;
#91698 = CARTESIAN_POINT ( 'NONE',  ( -59.86933866991501674, -299.5244753058009337, -197.7358065938024936 ) ) ;
#91699 = CARTESIAN_POINT ( 'NONE',  ( 21.03919886363193115, -293.4281445012146037, -226.4332330488559535 ) ) ;
#91700 = ORIENTED_EDGE ( 'NONE', *, *, #61930, .F. ) ;
#91701 = CARTESIAN_POINT ( 'NONE',  ( -110.8303546302146430, -289.2263167016748753, -271.1742207043170083 ) ) ;
#91702 = CARTESIAN_POINT ( 'NONE',  ( 39.52192656842822771, -276.2495196040169958, -274.0308160220959621 ) ) ;
#91703 = CARTESIAN_POINT ( 'NONE',  ( -35.81771388425057268, -298.2384338344615458, -197.3610733349210307 ) ) ;
#91704 = ORIENTED_EDGE ( 'NONE', *, *, #43329, .F. ) ;
#91705 = CARTESIAN_POINT ( 'NONE',  ( -7.796899972571944559, -273.3505533472036291, -199.5332986406163229 ) ) ;
#91706 = CARTESIAN_POINT ( 'NONE',  ( 144.2857639756989272, -299.5541904835127980, -201.0153591320744226 ) ) ;
#91707 = LINE ( 'NONE', #20696, #74849 ) ;
#91708 = CARTESIAN_POINT ( 'NONE',  ( 154.8793480878393041, 20.01712742760162200, 11.60576973085460040 ) ) ;
#91709 = CARTESIAN_POINT ( 'NONE',  ( 16.06043083789317194, -283.3524651980815179, -320.6582549383179526 ) ) ;
#91710 = CARTESIAN_POINT ( 'NONE',  ( 23.45795931788408950, -283.9269596676531933, -315.9393521227596580 ) ) ;
#91711 = CARTESIAN_POINT ( 'NONE',  ( -101.9845361584891776, -283.1420753304184927, -304.8887313686983020 ) ) ;
#91712 = CARTESIAN_POINT ( 'NONE',  ( 23.72564104763106130, -273.3817406380417196, -228.8990854082144892 ) ) ;
#91713 = CARTESIAN_POINT ( 'NONE',  ( 36.75126273659486742, -283.3529897628757794, -265.7678259215918501 ) ) ;
#91714 = CARTESIAN_POINT ( 'NONE',  ( 34.83980279765318500, -274.2260877448811129, -285.2116529775123581 ) ) ;
#91715 = LINE ( 'NONE', #41519, #10997 ) ;
#91716 = CARTESIAN_POINT ( 'NONE',  ( 35.41461877289251703, -276.7551922408595715, -279.7523525690032784 ) ) ;
#91717 = CARTESIAN_POINT ( 'NONE',  ( 195.3024354219830911, 42.05395879699454298, 13.15751923266871870 ) ) ;
#91718 = CARTESIAN_POINT ( 'NONE',  ( -112.6333464956169905, -279.1619107544272538, -285.7664656497231022 ) ) ;
#91719 = ORIENTED_EDGE ( 'NONE', *, *, #55843, .T. ) ;
#91720 = EDGE_LOOP ( 'NONE', ( #47417, #4672, #92622, #3973 ) ) ;
#91721 = CARTESIAN_POINT ( 'NONE',  ( -48.18343439339133027, -283.5835610574164889, -435.6442049081568939 ) ) ;
#91722 = CARTESIAN_POINT ( 'NONE',  ( -111.3138993237154040, -286.2043231567379848, -286.7446228228934046 ) ) ;
#91723 = EDGE_CURVE ( 'NONE', #69962, #25512, #14629, .T. ) ;
#91724 = CARTESIAN_POINT ( 'NONE',  ( -6.706584450672058217, -293.8365004650218566, -336.7997469187502588 ) ) ;
#91725 = CARTESIAN_POINT ( 'NONE',  ( -3.113565606788212481, -287.9605343500850836, -339.2360750304758881 ) ) ;
#91726 = CARTESIAN_POINT ( 'NONE',  ( -44.09482455433020220, -284.2054497223587646, -196.6565094170741190 ) ) ;
#91728 = CARTESIAN_POINT ( 'NONE',  ( -64.20936656575456425, -287.6472766143098738, -339.3805644166588991 ) ) ;
#91727 = CARTESIAN_POINT ( 'NONE',  ( -109.0032193232709687, -282.9072508542182049, -287.1494823584988580 ) ) ;
#91729 = CARTESIAN_POINT ( 'NONE',  ( -108.1401275136907998, -285.5023079593642592, -289.7660414748662561 ) ) ;
#91730 = CARTESIAN_POINT ( 'NONE',  ( 13.50798406253006334, -274.3405802992307940, -325.5617193760199939 ) ) ;
#91731 = CARTESIAN_POINT ( 'NONE',  ( 4.754873096778361230, -285.0098494613138200, -206.7819721037364502 ) ) ;
#91732 = CARTESIAN_POINT ( 'NONE',  ( -110.6511567924562485, -298.7563420412542996, -254.4668045767008948 ) ) ;
#91733 = CARTESIAN_POINT ( 'NONE',  ( -111.6705326620546970, -282.6997599140643160, -258.8270086063118356 ) ) ;
#91734 = CARTESIAN_POINT ( 'NONE',  ( 29.18140896738806589, -282.0800761637487426, -239.6114658502153532 ) ) ;
#91735 = CARTESIAN_POINT ( 'NONE',  ( -8.902587315481309105, -290.6812121743489001, -339.9541046579662975 ) ) ;
#91736 = CARTESIAN_POINT ( 'NONE',  ( 222.4306832106270804, -141.7221692137691775, -21.50000000000000000 ) ) ;
#91737 = EDGE_CURVE ( 'NONE', #28617, #32853, #87125, .T. ) ;
#91738 = DIRECTION ( 'NONE',  ( 0.000000000000000000, 0.000000000000000000, 1.000000000000000000 ) ) ;
#91739 = CARTESIAN_POINT ( 'NONE',  ( -96.26876338466560412, -297.8262628224761102, -317.6776274099951252 ) ) ;
#91740 = CARTESIAN_POINT ( 'NONE',  ( -35.59126679820413131, -278.0739276898694925, -195.3688009783398059 ) ) ;
#91741 = CARTESIAN_POINT ( 'NONE',  ( 22.98766303208299533, -292.1113056397780383, -222.7530447998403815 ) ) ;
#91742 = CARTESIAN_POINT ( 'NONE',  ( -105.7106075919401889, -294.5838432640967994, -298.1483975485358542 ) ) ;
#91743 = CARTESIAN_POINT ( 'NONE',  ( -77.07448203530071851, -278.1926744803297424, -208.4736902566769174 ) ) ;
#91744 = CARTESIAN_POINT ( 'NONE',  ( -43.57887120726325492, -272.0527257780428840, -196.1311633506247745 ) ) ;
#91745 = CARTESIAN_POINT ( 'NONE',  ( 35.19800885243055433, -294.7116871009865804, -258.4827826992625432 ) ) ;
#91746 = CARTESIAN_POINT ( 'NONE',  ( 35.78497577281001440, -296.2662352645559167, -287.0191576251351080 ) ) ;
#91747 = CARTESIAN_POINT ( 'NONE',  ( -113.4278473810832253, -295.1134496897300323, -263.9096316018108155 ) ) ;
#91748 = CARTESIAN_POINT ( 'NONE',  ( -71.69384214182173309, -289.8444593454817664, -202.5683653275041252 ) ) ;
#91749 = CARTESIAN_POINT ( 'NONE',  ( -93.01406652992514523, -292.6576305823376742, -222.2366695440773583 ) ) ;
#91750 = CARTESIAN_POINT ( 'NONE',  ( 180.6899167944524436, -12.49482340714361506, 10.00000000000000000 ) ) ;
#91751 = CARTESIAN_POINT ( 'NONE',  ( -109.4376628559425342, -291.5225509525306506, -257.6308211104511656 ) ) ;
#91752 = CYLINDRICAL_SURFACE ( 'NONE', #3654, 20.00000000000000355 ) ;
#91753 = CARTESIAN_POINT ( 'NONE',  ( -112.9655983075335399, -291.6037549177669348, -282.5690966434786446 ) ) ;
#91755 = CARTESIAN_POINT ( 'NONE',  ( 33.30820374967189679, -293.3095799440126825, -251.9874661391123709 ) ) ;
#91754 = CARTESIAN_POINT ( 'NONE',  ( 34.61279915932067297, -279.2849566659546099, -247.9790529440880391 ) ) ;
#91756 = CARTESIAN_POINT ( 'NONE',  ( -36.75255387050101774, -280.0593655540109808, -193.3503263514216144 ) ) ;
#91757 = CARTESIAN_POINT ( 'NONE',  ( -113.7981455125467534, -284.3308724264385319, -261.4081156560843056 ) ) ;
#91758 = CARTESIAN_POINT ( 'NONE',  ( 17.33345799608588322, -286.2696054494083455, -321.5314842045175396 ) ) ;
#91759 = CARTESIAN_POINT ( 'NONE',  ( -101.4800478459414848, -282.1872960009666826, -307.7394249323233453 ) ) ;
#91760 = CARTESIAN_POINT ( 'NONE',  ( 0.000000000000000000, 0.000000000000000000, -12.50000000000000000 ) ) ;
#91761 = CARTESIAN_POINT ( 'NONE',  ( -72.17290680989286500, -278.0798378535758388, -202.4533397644107424 ) ) ;
#91762 = CARTESIAN_POINT ( 'NONE',  ( -18.24564896744194797, -285.2128513128089935, -196.0308457512828397 ) ) ;
#91763 = CARTESIAN_POINT ( 'NONE',  ( 195.2279938257249228, 39.55206589069444334, 15.00421968542118911 ) ) ;
#91764 = CARTESIAN_POINT ( 'NONE',  ( -0.8789515018298554860, -294.1449983330211921, -206.1833473218507891 ) ) ;
#91765 = CARTESIAN_POINT ( 'NONE',  ( 30.71718065816105181, -276.5265891308233677, -235.6250410964830451 ) ) ;
#91766 = CARTESIAN_POINT ( 'NONE',  ( -36.47017944079517093, -276.7076860550151309, -343.3895319701514950 ) ) ;
#91767 = CARTESIAN_POINT ( 'NONE',  ( -113.3597151247126931, -290.5655268720333879, -282.6192336813119255 ) ) ;
#91768 = CARTESIAN_POINT ( 'NONE',  ( 1.335637636764364089, -280.6195446509958060, -335.2716544245148498 ) ) ;
#91769 = CARTESIAN_POINT ( 'NONE',  ( 28.95660921510317820, -292.1905694134405849, -239.1296145586582043 ) ) ;
#91770 = CARTESIAN_POINT ( 'NONE',  ( -102.8682676129395190, -294.0651481178776407, -306.9539161013492503 ) ) ;
#91771 = EDGE_LOOP ( 'NONE', ( #90624, #35614, #26205, #91094, #83276, #26379 ) ) ;
#91772 = CARTESIAN_POINT ( 'NONE',  ( 152.4883615486727990, 19.90193753872963711, 8.271207965229679715 ) ) ;
#91773 = CARTESIAN_POINT ( 'NONE',  ( -17.40979028262555062, -291.8239024861443340, -200.0183139752226396 ) ) ;
#91774 = CARTESIAN_POINT ( 'NONE',  ( 123.4306832106270804, -181.2434395487259167, 0.000000000000000000 ) ) ;
#91775 = CARTESIAN_POINT ( 'NONE',  ( -92.08974858914540107, -281.4094976428775112, -313.9805196606274080 ) ) ;
#91776 = CARTESIAN_POINT ( 'NONE',  ( -113.3670549132092873, -295.7454264841297800, -259.6376067691606409 ) ) ;
#91777 = CARTESIAN_POINT ( 'NONE',  ( 19.22256250171952985, -278.9970818841499636, -219.9353566953350310 ) ) ;
#91778 = CARTESIAN_POINT ( 'NONE',  ( -65.71016979450726581, -287.0039650047797863, -199.2940568747584678 ) ) ;
#91779 = CARTESIAN_POINT ( 'NONE',  ( -39.97179267375241807, -285.8515069821102657, -197.4085126985433760 ) ) ;
#91780 = CARTESIAN_POINT ( 'NONE',  ( -71.96295337408257353, -279.0387012991084816, -335.4297623780029198 ) ) ;
#91781 = CARTESIAN_POINT ( 'NONE',  ( -109.4174155893551585, -294.8236238401540845, -250.8970348886875854 ) ) ;
#91782 = CARTESIAN_POINT ( 'NONE',  ( -105.8921281902340326, -297.9435718458106521, -298.2683361158940443 ) ) ;
#91783 = CARTESIAN_POINT ( 'NONE',  ( -110.6775056113343396, -277.3077303702995664, -273.3594738413528376 ) ) ;
#91784 = ORIENTED_EDGE ( 'NONE', *, *, #54006, .T. ) ;
#91785 = CYLINDRICAL_SURFACE ( 'NONE', #35007, 7.500000000000012434 ) ;
#91786 = CARTESIAN_POINT ( 'NONE',  ( -111.1963033213652068, -295.9459741385330176, -292.1157270547931262 ) ) ;
#91787 = CARTESIAN_POINT ( 'NONE',  ( -107.9446695683545840, -292.7795539742988353, -246.7701259812290004 ) ) ;
#91788 = CARTESIAN_POINT ( 'NONE',  ( 200.9739487937824833, 293.7020456634571701, -53.99999999999736389 ) ) ;
#91789 = CARTESIAN_POINT ( 'NONE',  ( -29.15347963775107232, -289.5970591747833964, -343.0030185172483357 ) ) ;
#91790 = CARTESIAN_POINT ( 'NONE',  ( -43.47533972853607054, -255.2787295525174613, -444.3320233189222677 ) ) ;
#91791 = ORIENTED_EDGE ( 'NONE', *, *, #22448, .T. ) ;
#91792 = CARTESIAN_POINT ( 'NONE',  ( -1.235477515598032872, -279.5780311815800587, -202.6177721682351205 ) ) ;
#91793 = CARTESIAN_POINT ( 'NONE',  ( -112.1770765771534997, -297.4251209566139664, -252.6698992889003819 ) ) ;
#91794 = CARTESIAN_POINT ( 'NONE',  ( -110.7315722883733571, -288.4517730928777155, -289.2341395093843062 ) ) ;
#91795 = CARTESIAN_POINT ( 'NONE',  ( -109.8323779623486729, -297.2124640399762825, -244.4604245824954205 ) ) ;
#91796 = CARTESIAN_POINT ( 'NONE',  ( 35.66326375148873495, -293.9266412847684364, -273.4856438674964920 ) ) ;
#91797 = LINE ( 'NONE', #19371, #77551 ) ;
#91798 = CARTESIAN_POINT ( 'NONE',  ( 196.1155190967640465, 73.07272925554217124, -11.82469951281970566 ) ) ;
#91799 = CARTESIAN_POINT ( 'NONE',  ( 195.0811277904324754, 250.0000000000000568, 15.19607843137254477 ) ) ;
#91800 = CARTESIAN_POINT ( 'NONE',  ( 22.75351225982018732, -289.7066959741308665, -317.4063404058811102 ) ) ;
#91801 = CARTESIAN_POINT ( 'NONE',  ( -72.02372285203398405, -279.9805209788415823, -342.4524372437778652 ) ) ;
#91802 = CARTESIAN_POINT ( 'NONE',  ( 37.76417643443183891, -281.1081970956980172, -286.9270524464232608 ) ) ;
#91803 = CARTESIAN_POINT ( 'NONE',  ( -109.1205617816469129, -286.8275520536594740, -249.0193444161533591 ) ) ;
#91804 = CARTESIAN_POINT ( 'NONE',  ( -5.006668005434542046, -285.0443140911882551, -201.1292467610936967 ) ) ;
#91805 = CARTESIAN_POINT ( 'NONE',  ( -92.45595725158084122, -271.2609296138390960, -219.7215374228372013 ) ) ;
#91806 = CARTESIAN_POINT ( 'NONE',  ( -43.62762957097055505, -275.8924144356403190, -196.1352781762911945 ) ) ;
#91807 = CARTESIAN_POINT ( 'NONE',  ( -109.4983884083058854, -288.8694035462945635, -252.0138120648957454 ) ) ;
#91808 = CARTESIAN_POINT ( 'NONE',  ( -88.36255563599863194, -279.6185667387573517, -326.3716329020712692 ) ) ;
#91809 = ORIENTED_EDGE ( 'NONE', *, *, #77701, .T. ) ;
#91811 = CARTESIAN_POINT ( 'NONE',  ( -27.53650123667327776, -279.5284492524394295, -197.8684942311847124 ) ) ;
#91810 = CARTESIAN_POINT ( 'NONE',  ( -76.82185668607338869, -279.5076366028725943, -208.8979501364676707 ) ) ;
#91812 = CARTESIAN_POINT ( 'NONE',  ( 37.29423665495373541, -276.8539013933267370, -288.0520528909956397 ) ) ;
#91813 = CARTESIAN_POINT ( 'NONE',  ( -74.80030153582180219, -278.3597924952936182, -203.5414958685116460 ) ) ;
#91814 = CARTESIAN_POINT ( 'NONE',  ( 4.282212335244459211, -58.25047808272906025, -351.9149493628895584 ) ) ;
#91815 = CARTESIAN_POINT ( 'NONE',  ( -18.61899987255275946, -275.2287030145972722, -195.8597626330902983 ) ) ;
#91816 = CARTESIAN_POINT ( 'NONE',  ( -51.70776717304013914, -299.2972395592836961, -195.2590580967229812 ) ) ;
#91817 = CARTESIAN_POINT ( 'NONE',  ( 10.59707575819634329, -289.1948066931273615, -210.1954327657594490 ) ) ;
#91818 = DIRECTION ( 'NONE',  ( 0.000000000000000000, -1.000000000000000000, 0.000000000000000000 ) ) ;
#91819 = CARTESIAN_POINT ( 'NONE',  ( 35.30053514148841032, -288.4973683995830811, -260.1251577783254447 ) ) ;
#91820 = CARTESIAN_POINT ( 'NONE',  ( 19.82553354330629602, -289.9987018940424832, -320.4395068173125765 ) ) ;
#91821 = CARTESIAN_POINT ( 'NONE',  ( -105.8031890486252991, -290.2439073460990926, -244.5871305292801026 ) ) ;
#91822 = CARTESIAN_POINT ( 'NONE',  ( -90.40024388924976506, -283.2865065463062706, -326.1505799899610452 ) ) ;
#91823 = CARTESIAN_POINT ( 'NONE',  ( 20.31364087874701951, -279.3082717431319679, -224.2926681367810602 ) ) ;
#91824 = CARTESIAN_POINT ( 'NONE',  ( -80.03876101613434457, -287.3283573091060816, -209.5705195250062616 ) ) ;
#91825 = CARTESIAN_POINT ( 'NONE',  ( 32.88619890473360385, -280.3273064246847639, -292.8598822282093579 ) ) ;
#91826 = CARTESIAN_POINT ( 'NONE',  ( -57.26286389490530837, -281.1048254673006568, -199.6193996619407756 ) ) ;
#91827 = CARTESIAN_POINT ( 'NONE',  ( -53.96184027778807035, -277.7635378514856939, -341.5593444223308097 ) ) ;
#91828 = CARTESIAN_POINT ( 'NONE',  ( -112.9704871889050963, -289.1939925663604072, -282.5387731981658703 ) ) ;
#91829 = CARTESIAN_POINT ( 'NONE',  ( -97.04045901947404218, -284.7045630008437911, -318.7575810530527747 ) ) ;
#91830 = CARTESIAN_POINT ( 'NONE',  ( -55.68143276528162744, -283.7744671459013830, -345.0818052776580771 ) ) ;
#91831 = CARTESIAN_POINT ( 'NONE',  ( 31.97593600518977652, -281.4130346249777404, -247.3093392063195211 ) ) ;
#91832 = ORIENTED_EDGE ( 'NONE', *, *, #89671, .F. ) ;
#91833 = CYLINDRICAL_SURFACE ( 'NONE', #79150, 25.00000000000000000 ) ;
#91834 = CARTESIAN_POINT ( 'NONE',  ( -71.63472046504641355, -293.4644308327153226, -202.7871904682546358 ) ) ;
#91835 = CARTESIAN_POINT ( 'NONE',  ( -64.19989079931440301, -290.3939113357287169, -198.6677790883814509 ) ) ;
#91836 = CARTESIAN_POINT ( 'NONE',  ( 35.07612058973654001, -274.4663030009210161, -259.3648356892419997 ) ) ;
#91837 = ADVANCED_FACE ( 'NONE', ( #15534 ), #29758, .F. ) ;
#91838 = CARTESIAN_POINT ( 'NONE',  ( -105.8706357552103299, -295.4495753946923173, -305.3653693011394239 ) ) ;
#91839 = CARTESIAN_POINT ( 'NONE',  ( -19.88936985730601137, -290.7603060234929444, -198.7113942926003460 ) ) ;
#91840 = CARTESIAN_POINT ( 'NONE',  ( 23.75700681572322637, -292.3663860301136310, -312.2229679927377219 ) ) ;
#91841 = CARTESIAN_POINT ( 'NONE',  ( -73.72855007748313483, -290.7517836848141997, -334.1182738369247431 ) ) ;
#91842 = CARTESIAN_POINT ( 'NONE',  ( 133.0380396672494783, -299.5541904835127980, -189.2093064027359901 ) ) ;
#91843 = CARTESIAN_POINT ( 'NONE',  ( -110.3756761777892734, -292.7713613656292750, -253.3012529244568327 ) ) ;
#91844 = CARTESIAN_POINT ( 'NONE',  ( 37.40593867008024631, -291.4443189539040304, -261.9568209886302270 ) ) ;
#91845 = CARTESIAN_POINT ( 'NONE',  ( 21.89687321264483089, -296.1831772298917826, -316.3793056893565563 ) ) ;
#91846 = CARTESIAN_POINT ( 'NONE',  ( -52.14817795662543887, -286.7991715726088842, -198.6382021069378254 ) ) ;
#91847 = CARTESIAN_POINT ( 'NONE',  ( 25.00566051432071291, -296.1189489545133711, -312.3472472124772139 ) ) ;
#91848 = EDGE_CURVE ( 'NONE', #5104, #45831, #36385, .T. ) ;
#91849 = CARTESIAN_POINT ( 'NONE',  ( 38.06180751901270298, -277.5418625123454035, -271.1291655900909632 ) ) ;
#91850 = CARTESIAN_POINT ( 'NONE',  ( -112.9665071198076021, -272.0788151381000830, -256.1413742479614939 ) ) ;
#91851 = CARTESIAN_POINT ( 'NONE',  ( 36.36107723001683922, -273.8801293882200412, -277.1341986536174886 ) ) ;
#91852 = CARTESIAN_POINT ( 'NONE',  ( 8.039176767074440733, -278.7573703702663011, -211.2883394012095266 ) ) ;
#91853 = CARTESIAN_POINT ( 'NONE',  ( -74.48751654362214936, -274.7516660076539665, -206.9988494864960558 ) ) ;
#91854 = ADVANCED_FACE ( 'NONE', ( #28828 ), #50601, .T. ) ;
#91855 = CARTESIAN_POINT ( 'NONE',  ( -100.6643184575767265, -297.4651814447006473, -307.9530244787657125 ) ) ;
#91856 = FACE_OUTER_BOUND ( 'NONE', #49313, .T. ) ;
#91857 = CARTESIAN_POINT ( 'NONE',  ( -100.3002295447359273, -296.8428419755931600, -307.7277943024036517 ) ) ;
#91858 = DIRECTION ( 'NONE',  ( 0.000000000000000000, 0.000000000000000000, 1.000000000000000000 ) ) ;
#91860 = CARTESIAN_POINT ( 'NONE',  ( -69.48904837939930701, -273.4501191088235146, -204.8206876746464218 ) ) ;
#91859 = CARTESIAN_POINT ( 'NONE',  ( 37.93604199813501054, -285.5157656970316680, -265.9405660656128703 ) ) ;
#91861 = CARTESIAN_POINT ( 'NONE',  ( 1.521678898389058121, -286.5565626252717948, -203.8729447923337545 ) ) ;
#91862 = CARTESIAN_POINT ( 'NONE',  ( -68.04934297520905773, -289.1111759990607766, -340.9499624437111720 ) ) ;
#91863 = CARTESIAN_POINT ( 'NONE',  ( -109.9992654286719613, -298.2762687694247461, -290.3432352252511350 ) ) ;
#91864 = CARTESIAN_POINT ( 'NONE',  ( -58.96164863047513194, -293.3323655883094148, -342.0033279630837342 ) ) ;
#91865 = CARTESIAN_POINT ( 'NONE',  ( 37.17715946099330893, -280.5143881901126974, -251.6234984260304941 ) ) ;
#91866 = CARTESIAN_POINT ( 'NONE',  ( -95.99890600148557951, -293.4094976428775681, -317.0979686699210447 ) ) ;
#91867 = CARTESIAN_POINT ( 'NONE',  ( -101.8277212569831391, -277.0654772562059520, -231.9657784740427360 ) ) ;
#91868 = CARTESIAN_POINT ( 'NONE',  ( -95.27339438497588731, -288.7153551414180015, -315.4485938646981822 ) ) ;
#91869 = DIRECTION ( 'NONE',  ( -0.000000000000000000, 1.000000000000000000, 0.000000000000000000 ) ) ;
#91870 = CARTESIAN_POINT ( 'NONE',  ( -93.93726597655496846, -287.8683913119828048, -319.6519974895999212 ) ) ;
#91871 = CARTESIAN_POINT ( 'NONE',  ( -33.78388818234863322, -299.6975443180613183, -196.5601236198808408 ) ) ;
#91872 = CARTESIAN_POINT ( 'NONE',  ( 35.60773147979883646, -282.6895716546461017, -247.6237759881351792 ) ) ;
#91874 = CARTESIAN_POINT ( 'NONE',  ( 35.68737416741759461, -281.5287034445308905, -268.5835766000296871 ) ) ;
#91873 = CARTESIAN_POINT ( 'NONE',  ( -106.7449695285716018, -271.0213444609829025, -240.3541517011892665 ) ) ;
#91875 = CARTESIAN_POINT ( 'NONE',  ( -95.57249168267412642, -297.4000665056227035, -219.9012354232556277 ) ) ;
#91876 = CARTESIAN_POINT ( 'NONE',  ( -90.63575263835306828, -274.7035018539475004, -219.5970478485548369 ) ) ;
#91877 = CARTESIAN_POINT ( 'NONE',  ( 37.91106703316073379, -285.7187508110668546, -277.1681166480832417 ) ) ;
#91878 = CARTESIAN_POINT ( 'NONE',  ( -39.55445629143974884, -282.0245547042659382, -195.3810513015654067 ) ) ;
#91879 = CARTESIAN_POINT ( 'NONE',  ( -63.40381652690489744, -272.6247474751405662, -201.8275555931272152 ) ) ;
#91880 = ORIENTED_EDGE ( 'NONE', *, *, #66944, .T. ) ;
#91881 = CARTESIAN_POINT ( 'NONE',  ( 186.6539576904058890, 293.9636489450775230, 11.60392986742922439 ) ) ;
#91882 = CARTESIAN_POINT ( 'NONE',  ( -77.96487866844292114, -287.4836577092515881, -207.6770657199440393 ) ) ;
#91883 = DIRECTION ( 'NONE',  ( 0.000000000000000000, 0.000000000000000000, 1.000000000000000000 ) ) ;
#91884 = CARTESIAN_POINT ( 'NONE',  ( 13.84574458161073807, -272.1952119285918457, -206.2264541496106460 ) ) ;
#91885 = CARTESIAN_POINT ( 'NONE',  ( 21.60017092007287687, -275.4141205316000764, -319.6562968383907446 ) ) ;
#91886 = CARTESIAN_POINT ( 'NONE',  ( -91.23543323702172358, -285.3562470314963093, -320.6221693475289953 ) ) ;
#91887 = CARTESIAN_POINT ( 'NONE',  ( 21.30499631019853268, -276.5288173438711397, -225.5407098235782826 ) ) ;
#91888 = CARTESIAN_POINT ( 'NONE',  ( -110.5382745982274173, -285.6995892137407509, -292.3352137674459073 ) ) ;
#91889 = CARTESIAN_POINT ( 'NONE',  ( -56.43690790025585358, -282.0987019870414656, -341.2307415448175902 ) ) ;
#91890 = CARTESIAN_POINT ( 'NONE',  ( 34.64734469879528689, -283.2814240066580851, -249.3235783220800386 ) ) ;
#91891 = CARTESIAN_POINT ( 'NONE',  ( -41.19489415316546399, -274.1717271464443115, -193.4053284942501136 ) ) ;
#91892 = CARTESIAN_POINT ( 'NONE',  ( 38.92446846478642897, -275.2528393179302952, -259.7558583125066889 ) ) ;
#91893 = CARTESIAN_POINT ( 'NONE',  ( -45.21928212433525118, -297.0727189644497912, -344.4345994803593953 ) ) ;
#91894 = DIRECTION ( 'NONE',  ( 0.000000000000000000, 0.000000000000000000, 1.000000000000000000 ) ) ;
#91895 = CARTESIAN_POINT ( 'NONE',  ( 165.2494399300530290, 8.542400036368780647, 9.000000000000001776 ) ) ;
#91896 = CARTESIAN_POINT ( 'NONE',  ( -78.82085296595143120, -293.7443424706657993, -333.7628952348099460 ) ) ;
#91897 = CIRCLE ( 'NONE', #73809, 4.000000000000003553 ) ;
#91898 = CARTESIAN_POINT ( 'NONE',  ( -11.23790622253789984, -276.2102227427271828, -338.6002591364451746 ) ) ;
#91899 = CARTESIAN_POINT ( 'NONE',  ( -113.9446275073758699, -273.7570339554058592, -270.3764274833388868 ) ) ;
#91900 = CARTESIAN_POINT ( 'NONE',  ( -74.07780344596864097, -287.3170995385450510, -206.0935373704038795 ) ) ;
#91901 = CARTESIAN_POINT ( 'NONE',  ( 15.01713785587491401, -295.8495755538914409, -325.8702148620531034 ) ) ;
#91902 = CARTESIAN_POINT ( 'NONE',  ( 15.21745189415454114, -295.5345800671756251, -326.0885282622135151 ) ) ;
#91903 = CARTESIAN_POINT ( 'NONE',  ( -73.53544701219848889, -293.5712964389833246, -204.8044734432176313 ) ) ;
#91904 = CARTESIAN_POINT ( 'NONE',  ( -43.88667278441708675, -277.9692035606976788, -195.7630480247708249 ) ) ;
#91905 = CARTESIAN_POINT ( 'NONE',  ( -67.91972832504953317, -281.5677790049043665, -202.4775244486798158 ) ) ;
#91906 = CARTESIAN_POINT ( 'NONE',  ( -110.0026929880996249, -294.4227261725366702, -286.5380867493872756 ) ) ;
#91907 = CARTESIAN_POINT ( 'NONE',  ( -4.674599227087804287, -284.4868630699195364, -338.7359360913204682 ) ) ;
#91908 = CARTESIAN_POINT ( 'NONE',  ( -52.13794709388877635, -284.7785734099470005, -198.5607200144326612 ) ) ;
#91909 = CARTESIAN_POINT ( 'NONE',  ( 201.4154447744461436, 287.2677491621798254, -97.13488168232527187 ) ) ;
#91910 = ORIENTED_EDGE ( 'NONE', *, *, #28072, .F. ) ;
#91911 = CARTESIAN_POINT ( 'NONE',  ( -54.75726958385478582, -285.4889231387453492, -199.3948759657450864 ) ) ;
#91912 = ORIENTED_EDGE ( 'NONE', *, *, #38745, .F. ) ;
#91913 = CARTESIAN_POINT ( 'NONE',  ( 38.12387407597498168, -282.8041900982574930, -284.0884207088452627 ) ) ;
#91914 = CARTESIAN_POINT ( 'NONE',  ( -62.04083777113134346, -274.0552430078333828, -201.6440161341498083 ) ) ;
#91915 = CARTESIAN_POINT ( 'NONE',  ( 35.47640323013938257, -286.0444184606371891, -246.4104449699778172 ) ) ;
#91916 = CARTESIAN_POINT ( 'NONE',  ( -111.2108243040277102, -279.2308470294760241, -291.2458661682531442 ) ) ;
#91917 = CARTESIAN_POINT ( 'NONE',  ( -109.0782685117798820, -279.7389951790068494, -296.5265881705340121 ) ) ;
#91918 = CARTESIAN_POINT ( 'NONE',  ( 19.07972590216577657, -281.4908782539976642, -218.1123335820869045 ) ) ;
#91919 = CARTESIAN_POINT ( 'NONE',  ( -102.0172624299487154, -276.4809262143062369, -239.1787733560258289 ) ) ;
#91920 = CARTESIAN_POINT ( 'NONE',  ( 168.9861705969244952, 232.0887483361810553, -192.7465431548272932 ) ) ;
#91921 = ORIENTED_EDGE ( 'NONE', *, *, #59069, .T. ) ;
#91922 = CARTESIAN_POINT ( 'NONE',  ( 8.432731809881056861, -276.6807212603808352, -211.1603595064202068 ) ) ;
#91923 = CARTESIAN_POINT ( 'NONE',  ( 160.6459981038951241, 220.5539213599568882, -205.1006532850495319 ) ) ;
#91924 = CARTESIAN_POINT ( 'NONE',  ( -110.2069566012316244, -276.7819686512834210, -254.1008076556053368 ) ) ;
#91925 = CARTESIAN_POINT ( 'NONE',  ( 33.50974497670642194, -294.9581110484263036, -242.7559094410300702 ) ) ;
#91926 = CARTESIAN_POINT ( 'NONE',  ( -12.98208472004965763, -294.0757943326610757, -339.3383318844054202 ) ) ;
#91927 = CARTESIAN_POINT ( 'NONE',  ( -60.01512694401825598, -288.8459964239874012, -343.8828332748200864 ) ) ;
#91928 = CARTESIAN_POINT ( 'NONE',  ( 10.19742947581766401, -229.5268262511776527, 25.50000000000000000 ) ) ;
#91930 = CARTESIAN_POINT ( 'NONE',  ( -42.71223244418801812, -284.3831666969355751, -196.7440212856437540 ) ) ;
#91929 = CARTESIAN_POINT ( 'NONE',  ( -70.56818840286992156, -294.0563422331115930, -339.1839972827448833 ) ) ;
#91931 = CARTESIAN_POINT ( 'NONE',  ( -67.08028788448426383, -293.5185224848062830, -202.3428713081064245 ) ) ;
#91932 = CARTESIAN_POINT ( 'NONE',  ( 11.60892536227643923, -285.2256131238391959, -215.2058446102657285 ) ) ;
#91933 = CARTESIAN_POINT ( 'NONE',  ( -93.64361965568940604, -286.5336010592957905, -223.1240844515426147 ) ) ;
#91934 = ORIENTED_EDGE ( 'NONE', *, *, #74810, .F. ) ;
#91935 = CARTESIAN_POINT ( 'NONE',  ( -99.02270762608848997, -292.1029866440836145, -224.6414619417408005 ) ) ;
#91936 = CARTESIAN_POINT ( 'NONE',  ( 34.29225727024859083, -282.2347667020269455, -284.7964595700007635 ) ) ;
#91937 = CARTESIAN_POINT ( 'NONE',  ( -111.2131959168634694, -295.0918155158527725, -290.6345199974070965 ) ) ;
#91938 = CARTESIAN_POINT ( 'NONE',  ( -113.9506063685677333, -291.2724074518176849, -276.9499439747928591 ) ) ;
#91939 = CARTESIAN_POINT ( 'NONE',  ( -112.2013555857373746, -290.8214502075636005, -288.1814473201278588 ) ) ;
#91940 = CARTESIAN_POINT ( 'NONE',  ( 12.15736005180612800, -288.5073287863922360, -324.0846597465782111 ) ) ;
#91941 = ORIENTED_EDGE ( 'NONE', *, *, #52236, .F. ) ;
#91942 = PLANE ( 'NONE',  #18566 ) ;
#91943 = CARTESIAN_POINT ( 'NONE',  ( -112.7120078377118233, -298.3144246460426530, -278.0826589455841145 ) ) ;
#91944 = CARTESIAN_POINT ( 'NONE',  ( -51.69158880102221332, -296.5572342895215456, -195.1580839439134820 ) ) ;
#91945 = CARTESIAN_POINT ( 'NONE',  ( -11.64940865082109411, -279.4537228864278404, -201.7267683024158487 ) ) ;
#91946 = ORIENTED_EDGE ( 'NONE', *, *, #34351, .F. ) ;
#91947 = EDGE_CURVE ( 'NONE', #8082, #18551, #85577, .T. ) ;
#91948 = CARTESIAN_POINT ( 'NONE',  ( 37.57642738403805538, -274.8399216343725016, -252.7880495320005707 ) ) ;
#91949 = CARTESIAN_POINT ( 'NONE',  ( -96.64687811334589185, -295.6396275759994410, -226.5950656291205405 ) ) ;
#91950 = CARTESIAN_POINT ( 'NONE',  ( -35.05626805444299521, -278.8835642863836028, -344.5611333663245546 ) ) ;
#91951 = CARTESIAN_POINT ( 'NONE',  ( 28.97518455151838168, -273.2465126446829800, -237.0004182916892432 ) ) ;
#91952 = CARTESIAN_POINT ( 'NONE',  ( -90.68532492310458792, -297.0342764166445590, -320.8484608131063283 ) ) ;
#91953 = CARTESIAN_POINT ( 'NONE',  ( -34.27455773902066483, -296.0923594263009022, -343.6060407542240114 ) ) ;
#91954 = CARTESIAN_POINT ( 'NONE',  ( 200.8419735307467420, 26.78103457774642138, 10.49999999999999822 ) ) ;
#91955 = CARTESIAN_POINT ( 'NONE',  ( -55.85598205364291147, -296.8868124432819968, -344.2777046070123106 ) ) ;
#91956 = CARTESIAN_POINT ( 'NONE',  ( -64.84684375226086672, -295.6937435332915243, -200.3519702175213979 ) ) ;
#91957 = CARTESIAN_POINT ( 'NONE',  ( -3.596568554813896590, -293.1613592672813979, -205.5139224875146056 ) ) ;
#91958 = CARTESIAN_POINT ( 'NONE',  ( 1.105749626554779264, -275.3545969431295362, -203.8180340006146594 ) ) ;
#91959 = CARTESIAN_POINT ( 'NONE',  ( -100.2056147587211541, -289.6495546316100445, -232.1053582376200666 ) ) ;
#91960 = CARTESIAN_POINT ( 'NONE',  ( 208.8044539878574426, 30.13468703429182227, 15.11452430534868618 ) ) ;
#91961 = CARTESIAN_POINT ( 'NONE',  ( -92.12964482789575982, -273.7870400243897393, -216.3443796625153084 ) ) ;
#91962 = CARTESIAN_POINT ( 'NONE',  ( -109.1621552512183797, -296.7106070021491746, -283.6178463856912799 ) ) ;
#91963 = CARTESIAN_POINT ( 'NONE',  ( -45.12901951119007293, -281.9340233236259223, -195.3575115912544220 ) ) ;
#91964 = CARTESIAN_POINT ( 'NONE',  ( 39.14832307778954856, -280.1958719896468892, -267.0952412762640620 ) ) ;
#91965 = CARTESIAN_POINT ( 'NONE',  ( -84.80998275992679680, -277.0354545267573485, -330.9273373640988325 ) ) ;
#91966 = CARTESIAN_POINT ( 'NONE',  ( -6.534919710642594026, -278.8498476236773627, -200.6520660626392782 ) ) ;
#91967 = CARTESIAN_POINT ( 'NONE',  ( 30.38103407202071082, -279.1220303900754516, -237.6274914876550497 ) ) ;
#91968 = ADVANCED_FACE ( 'NONE', ( #57711 ), #29640, .T. ) ;
#91969 = CARTESIAN_POINT ( 'NONE',  ( 15.88543004276931825, -273.3990933848373288, -219.4715144374321483 ) ) ;
#91970 = CARTESIAN_POINT ( 'NONE',  ( -88.12214496503453631, -279.7625257247373725, -325.6245846552706098 ) ) ;
#91971 = CARTESIAN_POINT ( 'NONE',  ( 175.2296996224750103, 20.99999999999998934, 0.000000000000000000 ) ) ;
#91972 = CIRCLE ( 'NONE', #46612, 1.000000000000000888 ) ;
#91973 = FACE_OUTER_BOUND ( 'NONE', #43521, .T. ) ;
#91974 = CARTESIAN_POINT ( 'NONE',  ( -40.37703197663353194, -296.2544867127755310, -194.3836547306584919 ) ) ;
#91975 = CARTESIAN_POINT ( 'NONE',  ( -36.37836834806066122, -292.0639173955225374, -193.3541118592440000 ) ) ;
#91976 = EDGE_CURVE ( 'NONE', #71100, #88143, #86556, .T. ) ;
#91977 = CARTESIAN_POINT ( 'NONE',  ( 21.22887725293852768, -278.1992681506508802, -317.4932249393975212 ) ) ;
#91978 = CARTESIAN_POINT ( 'NONE',  ( 14.90774451288066693, -272.7886193610837609, -216.5559492543085014 ) ) ;
#91979 = CARTESIAN_POINT ( 'NONE',  ( 193.1191634708854110, 250.0000000000000000, 16.90039380915348843 ) ) ;
#91980 = CARTESIAN_POINT ( 'NONE',  ( -3.515140457016934672, -284.5293911776420828, -337.9408604897415103 ) ) ;
#91981 = SURFACE_STYLE_FILL_AREA ( #84874 ) ;
#91982 = CARTESIAN_POINT ( 'NONE',  ( 7.768505764125121615, -284.6675049210330712, -210.3796399163485091 ) ) ;
#91983 = CARTESIAN_POINT ( 'NONE',  ( 207.6175730408114930, 30.32598770090644180, 14.41714557868295898 ) ) ;
#91984 = CARTESIAN_POINT ( 'NONE',  ( -23.45868950761676786, -293.6657704200166563, -342.4851353964479017 ) ) ;
#91985 = CARTESIAN_POINT ( 'NONE',  ( 26.75072558276606927, -286.1985290916646818, -307.9196834629384512 ) ) ;
#91986 = CARTESIAN_POINT ( 'NONE',  ( 158.9078607026220595, 17.25638377771136334, -9.432942837125283475 ) ) ;
#91987 = CARTESIAN_POINT ( 'NONE',  ( 28.91325046412860189, -292.0193218077198480, -305.6186068693261859 ) ) ;
#91988 = CARTESIAN_POINT ( 'NONE',  ( -21.11238584718955380, -284.7366129088260891, -195.8002897356844301 ) ) ;
#91989 = CARTESIAN_POINT ( 'NONE',  ( -88.09543143389169018, -280.9281100523474493, -216.7134359059565725 ) ) ;
#91990 = CARTESIAN_POINT ( 'NONE',  ( 38.57968083735106291, -288.6290522371708107, -260.1654016927717521 ) ) ;
#91991 = CARTESIAN_POINT ( 'NONE',  ( 32.25394314418228703, -279.3978389811244938, -239.8583238657862751 ) ) ;
#91992 = CARTESIAN_POINT ( 'NONE',  ( 34.75922159645808307, -287.7038752945713327, -281.8625601182478704 ) ) ;
#91993 = CARTESIAN_POINT ( 'NONE',  ( -39.73846186487903509, -281.4467730477243776, -196.7983073072052775 ) ) ;
#91994 = CARTESIAN_POINT ( 'NONE',  ( 23.81189559993686800, -281.7983218556843212, -230.1096022833589529 ) ) ;
#91995 = CARTESIAN_POINT ( 'NONE',  ( 8.783644447499016295, -288.6609627192716516, -210.7720301598189394 ) ) ;
#91996 = EDGE_LOOP ( 'NONE', ( #15269, #44787, #37744, #7698 ) ) ;
#91997 = CARTESIAN_POINT ( 'NONE',  ( -75.77806400934161957, -297.3875275589903140, -203.5792702333208126 ) ) ;
#91998 = CARTESIAN_POINT ( 'NONE',  ( -111.9814579140253556, -292.5208526317213682, -271.2290795190710924 ) ) ;
#91999 = CARTESIAN_POINT ( 'NONE',  ( 209.5646630284975629, 29.26077267968336315, 13.08022668053246740 ) ) ;
#92000 = CARTESIAN_POINT ( 'NONE',  ( -88.52914483777347243, -299.9090924074130271, -206.2264541496106460 ) ) ;
#92001 = VERTEX_POINT ( 'NONE', #51975 ) ;
#92002 = CARTESIAN_POINT ( 'NONE',  ( -68.07070580768768764, -271.6494982618768859, -201.7485503678572343 ) ) ;
#92003 = CARTESIAN_POINT ( 'NONE',  ( 196.8803347170859865, 73.40565171261609123, 12.49999999999999289 ) ) ;
#92004 = CARTESIAN_POINT ( 'NONE',  ( -110.8259917662915370, -294.6968267037566420, -290.5229457555069530 ) ) ;
#92005 = CARTESIAN_POINT ( 'NONE',  ( 51.77000390654524864, -298.7049638229934203, -197.3073222814579708 ) ) ;
#92006 = CARTESIAN_POINT ( 'NONE',  ( -73.87198977184749538, -291.0667790645606487, -334.3775839084418635 ) ) ;
#92007 = PRODUCT_DEFINITION_SHAPE ( 'NONE', 'NONE',  #93723 ) ;
#92008 = CARTESIAN_POINT ( 'NONE',  ( 36.44112851301330380, -283.3963049185937848, -276.8175352054258838 ) ) ;
#92009 = CARTESIAN_POINT ( 'NONE',  ( -110.9693100189715125, -291.7194235732703760, -290.7959254338969117 ) ) ;
#92010 = CARTESIAN_POINT ( 'NONE',  ( -99.46000844568962407, -291.2712631964897128, -315.0446589745617416 ) ) ;
#92011 = CARTESIAN_POINT ( 'NONE',  ( -69.65919759463426431, -287.6268861137378394, -202.6669655641330507 ) ) ;
#92012 = CARTESIAN_POINT ( 'NONE',  ( -16.99403352886174190, -280.4745445257507868, -196.0982573559109881 ) ) ;
#92013 = CARTESIAN_POINT ( 'NONE',  ( -110.2099275173082020, -294.3768527458136646, -290.3495055397546025 ) ) ;
#92014 = CARTESIAN_POINT ( 'NONE',  ( 25.10604466883235020, -281.9830244842723914, -315.4310201944050505 ) ) ;
#92015 = CARTESIAN_POINT ( 'NONE',  ( 34.70229330404547596, -277.1802454070192994, -252.4578084109721487 ) ) ;
#92016 = CARTESIAN_POINT ( 'NONE',  ( -110.4683760289727132, -299.2662352645559167, -253.7030783399848985 ) ) ;
#92017 = CARTESIAN_POINT ( 'NONE',  ( 36.95933304926105478, -273.5895259923603362, -254.3831637393510050 ) ) ;
#92018 = FACE_OUTER_BOUND ( 'NONE', #53093, .T. ) ;
#92019 = CARTESIAN_POINT ( 'NONE',  ( 33.99914805675263807, -281.2675685681434743, -286.1241069803528490 ) ) ;
#92020 = CARTESIAN_POINT ( 'NONE',  ( -111.7856387412321197, -279.5295139327766378, -288.4744952184310591 ) ) ;
#92021 = CARTESIAN_POINT ( 'NONE',  ( -103.8306470437137534, -284.1124130479129235, -231.8882622163514782 ) ) ;
#92022 = CARTESIAN_POINT ( 'NONE',  ( -41.67426004594123867, -293.7571183094771641, -196.4241610917527510 ) ) ;
#92023 = CARTESIAN_POINT ( 'NONE',  ( -87.52499333443032015, -274.9659601317374040, -212.9491883737881039 ) ) ;
#92024 = CARTESIAN_POINT ( 'NONE',  ( -99.17842488240971477, -274.4700719676970380, -225.2230780620052712 ) ) ;
#92025 = DIRECTION ( 'NONE',  ( 0.000000000000000000, 0.000000000000000000, 1.000000000000000000 ) ) ;
#92026 = CARTESIAN_POINT ( 'NONE',  ( 33.89279848684195429, -275.5967291786685678, -286.3755898579345853 ) ) ;
#92027 = CARTESIAN_POINT ( 'NONE',  ( -94.46578244691021098, -297.8818750915947930, -318.7221195585580062 ) ) ;
#92028 = CARTESIAN_POINT ( 'NONE',  ( -40.01451821524881325, -284.0183229289527844, -195.5755279760670078 ) ) ;
#92029 = CARTESIAN_POINT ( 'NONE',  ( 39.58559932006338755, -293.2541105181479111, -273.1780118490173095 ) ) ;
#92030 = CARTESIAN_POINT ( 'NONE',  ( 33.63344882615579223, -273.2703432677488991, -247.0781140317762947 ) ) ;
#92031 = CARTESIAN_POINT ( 'NONE',  ( 34.32707485210553955, -289.4843486069773917, -296.3996331080620621 ) ) ;
#92032 = CARTESIAN_POINT ( 'NONE',  ( -110.0979748727744720, -289.3544335453830740, -279.3472494500714447 ) ) ;
#92033 = ORIENTED_EDGE ( 'NONE', *, *, #75740, .F. ) ;
#92034 = CARTESIAN_POINT ( 'NONE',  ( -8.714997057639369160, -290.9942222789335915, -199.5153830048110422 ) ) ;
#92035 = CARTESIAN_POINT ( 'NONE',  ( -110.2665035933152780, -290.2799426631613073, -265.7300492090016064 ) ) ;
#92036 = EDGE_LOOP ( 'NONE', ( #81403, #61680 ) ) ;
#92037 = CARTESIAN_POINT ( 'NONE',  ( 23.60736984058561916, -288.0084566337292244, -223.7917301608247556 ) ) ;
#92038 = CARTESIAN_POINT ( 'NONE',  ( -89.49165153032868147, -279.6257366972444061, -219.1771265859307505 ) ) ;
#92039 = ADVANCED_FACE ( 'NONE', ( #15074 ), #3945, .T. ) ;
#92040 = CARTESIAN_POINT ( 'NONE',  ( -94.43070419324349984, -294.7747330633922616, -321.5894578174184062 ) ) ;
#92041 = CARTESIAN_POINT ( 'NONE',  ( -12.74417551216628652, -287.0151327517111781, -197.5032112793357157 ) ) ;
#92042 = CARTESIAN_POINT ( 'NONE',  ( -43.66876323159878126, -286.3076894294931662, -193.5894754655832912 ) ) ;
#92044 = CARTESIAN_POINT ( 'NONE',  ( -37.53631795842395746, -283.3879720882690094, -343.3944356157275593 ) ) ;
#92043 = TOROIDAL_SURFACE ( 'NONE', #61845, 1.000000000000000000, 0.5000000000000000000 ) ;
#92045 = CARTESIAN_POINT ( 'NONE',  ( -104.3679765323354616, -256.1617121061207740, -326.7344306583073035 ) ) ;
#92046 = CARTESIAN_POINT ( 'NONE',  ( 4.264052385521533317, -57.87785853924207657, -353.4280301830093549 ) ) ;
#92047 = CARTESIAN_POINT ( 'NONE',  ( 166.5363578158908240, 230.4628405918484475, -189.9770653364864472 ) ) ;
#92048 = CARTESIAN_POINT ( 'NONE',  ( 34.32067219484060416, -274.9432610931079353, -285.0956393696828286 ) ) ;
#92049 = CARTESIAN_POINT ( 'NONE',  ( 24.05988102136718254, -273.9198550864552431, -230.3102515012598133 ) ) ;
#92050 = CARTESIAN_POINT ( 'NONE',  ( -112.2130229303147928, -296.2815456867034527, -252.6463804626246201 ) ) ;
#92051 = CARTESIAN_POINT ( 'NONE',  ( -92.95586860365406778, -239.4756788387215352, -338.8937605817495751 ) ) ;
#92052 = CARTESIAN_POINT ( 'NONE',  ( 12.37139436456461716, -275.0612863531230801, -328.5152795485695947 ) ) ;
#92053 = CARTESIAN_POINT ( 'NONE',  ( -92.79201071169505610, -275.0030598458685063, -221.3382960424069097 ) ) ;
#92054 = CARTESIAN_POINT ( 'NONE',  ( -49.75453633662386466, -292.9699190552871642, -198.0589850946062995 ) ) ;
#92055 = ORIENTED_EDGE ( 'NONE', *, *, #24425, .F. ) ;
#92056 = CARTESIAN_POINT ( 'NONE',  ( -113.5426695157466952, -297.6098935921430666, -261.0749736215325356 ) ) ;
#92057 = CARTESIAN_POINT ( 'NONE',  ( 35.61368441934300222, -287.9814376395827935, -265.5764307693015098 ) ) ;
#92058 = CARTESIAN_POINT ( 'NONE',  ( -33.43280527484429143, -295.8069798995209680, -347.1132439189937031 ) ) ;
#92059 = CARTESIAN_POINT ( 'NONE',  ( -90.66490207147944602, -296.2757623633210642, -325.8976296311550982 ) ) ;
#92060 = CARTESIAN_POINT ( 'NONE',  ( 32.62846924756416200, -293.4413093988539458, -249.3740805853048812 ) ) ;
#92061 = VERTEX_POINT ( 'NONE', #43935 ) ;
#92062 = CARTESIAN_POINT ( 'NONE',  ( 37.06964831873957422, -277.3040884406809141, -257.1623273905797760 ) ) ;
#92063 = VERTEX_POINT ( 'NONE', #72832 ) ;
#92064 = CARTESIAN_POINT ( 'NONE',  ( -50.92260395706821896, -279.3907192836596778, -194.6307676977707501 ) ) ;
#92065 = PRODUCT_DEFINITION_CONTEXT ( 'detailed design', #17230, 'design' ) ;
#92066 = CARTESIAN_POINT ( 'NONE',  ( -92.89733007106960372, -278.8161941620347761, -318.0788340878128224 ) ) ;
#92067 = CARTESIAN_POINT ( 'NONE',  ( -16.08263755026676023, -276.0833610950304546, -197.3542936509817025 ) ) ;
#92068 = CARTESIAN_POINT ( 'NONE',  ( -111.4526897081685206, -276.3970826590530692, -284.0691491544161522 ) ) ;
#92069 = CARTESIAN_POINT ( 'NONE',  ( -109.1473611472535765, -297.3849921027006076, -256.5889477398108625 ) ) ;
#92070 = CARTESIAN_POINT ( 'NONE',  ( -109.1709386364213543, -294.9175278265370821, -286.3590995554434926 ) ) ;
#92071 = CARTESIAN_POINT ( 'NONE',  ( 208.6208076322478746, 32.98517505407394168, 10.50000000000000000 ) ) ;
#92072 = CARTESIAN_POINT ( 'NONE',  ( -42.43224750726681549, -280.4819101112354360, -193.5912460883368738 ) ) ;
#92073 = CARTESIAN_POINT ( 'NONE',  ( 25.37665491622757230, -276.2324032763314676, -307.7162775328546331 ) ) ;
#92074 = CARTESIAN_POINT ( 'NONE',  ( 4.921299900166357766, -285.2947579352629646, -206.5238996140087124 ) ) ;
#92075 = CARTESIAN_POINT ( 'NONE',  ( -84.09644513435723923, -299.4112751574487561, -211.5051731440177321 ) ) ;
#92076 = CARTESIAN_POINT ( 'NONE',  ( 82.62096999362312033, -301.7479467211907149, -196.5710693965175437 ) ) ;
#92077 = CARTESIAN_POINT ( 'NONE',  ( 31.54801855125912624, -287.0765860671094174, -294.9945990004187593 ) ) ;
#92078 = CARTESIAN_POINT ( 'NONE',  ( -79.61554045679248759, -277.7119601983326902, -209.6083696056004442 ) ) ;
#92080 = CARTESIAN_POINT ( 'NONE',  ( -110.3973360645508421, -282.4471423871152638, -284.6505636823185341 ) ) ;
#92079 = CARTESIAN_POINT ( 'NONE',  ( -11.51952119948420439, -278.9697806391696986, -201.3972093027971937 ) ) ;
#92081 = CARTESIAN_POINT ( 'NONE',  ( -10.34543797468004911, -288.4045760319200440, -200.3745887515610775 ) ) ;
#92082 = CARTESIAN_POINT ( 'NONE',  ( -83.24319208077670851, -278.9018947472122250, -327.6994059298249340 ) ) ;
#92083 = CARTESIAN_POINT ( 'NONE',  ( 175.2296996224750103, 215.0000000000000568, 0.000000000000000000 ) ) ;
#92084 = CARTESIAN_POINT ( 'NONE',  ( -17.18914787079680906, -294.3124661108431610, -198.1193344808359029 ) ) ;
#92085 = CARTESIAN_POINT ( 'NONE',  ( -98.00811692064213787, -276.1743449035008666, -316.1379165729312604 ) ) ;
#92086 = CARTESIAN_POINT ( 'NONE',  ( -56.61907550713243609, -277.9585795022109096, -340.9280509072449377 ) ) ;
#92087 = CARTESIAN_POINT ( 'NONE',  ( 23.63533713568915928, -284.1495149366861028, -314.3355571250510820 ) ) ;
#92088 = DIRECTION ( 'NONE',  ( -0.000000000000000000, 1.000000000000000000, 0.000000000000000000 ) ) ;
#92089 = CARTESIAN_POINT ( 'NONE',  ( -38.86614059597783211, -290.9912866863014642, -345.9057424287087201 ) ) ;
#92090 = CARTESIAN_POINT ( 'NONE',  ( -111.1827526396086796, -294.3824330138968435, -283.5667972832322903 ) ) ;
#92091 = EDGE_CURVE ( 'NONE', #87260, #26725, #65769, .T. ) ;
#92092 = CARTESIAN_POINT ( 'NONE',  ( 193.5659903145831038, 249.5000000000000568, 16.24901362097127233 ) ) ;
#92093 = CARTESIAN_POINT ( 'NONE',  ( 3.215954506125094259, -273.2941128010002103, -209.0114635707370496 ) ) ;
#92094 = CARTESIAN_POINT ( 'NONE',  ( 15.77561970220103404, -290.9532700453690950, -218.4278891622215326 ) ) ;
#92095 = DIRECTION ( 'NONE',  ( -1.000000000000000000, 0.000000000000000000, 0.000000000000000000 ) ) ;
#92096 = FACE_OUTER_BOUND ( 'NONE', #35918, .T. ) ;
#92097 = CARTESIAN_POINT ( 'NONE',  ( -90.29077295507200063, -289.7996606162673174, -215.3414338584399843 ) ) ;
#92098 = CARTESIAN_POINT ( 'NONE',  ( -94.89624433596443964, -285.5063151616044479, -316.5755298017816131 ) ) ;
#92099 = CARTESIAN_POINT ( 'NONE',  ( 17.63406156653762480, -285.0644993850514197, -217.8291359498942086 ) ) ;
#92100 = CARTESIAN_POINT ( 'NONE',  ( -108.6598237742127537, -285.7399014278877871, -288.5022358712301980 ) ) ;
#92101 = EDGE_CURVE ( 'NONE', #28861, #53738, #10278, .T. ) ;
#92102 = CARTESIAN_POINT ( 'NONE',  ( -74.81157098468700895, -286.3422261880000974, -207.5231477339215758 ) ) ;
#92103 = CARTESIAN_POINT ( 'NONE',  ( -110.4061193128121943, -292.7683902754417886, -251.8700526055010016 ) ) ;
#92104 = CIRCLE ( 'NONE', #48300, 6.499999999999977796 ) ;
#92105 = CARTESIAN_POINT ( 'NONE',  ( 38.18290392137456735, -273.6783662369252852, -273.9994752100878372 ) ) ;
#92106 = CARTESIAN_POINT ( 'NONE',  ( 32.53208464009873069, -275.4706213075840537, -237.9325165720736948 ) ) ;
#92107 = CARTESIAN_POINT ( 'NONE',  ( -108.5175170296699463, -288.3039852311906657, -295.8800774431864511 ) ) ;
#92108 = CARTESIAN_POINT ( 'NONE',  ( -69.01537505253617155, -277.4572722322339473, -340.5594118909148165 ) ) ;
#92109 = CARTESIAN_POINT ( 'NONE',  ( -85.52092927726266680, -297.7017159697305146, -327.4430724511720427 ) ) ;
#92110 = CARTESIAN_POINT ( 'NONE',  ( -43.52943240505717171, -249.3936360501505476, -482.3142747188312569 ) ) ;
#92111 = CARTESIAN_POINT ( 'NONE',  ( 0.000000000000000000, 131.0000000000000568, 11.50000000000000000 ) ) ;
#92112 = CARTESIAN_POINT ( 'NONE',  ( -101.4130973739320893, -283.7275272302651388, -234.2554835568423073 ) ) ;
#92113 = CARTESIAN_POINT ( 'NONE',  ( -20.18823718843633586, -278.2722409054376271, -197.2957160965913204 ) ) ;
#92114 = DIRECTION ( 'NONE',  ( -1.124465274301078034E-16, -1.000000000000000000, -0.000000000000000000 ) ) ;
#92115 = CARTESIAN_POINT ( 'NONE',  ( 38.04568002670000482, -273.8819406966314318, -258.4678354807006144 ) ) ;
#92116 = CARTESIAN_POINT ( 'NONE',  ( -24.31958225480821056, -276.2302156437014560, -342.3453661107727726 ) ) ;
#92117 = CARTESIAN_POINT ( 'NONE',  ( 34.45527216119190683, -295.2899890095026194, -287.0270891889493896 ) ) ;
#92118 = CARTESIAN_POINT ( 'NONE',  ( 22.64218013656804374, -279.8299477325448947, -222.5550216351258257 ) ) ;
#92119 = CARTESIAN_POINT ( 'NONE',  ( -58.46468524604843253, -296.2733044206775048, -340.4840667745914402 ) ) ;
#92120 = CARTESIAN_POINT ( 'NONE',  ( -97.87394220482170226, -297.2387306832472973, -317.1494278878799946 ) ) ;
#92121 = CARTESIAN_POINT ( 'NONE',  ( -69.25561991581021459, -297.4534641100697741, -204.7067066431669673 ) ) ;
#92122 = CARTESIAN_POINT ( 'NONE',  ( -37.58122463873551311, -294.0493461534879884, -195.3487118981795447 ) ) ;
#92123 = CARTESIAN_POINT ( 'NONE',  ( -64.54917640582389993, -285.8733124002492332, -198.3139491388778026 ) ) ;
#92124 = CARTESIAN_POINT ( 'NONE',  ( 25.91257838495116772, -273.1344271491331028, -228.6573803810417473 ) ) ;
#92125 = CARTESIAN_POINT ( 'NONE',  ( 10.22627933519428112, -288.2501738771244959, -330.9788227866316674 ) ) ;
#92126 = CARTESIAN_POINT ( 'NONE',  ( -80.01537981972640523, -281.4513914074202034, -209.1173112602517676 ) ) ;
#92127 = CARTESIAN_POINT ( 'NONE',  ( -104.8096622764974342, -283.9935699379740299, -241.7442901645396205 ) ) ;
#92128 = CARTESIAN_POINT ( 'NONE',  ( -81.69104272750401208, -287.6558560696544191, -330.8436481618447260 ) ) ;
#92129 = CARTESIAN_POINT ( 'NONE',  ( 173.4479467868932829, 229.7134184023448142, -192.0138545908111496 ) ) ;
#92130 = CARTESIAN_POINT ( 'NONE',  ( -6.985220253899331766, -285.9692186405659982, -203.8908324833523125 ) ) ;
#92131 = CARTESIAN_POINT ( 'NONE',  ( 155.6265766802846713, 17.98195150565417322, 10.85854113850158953 ) ) ;
#92132 = CARTESIAN_POINT ( 'NONE',  ( -24.56091773604495998, -283.8342508652153242, -346.1083444665698039 ) ) ;
#92133 = CARTESIAN_POINT ( 'NONE',  ( -61.60281816866072546, -290.8033570143372799, -197.4750708816478380 ) ) ;
#92134 = CARTESIAN_POINT ( 'NONE',  ( -77.09275720576751212, -281.1293841970339145, -205.2900726959945814 ) ) ;
#92135 = CARTESIAN_POINT ( 'NONE',  ( -90.72613789452995547, -280.6297838383227941, -215.4839605343739777 ) ) ;
#92136 = CARTESIAN_POINT ( 'NONE',  ( 28.15013031995771087, -281.8238091456313441, -302.7220703729472007 ) ) ;
#92137 = CARTESIAN_POINT ( 'NONE',  ( 29.63624354911688386, -277.1064677571801553, -236.6127001463279953 ) ) ;
#92138 = CARTESIAN_POINT ( 'NONE',  ( -19.28728046576089383, -294.8261969203741728, -345.2694466029412297 ) ) ;
#92139 = CARTESIAN_POINT ( 'NONE',  ( -103.8642042717651606, -289.0233785415663306, -236.3852448360190408 ) ) ;
#92140 = CARTESIAN_POINT ( 'NONE',  ( -110.6832066223082194, -295.4941334381200591, -268.7122824466516136 ) ) ;
#92141 = ORIENTED_EDGE ( 'NONE', *, *, #19203, .T. ) ;
#92142 = EDGE_LOOP ( 'NONE', ( #13678, #41989, #67012, #27215 ) ) ;
#92143 = CARTESIAN_POINT ( 'NONE',  ( 8.703496828763627846, -284.3360506428081749, -328.9175981098180159 ) ) ;
#92144 = CARTESIAN_POINT ( 'NONE',  ( -108.7989415408142264, -296.4178817797650254, -255.2693763011288297 ) ) ;
#92145 = CARTESIAN_POINT ( 'NONE',  ( -4.748052243191166255, -293.5511440313488265, -200.9410443095753749 ) ) ;
#92146 = CARTESIAN_POINT ( 'NONE',  ( -76.17425371797476430, -284.2371860237928445, -332.3558276395201574 ) ) ;
#92147 = CARTESIAN_POINT ( 'NONE',  ( -29.84988571813216751, -273.2035521339015531, -193.9628658454433889 ) ) ;
#92148 = CARTESIAN_POINT ( 'NONE',  ( -111.8212305396424142, -290.9631960646470361, -289.5478345414990713 ) ) ;
#92149 = CARTESIAN_POINT ( 'NONE',  ( -49.12880950617137898, -284.0432150133303821, -195.4659481531978145 ) ) ;
#92150 = CARTESIAN_POINT ( 'NONE',  ( -113.3385027575013311, -290.7321011129461681, -282.6179642998316126 ) ) ;
#92151 = CARTESIAN_POINT ( 'NONE',  ( 14.10128641238149427, -288.6382868691399040, -322.1849216111931469 ) ) ;
#92152 = CARTESIAN_POINT ( 'NONE',  ( 113.5000000000000568, -218.8335761803644743, -447.4016117689005796 ) ) ;
#92153 = CARTESIAN_POINT ( 'NONE',  ( 150.6539576904058606, 293.9636489450775230, 0.000000000000000000 ) ) ;
#92154 = CARTESIAN_POINT ( 'NONE',  ( 198.9222472290481107, 285.7997244369286705, -96.29823329932079901 ) ) ;
#92155 = CARTESIAN_POINT ( 'NONE',  ( -30.25979458878175166, -284.4842132587976380, -346.3384459577605980 ) ) ;
#92156 = CARTESIAN_POINT ( 'NONE',  ( 35.77081079830085031, -285.2666405000204577, -287.0812184334320705 ) ) ;
#92157 = ORIENTED_EDGE ( 'NONE', *, *, #56521, .T. ) ;
#92158 = CARTESIAN_POINT ( 'NONE',  ( 21.24870238136351830, -281.0888294652893933, -314.4430737902855526 ) ) ;
#92159 = CARTESIAN_POINT ( 'NONE',  ( 36.86410477721120316, -275.4760006315963778, -290.8856773332105377 ) ) ;
#92160 = CARTESIAN_POINT ( 'NONE',  ( -104.7722036336553657, -280.1225945607095014, -302.9332956353616737 ) ) ;
#92161 = CARTESIAN_POINT ( 'NONE',  ( 175.5294223676853562, 240.7679223315280979, -178.2279574903016623 ) ) ;
#92162 = CARTESIAN_POINT ( 'NONE',  ( 38.08327240192149787, -280.2821001480572818, -282.6771018170967977 ) ) ;
#92163 = CARTESIAN_POINT ( 'NONE',  ( -73.14119015358589593, -283.5952883239441462, -204.8466343622566228 ) ) ;
#92164 = CARTESIAN_POINT ( 'NONE',  ( -94.80036233197064632, -297.6315636111481808, -320.0851177538386878 ) ) ;
#92165 = CARTESIAN_POINT ( 'NONE',  ( 35.26881681877143393, -294.1572010639757764, -278.9115201708078757 ) ) ;
#92166 = ORIENTED_EDGE ( 'NONE', *, *, #26705, .F. ) ;
#92167 = CARTESIAN_POINT ( 'NONE',  ( -107.8638171348330701, -289.5093358452252801, -249.6313410613936412 ) ) ;
#92168 = CARTESIAN_POINT ( 'NONE',  ( -18.58288025350287498, -274.9389108772076042, -195.7312371196776724 ) ) ;
#92169 = CARTESIAN_POINT ( 'NONE',  ( -92.91378333311681104, -273.2256387032089719, -223.0053292369560438 ) ) ;
#92170 = ORIENTED_EDGE ( 'NONE', *, *, #73959, .T. ) ;
#92171 = CARTESIAN_POINT ( 'NONE',  ( -97.56176595634224213, -272.1102037436245382, -222.8738967228917716 ) ) ;
#92172 = CARTESIAN_POINT ( 'NONE',  ( 222.4306832106270804, -135.2391364535880882, -21.50000000000000000 ) ) ;
#92173 = DIRECTION ( 'NONE',  ( 1.000000000000000000, -0.000000000000000000, 0.000000000000000000 ) ) ;
#92174 = AXIS2_PLACEMENT_3D ( 'NONE', #49044, #85493, #20640 ) ;
#92175 = DIRECTION ( 'NONE',  ( 0.000000000000000000, 0.000000000000000000, -1.000000000000000000 ) ) ;
#92176 = CARTESIAN_POINT ( 'NONE',  ( 5.784984827709251043, -283.5315821599924675, -329.6427771822853288 ) ) ;
#92177 = CARTESIAN_POINT ( 'NONE',  ( -59.03458198338113050, -281.5353505352627508, -197.5367203637727584 ) ) ;
#92178 = AXIS2_PLACEMENT_3D ( 'NONE', #77918, #36209, #65128 ) ;
#92179 = CARTESIAN_POINT ( 'NONE',  ( -51.07373165187753017, -282.2905828170895575, -342.3492210155351358 ) ) ;
#92180 = CARTESIAN_POINT ( 'NONE',  ( 12.11133522320177036, -282.6091956308266049, -214.9963026891963693 ) ) ;
#92181 = CARTESIAN_POINT ( 'NONE',  ( 23.63682128274491134, -273.4617341466191647, -228.9581937063117607 ) ) ;
#92182 = CARTESIAN_POINT ( 'NONE',  ( 208.0212563688061209, 27.56882951438707607, 12.00000000000000000 ) ) ;
#92183 = CARTESIAN_POINT ( 'NONE',  ( 195.7510731661265595, -164.3527196417747405, -32.50000000000000711 ) ) ;
#92184 = CARTESIAN_POINT ( 'NONE',  ( -97.79552033249345300, -278.7195952539516952, -317.7899535576747780 ) ) ;
#92185 = EDGE_LOOP ( 'NONE', ( #90490, #89313, #83368, #49780 ) ) ;
#92186 = ORIENTED_EDGE ( 'NONE', *, *, #42456, .F. ) ;
#92187 = CARTESIAN_POINT ( 'NONE',  ( 201.2104617360081704, 25.32700003806615641, 10.50000000000000000 ) ) ;
#92188 = CARTESIAN_POINT ( 'NONE',  ( -68.48319767168499084, -285.4391456624471743, -338.9945624313600092 ) ) ;
#92189 = CARTESIAN_POINT ( 'NONE',  ( -2.353237483384341022, -291.7248160040581979, -206.0941923850689363 ) ) ;
#92190 = CARTESIAN_POINT ( 'NONE',  ( 37.04370229184142005, -287.1451181073712178, -289.8579047366315535 ) ) ;
#92191 = CARTESIAN_POINT ( 'NONE',  ( -69.19095982766481256, -283.8671932675695189, -203.5369706117102169 ) ) ;
#92193 = CARTESIAN_POINT ( 'NONE',  ( 1.829139564833170528, -286.7601202057824139, -333.1593610351702637 ) ) ;
#92192 = CARTESIAN_POINT ( 'NONE',  ( -102.7539228424638367, -283.5815338090217779, -236.6473813897290768 ) ) ;
#92194 = CARTESIAN_POINT ( 'NONE',  ( -107.7686164525559889, -285.4847289093170843, -291.0742913940970880 ) ) ;
#92195 = CARTESIAN_POINT ( 'NONE',  ( 35.94575831833729040, -273.7573775859350462, -286.3568093329479325 ) ) ;
#92196 = CARTESIAN_POINT ( 'NONE',  ( 38.18507422594242939, -285.8243005830075276, -260.2543494226483176 ) ) ;
#92197 = CARTESIAN_POINT ( 'NONE',  ( -100.6423988056475878, -299.0935691335796491, -230.1364713737373791 ) ) ;
#92198 = CARTESIAN_POINT ( 'NONE',  ( -92.55533242118022486, -283.2641184400021643, -219.2801281553609556 ) ) ;
#92199 = CARTESIAN_POINT ( 'NONE',  ( -14.24600351129383569, -281.3002647426362728, -200.8093280125607123 ) ) ;
#92200 = CARTESIAN_POINT ( 'NONE',  ( 34.92145991046990616, -289.2844816226241278, -249.4868153894530280 ) ) ;
#92201 = CARTESIAN_POINT ( 'NONE',  ( 196.0602364706492153, 26.06347922710755327, 13.31833675859200916 ) ) ;
#92202 = FACE_OUTER_BOUND ( 'NONE', #30197, .T. ) ;
#92203 = CARTESIAN_POINT ( 'NONE',  ( -101.8728308340789681, -297.9492272323626594, -309.6682085169498464 ) ) ;
#92204 = CARTESIAN_POINT ( 'NONE',  ( -43.90130609867937039, -277.9692035606338436, -195.5969103175798693 ) ) ;
#92205 = CARTESIAN_POINT ( 'NONE',  ( -102.1705312572491664, -289.2064142907390192, -311.7068565704846037 ) ) ;
#92206 = CARTESIAN_POINT ( 'NONE',  ( 4.250634731313062353, -292.8808198747910865, -331.3243699842163323 ) ) ;
#92207 = CARTESIAN_POINT ( 'NONE',  ( -38.34386269574050488, -278.7241583040062096, -196.8623143927832473 ) ) ;
#92208 = CARTESIAN_POINT ( 'NONE',  ( -58.23003210534655949, -295.9188985158894525, -199.1252908642997852 ) ) ;
#92209 = CARTESIAN_POINT ( 'NONE',  ( 13.23045453135390304, -294.0926145982928119, -217.0347581752882604 ) ) ;
#92210 = CARTESIAN_POINT ( 'NONE',  ( -4.829096099716510437, -288.9805209788416391, -202.7746430608542312 ) ) ;
#92211 = CARTESIAN_POINT ( 'NONE',  ( -110.1457271592157241, -295.3237972234453537, -247.3326282225894488 ) ) ;
#92212 = CARTESIAN_POINT ( 'NONE',  ( -78.60502091279583681, -291.2178118523368084, -331.6090555798036235 ) ) ;
#92213 = CARTESIAN_POINT ( 'NONE',  ( 32.40330115951777401, -291.4025775502460078, -240.2013963849918241 ) ) ;
#92214 = CARTESIAN_POINT ( 'NONE',  ( -107.5084575424834128, -291.6837493782022648, -292.7106225379789066 ) ) ;
#92215 = ADVANCED_FACE ( 'NONE', ( #76567 ), #23607, .F. ) ;
#92216 = FACE_OUTER_BOUND ( 'NONE', #54105, .T. ) ;
#92217 = CARTESIAN_POINT ( 'NONE',  ( -95.24845408909473576, -291.9831262664929454, -225.6463600921897807 ) ) ;
#92218 = DIRECTION ( 'NONE',  ( -5.551115123125793746E-15, 0.000000000000000000, 1.000000000000000000 ) ) ;
#92219 = CARTESIAN_POINT ( 'NONE',  ( -113.9720259457677258, -291.7821268469442657, -268.3803722770622926 ) ) ;
#92221 = CARTESIAN_POINT ( 'NONE',  ( 29.85574526842174947, -293.1676665568263047, -241.7098139173920401 ) ) ;
#92220 = CARTESIAN_POINT ( 'NONE',  ( 0.5687818237891290041, -278.5745202268709022, -205.1771869677942277 ) ) ;
#92222 = CARTESIAN_POINT ( 'NONE',  ( -39.58725916897031283, -280.0247176494351038, -193.3808179989841847 ) ) ;
#92223 = CARTESIAN_POINT ( 'NONE',  ( -111.8555693876049872, -283.9763558657629119, -289.7376626467539040 ) ) ;
#92224 = CARTESIAN_POINT ( 'NONE',  ( 23.43617371858514886, -286.1473971568800039, -314.0197766768680481 ) ) ;
#92225 = CARTESIAN_POINT ( 'NONE',  ( 33.92696323495075461, -279.4214710237247346, -249.5850956529434370 ) ) ;
#92226 = CARTESIAN_POINT ( 'NONE',  ( -33.79572641913322428, -284.0966204441852483, -195.4449867343163021 ) ) ;
#92227 = CARTESIAN_POINT ( 'NONE',  ( 28.69632656350021804, -279.5303523302633266, -232.1291054537108778 ) ) ;
#92228 = CARTESIAN_POINT ( 'NONE',  ( 21.86035610847062571, -285.8148781798079767, -221.6106405654452089 ) ) ;
#92229 = CARTESIAN_POINT ( 'NONE',  ( 199.0061125298537377, 249.5000000000000568, -7.725424859374024678 ) ) ;
#92230 = CARTESIAN_POINT ( 'NONE',  ( 15.43350097081438754, -294.4132564806113237, -218.7009453128011671 ) ) ;
#92231 = CARTESIAN_POINT ( 'NONE',  ( 38.72885893514061451, -276.8798855086320145, -262.6218382784726373 ) ) ;
#92232 = CARTESIAN_POINT ( 'NONE',  ( -24.33000313824093297, -276.5482964787728406, -342.2650934989455891 ) ) ;
#92233 = CARTESIAN_POINT ( 'NONE',  ( -112.6404178736079587, -290.9208841501561551, -254.2022223462749366 ) ) ;
#92234 = CARTESIAN_POINT ( 'NONE',  ( -27.58277256195642835, -281.0090946815363964, -345.3406282654490269 ) ) ;
#92236 = CARTESIAN_POINT ( 'NONE',  ( -107.9756624265907163, -289.8656723942427789, -251.0155288570420851 ) ) ;
#92235 = CIRCLE ( 'NONE', #75548, 0.5000000000000004441 ) ;
#92237 = CARTESIAN_POINT ( 'NONE',  ( -92.24326195022581487, -293.8367803861256675, -321.4762157344185880 ) ) ;
#92238 = ORIENTED_EDGE ( 'NONE', *, *, #35647, .T. ) ;
#92239 = CARTESIAN_POINT ( 'NONE',  ( -14.82148196441097454, -291.8596224417491953, -200.8569582839153043 ) ) ;
#92240 = DIRECTION ( 'NONE',  ( 0.000000000000000000, 0.000000000000000000, -1.000000000000000000 ) ) ;
#92241 = CIRCLE ( 'NONE', #9090, 1.000000000000000888 ) ;
#92242 = CARTESIAN_POINT ( 'NONE',  ( 7.450504543161054372, -272.1952119285918457, -214.2458315076590907 ) ) ;
#92243 = CARTESIAN_POINT ( 'NONE',  ( -105.0404320084053182, -296.0812981215323703, -234.0585842990633694 ) ) ;
#92244 = CARTESIAN_POINT ( 'NONE',  ( 36.65396876758700273, -279.8993900819789360, -286.6981247717925498 ) ) ;
#92245 = CARTESIAN_POINT ( 'NONE',  ( -113.0023115558056332, -286.0145593653165861, -258.6635762973609189 ) ) ;
#92246 = CARTESIAN_POINT ( 'NONE',  ( -35.93133902273247315, -285.9036501387922158, -197.3747433220484311 ) ) ;
#92247 = CARTESIAN_POINT ( 'NONE',  ( 1.250861165908237371, -278.0471246036970001, -333.2010361074588332 ) ) ;
#92248 = CARTESIAN_POINT ( 'NONE',  ( -105.4474449543378825, -294.1683133094104505, -301.0400487017277555 ) ) ;
#92249 = CARTESIAN_POINT ( 'NONE',  ( -108.8200541069438003, -298.5630527555596814, -251.1075652290759592 ) ) ;
#92250 = CARTESIAN_POINT ( 'NONE',  ( -100.9344959331764073, -276.8460881183456195, -307.1113789955583115 ) ) ;
#92251 = ORIENTED_EDGE ( 'NONE', *, *, #68560, .T. ) ;
#92252 = CARTESIAN_POINT ( 'NONE',  ( 195.5098343408735957, 40.18270620362346079, 13.84004740867598393 ) ) ;
#92253 = CARTESIAN_POINT ( 'NONE',  ( -112.8671136782256070, -296.4059681149219045, -255.4052258804949815 ) ) ;
#92254 = CARTESIAN_POINT ( 'NONE',  ( 29.53190838839401167, -289.9066480218052675, -303.0602720826641985 ) ) ;
#92255 = CARTESIAN_POINT ( 'NONE',  ( 200.4551663813218170, 64.49084098419280053, -5.329070518200752656E-14 ) ) ;
#92256 = CARTESIAN_POINT ( 'NONE',  ( 28.32295606611701189, -288.6381113537674423, -302.4865844340063745 ) ) ;
#92257 = ORIENTED_EDGE ( 'NONE', *, *, #61720, .T. ) ;
#92258 = CARTESIAN_POINT ( 'NONE',  ( -71.12022602912675495, -278.6759169596537049, -201.4275891154477449 ) ) ;
#92259 = CARTESIAN_POINT ( 'NONE',  ( -111.5259488317175851, -297.4597361964793549, -249.9155729426356629 ) ) ;
#92260 = CARTESIAN_POINT ( 'NONE',  ( -110.7911859833681234, -288.9287032777452850, -251.7218752484802735 ) ) ;
#92261 = CARTESIAN_POINT ( 'NONE',  ( -114.2124237528593511, -296.8231197402293446, -275.3422355777246935 ) ) ;
#92262 = CARTESIAN_POINT ( 'NONE',  ( 33.46760488580594028, -294.1207624177496882, -288.1973118116284240 ) ) ;
#92263 = CARTESIAN_POINT ( 'NONE',  ( 197.0949311480472659, 69.78325229578651090, -10.59408097397595405 ) ) ;
#92264 = CARTESIAN_POINT ( 'NONE',  ( 140.6539576904058606, 275.5000000000000568, 12.50000000000000000 ) ) ;
#92265 = DIRECTION ( 'NONE',  ( 1.000000000000000000, 0.000000000000000000, 0.000000000000000000 ) ) ;
#92266 = CARTESIAN_POINT ( 'NONE',  ( 32.24064525209211496, -289.4759654089318701, -301.6821167265741224 ) ) ;
#92267 = CARTESIAN_POINT ( 'NONE',  ( -99.90806341382572953, -281.6948066931272479, -220.5068182859052968 ) ) ;
#92268 = EDGE_CURVE ( 'NONE', #28384, #75749, #30980, .T. ) ;
#92269 = CARTESIAN_POINT ( 'NONE',  ( 26.20107647552291041, -280.3277403440131934, -226.9596683785739799 ) ) ;
#92270 = CARTESIAN_POINT ( 'NONE',  ( -92.06517812412242563, -285.8362080835908046, -321.4039370950949888 ) ) ;
#92271 = EDGE_CURVE ( 'NONE', #31343, #16501, #60501, .T. ) ;
#92272 = CARTESIAN_POINT ( 'NONE',  ( 25.88012464252941669, -285.5564764560488697, -227.4237860734758954 ) ) ;
#92273 = CARTESIAN_POINT ( 'NONE',  ( -111.7467798112649433, -288.5855052615702334, -273.9545584431152179 ) ) ;
#92274 = CARTESIAN_POINT ( 'NONE',  ( 38.39547106792315390, -277.3865629595952669, -268.3150541804079694 ) ) ;
#92275 = ORIENTED_EDGE ( 'NONE', *, *, #6687, .F. ) ;
#92277 = CARTESIAN_POINT ( 'NONE',  ( 35.13497451868102672, -280.7700919818917100, -260.4437811557052669 ) ) ;
#92276 = CARTESIAN_POINT ( 'NONE',  ( -108.4862654471839960, -278.3356859625646393, -286.7704393067185720 ) ) ;
#92278 = CARTESIAN_POINT ( 'NONE',  ( 38.43252789911300482, -276.7844557826115306, -282.5167594656351753 ) ) ;
#92279 = CARTESIAN_POINT ( 'NONE',  ( -59.17421544043035198, -278.5706110470615045, -196.9353051318821315 ) ) ;
#92280 = CARTESIAN_POINT ( 'NONE',  ( 101.3885564533947132, 116.0994877786729944, -280.6488961443201902 ) ) ;
#92281 = CARTESIAN_POINT ( 'NONE',  ( -49.69323055338989548, -274.8396986135285829, -194.5429730840638172 ) ) ;
#92282 = CARTESIAN_POINT ( 'NONE',  ( -108.5268680866647486, -274.4252176589839110, -242.7314046901510949 ) ) ;
#92283 = CARTESIAN_POINT ( 'NONE',  ( -106.6662871844225293, -287.4805209788416391, -237.0123917617630980 ) ) ;
#92284 = CARTESIAN_POINT ( 'NONE',  ( 129.9467878515196162, -299.5541904835127980, -200.7046326357662167 ) ) ;
#92285 = CARTESIAN_POINT ( 'NONE',  ( 31.25901186464348669, -288.2866270422087496, -244.3689389846792892 ) ) ;
#92286 = CARTESIAN_POINT ( 'NONE',  ( 22.18389846867367865, -288.6715833538992797, -223.1103425658456558 ) ) ;
#92287 = CARTESIAN_POINT ( 'NONE',  ( 28.31568157913729777, -287.3354945827409210, -302.5014492686228778 ) ) ;
#92288 = CARTESIAN_POINT ( 'NONE',  ( -110.8653598411162307, -284.3467323289016804, -247.5147273865749469 ) ) ;
#92289 = CARTESIAN_POINT ( 'NONE',  ( -70.07699919036306824, -278.0133875953563347, -204.2045452565980383 ) ) ;
#92290 = CARTESIAN_POINT ( 'NONE',  ( -49.64925598126998807, -287.7541078901966216, -197.1008938015943102 ) ) ;
#92291 = CARTESIAN_POINT ( 'NONE',  ( 11.78226379117393208, -279.2292019679542250, -215.4289423501730596 ) ) ;
#92292 = CARTESIAN_POINT ( 'NONE',  ( -59.32667500354519063, -278.6579949677140462, -340.4888896342499152 ) ) ;
#92293 = CARTESIAN_POINT ( 'NONE',  ( -32.41014727835776199, -277.4807887021507895, -343.3060384995462755 ) ) ;
#92294 = CARTESIAN_POINT ( 'NONE',  ( -40.33866810305801920, -287.8839397658408075, -346.9184127381960252 ) ) ;
#92295 = CARTESIAN_POINT ( 'NONE',  ( 19.67058461752129261, -283.0566368584561019, -321.9536152058485641 ) ) ;
#92296 = CARTESIAN_POINT ( 'NONE',  ( -112.1578352728291463, -284.8191745609818781, -288.3632571558972586 ) ) ;
#92297 = CARTESIAN_POINT ( 'NONE',  ( 24.13158749145670257, -282.2645867068694088, -309.8245316795982376 ) ) ;
#92298 = ORIENTED_EDGE ( 'NONE', *, *, #17686, .F. ) ;
#92299 = ORIENTED_EDGE ( 'NONE', *, *, #84612, .T. ) ;
#92300 = CARTESIAN_POINT ( 'NONE',  ( 121.3395553409046528, -296.8152984961567427, -195.3611179825600175 ) ) ;
#92301 = CARTESIAN_POINT ( 'NONE',  ( -110.8028588639680123, -292.6489333521008689, -251.7679302346301711 ) ) ;
#92302 = CARTESIAN_POINT ( 'NONE',  ( -40.59458186991012241, -290.6969084256586484, -193.9103524594466990 ) ) ;
#92303 = CARTESIAN_POINT ( 'NONE',  ( -72.00855973548746647, -272.6409959338194540, -205.7940179997810048 ) ) ;
#92304 = CARTESIAN_POINT ( 'NONE',  ( 37.35900325008093148, -293.1299764320229997, -288.6677030066111342 ) ) ;
#92305 = AXIS2_PLACEMENT_3D ( 'NONE', #32413, #18664, #68866 ) ;
#92306 = CARTESIAN_POINT ( 'NONE',  ( -40.00235977253007036, -287.5659332485013238, -344.0564582181897322 ) ) ;
#92308 = EDGE_CURVE ( 'NONE', #89567, #71577, #31155, .T. ) ;
#92307 = CARTESIAN_POINT ( 'NONE',  ( 32.76805845636194192, -291.4793028913970829, -246.4823313087376846 ) ) ;
#92309 = CARTESIAN_POINT ( 'NONE',  ( -39.95682695602013013, -290.2906886463000546, -343.7614352514647180 ) ) ;
#92310 = DIRECTION ( 'NONE',  ( 0.000000000000000000, 0.000000000000000000, 1.000000000000000000 ) ) ;
#92311 = CARTESIAN_POINT ( 'NONE',  ( -92.11430713159376182, -291.8342549182078756, -321.6703205373823948 ) ) ;
#92312 = CARTESIAN_POINT ( 'NONE',  ( -94.25569371910715688, -289.2314237010997999, -221.2412922283180308 ) ) ;
#92313 = CIRCLE ( 'NONE', #40852, 24.00000000000000355 ) ;
#92314 = CARTESIAN_POINT ( 'NONE',  ( -79.00362692893637018, -293.4909826529812449, -207.9352936989693603 ) ) ;
#92315 = CARTESIAN_POINT ( 'NONE',  ( 13.29360894974098173, -287.7224703606501635, -217.3811099711532790 ) ) ;
#92316 = CARTESIAN_POINT ( 'NONE',  ( 26.48189180133820031, -295.0190670001029503, -230.5566810147311685 ) ) ;
#92317 = CARTESIAN_POINT ( 'NONE',  ( 196.8409580319986674, 73.46773880466290052, -12.56795567929779445 ) ) ;
#92318 = CARTESIAN_POINT ( 'NONE',  ( 180.6209651459523968, 275.5000000000000568, -24.41176470588238345 ) ) ;
#92319 = CARTESIAN_POINT ( 'NONE',  ( -5.825641502940878347, -276.4443388915217383, -201.9129999996004017 ) ) ;
#92320 = CARTESIAN_POINT ( 'NONE',  ( -113.9589469772315908, -295.8306235535918631, -263.8738918065893131 ) ) ;
#92321 = CARTESIAN_POINT ( 'NONE',  ( 1.158457435358022369, -272.8137145038447784, -207.1494744294204509 ) ) ;
#92322 = CARTESIAN_POINT ( 'NONE',  ( -107.7999268318789632, -276.9468911568533827, -246.1831459873743313 ) ) ;
#92323 = CARTESIAN_POINT ( 'NONE',  ( -87.61640209655796241, -274.5366816873591915, -216.8164309816662580 ) ) ;
#92324 = CARTESIAN_POINT ( 'NONE',  ( -90.82307977799618470, -297.2544374603523352, -320.9826472191942912 ) ) ;
#92325 = FACE_OUTER_BOUND ( 'NONE', #67726, .T. ) ;
#92326 = CARTESIAN_POINT ( 'NONE',  ( -104.9152558011691241, -297.7302119871392279, -242.3180029591451330 ) ) ;
#92327 = DIRECTION ( 'NONE',  ( 1.000000000000000000, 0.000000000000000000, 0.000000000000000000 ) ) ;
#92329 = CARTESIAN_POINT ( 'NONE',  ( -68.04752391275964385, -297.6374348207216372, -204.1194202711456569 ) ) ;
#92328 = CARTESIAN_POINT ( 'NONE',  ( 15.17142995382244486, -284.8091770220731860, -216.3168956254932027 ) ) ;
#92330 = CARTESIAN_POINT ( 'NONE',  ( -60.50992131055743073, -285.7598909318557503, -196.8737128612835079 ) ) ;
#92331 = CARTESIAN_POINT ( 'NONE',  ( -37.50580642586700009, -288.7208385459273927, -347.3528673581230919 ) ) ;
#92332 = CARTESIAN_POINT ( 'NONE',  ( -96.10852583545484151, -297.8859912694574632, -317.5500273586097819 ) ) ;
#92333 = CARTESIAN_POINT ( 'NONE',  ( 22.78468102161714981, -292.1613886565898497, -314.9127365726932908 ) ) ;
#92334 = CARTESIAN_POINT ( 'NONE',  ( 15.05870482382987596, -279.9659114116985279, -214.0891177953703561 ) ) ;
#92335 = CARTESIAN_POINT ( 'NONE',  ( -85.28047601435908120, -288.9094976428776818, -210.1954327657594206 ) ) ;
#92336 = CARTESIAN_POINT ( 'NONE',  ( 222.8344101925596590, 7.485601368116228304E-15, -22.08578643762689708 ) ) ;
#92337 = CARTESIAN_POINT ( 'NONE',  ( -42.70818369039324125, -287.9161411897082417, -343.6126213517956671 ) ) ;
#92338 = CARTESIAN_POINT ( 'NONE',  ( -186.9122233887894140, -89.54582641780471874, 22.50000000000000000 ) ) ;
#92339 = CARTESIAN_POINT ( 'NONE',  ( 11.39612404223932351, -286.3767784449806868, -327.4352506789019230 ) ) ;
#92340 = CARTESIAN_POINT ( 'NONE',  ( -68.40260495460989887, -299.2373038247618524, -203.4020963817534096 ) ) ;
#92341 = CARTESIAN_POINT ( 'NONE',  ( -48.05426540342109121, -281.3438325209871778, -194.6515723423923134 ) ) ;
#92343 = CARTESIAN_POINT ( 'NONE',  ( 19.35203898731771233, -282.2030330379161569, -316.3679929442639605 ) ) ;
#92342 = CARTESIAN_POINT ( 'NONE',  ( -111.7611038063295013, -294.7245969887872548, -258.4406608521890121 ) ) ;
#92344 = CARTESIAN_POINT ( 'NONE',  ( -110.8137658269120607, -297.0103271155928155, -247.1440507521128609 ) ) ;
#92345 = CARTESIAN_POINT ( 'NONE',  ( -105.9722901025433828, -274.3310865244872048, -243.6645393570520923 ) ) ;
#92346 = CARTESIAN_POINT ( 'NONE',  ( 15.78786429297873006, -282.8041539373235764, -217.3520389658156660 ) ) ;
#92347 = CARTESIAN_POINT ( 'NONE',  ( -67.17074346553154385, -272.5719656088507463, -203.3813005540561960 ) ) ;
#92348 = ORIENTED_EDGE ( 'NONE', *, *, #84321, .T. ) ;
#92349 = DIRECTION ( 'NONE',  ( -0.000000000000000000, 1.000000000000000000, -9.656854691831248164E-17 ) ) ;
#92350 = CARTESIAN_POINT ( 'NONE',  ( -68.44730547988727665, -285.4427669884234433, -338.2160229043689696 ) ) ;
#92351 = DIRECTION ( 'NONE',  ( -0.000000000000000000, 1.000000000000000000, 0.000000000000000000 ) ) ;
#92352 = CARTESIAN_POINT ( 'NONE',  ( -69.85430415644619018, -289.1237833571632905, -202.7746430608542312 ) ) ;
#92353 = CARTESIAN_POINT ( 'NONE',  ( 19.75035846940255979, -275.4490506322395049, -321.8070212831317463 ) ) ;
#92354 = CARTESIAN_POINT ( 'NONE',  ( 8.850481388264096694, -292.5392735307085559, -213.7687220435549023 ) ) ;
#92355 = CARTESIAN_POINT ( 'NONE',  ( 19.03717703127611927, -283.7402298262488216, -317.8373246556525373 ) ) ;
#92356 = CARTESIAN_POINT ( 'NONE',  ( 35.15560644665041679, -276.9721454594476313, -256.5560118213106193 ) ) ;
#92357 = CARTESIAN_POINT ( 'NONE',  ( -113.3160529357301556, -285.8746459840568264, -278.5161169109562707 ) ) ;
#92358 = CARTESIAN_POINT ( 'NONE',  ( -5.876569458893204256, -281.4240098572850570, -336.6853941419780085 ) ) ;
#92359 = CARTESIAN_POINT ( 'NONE',  ( -105.1897154986274074, -280.9740806400527049, -238.2757403489738977 ) ) ;
#92360 = CARTESIAN_POINT ( 'NONE',  ( 33.71272902355963907, -275.3399628929311689, -240.5541036817906786 ) ) ;
#92361 = CARTESIAN_POINT ( 'NONE',  ( 38.21915848302209184, -275.2001603839090649, -255.5436738548442293 ) ) ;
#92362 = CARTESIAN_POINT ( 'NONE',  ( -34.21674308949055643, -296.9327062603370564, -344.7355009611281957 ) ) ;
#92363 = DIRECTION ( 'NONE',  ( 0.000000000000000000, 0.000000000000000000, 1.000000000000000000 ) ) ;
#92364 = CARTESIAN_POINT ( 'NONE',  ( 151.9232213214486649, 19.99481389066561121, -6.233836834234008251 ) ) ;
#92365 = CARTESIAN_POINT ( 'NONE',  ( -66.47178800654958764, -293.5691398486422941, -340.3160939247162560 ) ) ;
#92366 = CARTESIAN_POINT ( 'NONE',  ( 0.8982964622461634407, -276.0349798733692523, -332.6756102250192839 ) ) ;
#92367 = AXIS2_PLACEMENT_3D ( 'NONE', #66873, #89088, #45529 ) ;
#92368 = CARTESIAN_POINT ( 'NONE',  ( 23.48809492524796738, -295.6915857997874468, -316.4311059189952857 ) ) ;
#92369 = CARTESIAN_POINT ( 'NONE',  ( -4.657948827176248585, -295.8362059009780296, -339.6559675273774133 ) ) ;
#92370 = EDGE_CURVE ( 'NONE', #3752, #15791, #8003, .T. ) ;
#92372 = AXIS2_PLACEMENT_3D ( 'NONE', #37867, #44970, #67708 ) ;
#92371 = CARTESIAN_POINT ( 'NONE',  ( -75.94668771473020286, -293.5358917652927175, -206.1937969760872136 ) ) ;
#92373 = CARTESIAN_POINT ( 'NONE',  ( -99.17774930438719139, -275.9800244522102162, -312.5076652827130488 ) ) ;
#92374 = CARTESIAN_POINT ( 'NONE',  ( -109.6949650857145286, -280.6987555229260352, -252.8591394829081764 ) ) ;
#92375 = CARTESIAN_POINT ( 'NONE',  ( -93.28878772601973424, -293.9446465654510803, -319.4654720558318672 ) ) ;
#92376 = CARTESIAN_POINT ( 'NONE',  ( 31.28380535012820118, -283.8317752433003989, -302.5915855325646930 ) ) ;
#92377 = CARTESIAN_POINT ( 'NONE',  ( -41.32603987864296613, -284.9211706674892639, -197.1478076631026397 ) ) ;
#92378 = CARTESIAN_POINT ( 'NONE',  ( -29.18771587708346615, -125.5003645754393915, -363.4224408895635747 ) ) ;
#92379 = ORIENTED_EDGE ( 'NONE', *, *, #53825, .F. ) ;
#92380 = CARTESIAN_POINT ( 'NONE',  ( -109.6325590332666309, -284.3547228059580902, -260.0597003358899997 ) ) ;
#92381 = ORIENTED_EDGE ( 'NONE', *, *, #9285, .F. ) ;
#92382 = CARTESIAN_POINT ( 'NONE',  ( 32.88435712544961120, -282.2371944979362297, -239.5423997818317048 ) ) ;
#92383 = CARTESIAN_POINT ( 'NONE',  ( -113.9290005361301752, -283.3878749898391334, -267.1158424668637394 ) ) ;
#92384 = CARTESIAN_POINT ( 'NONE',  ( -111.8604135686670560, -279.7253183986641147, -251.8739877468008217 ) ) ;
#92385 = CARTESIAN_POINT ( 'NONE',  ( -92.81651322988420816, -279.3496176672071556, -322.8320783532010410 ) ) ;
#92386 = CARTESIAN_POINT ( 'NONE',  ( -82.18614792566211236, -280.1093904727838435, -207.8928197183208795 ) ) ;
#92387 = CARTESIAN_POINT ( 'NONE',  ( -67.74223827176246004, -274.9809262143061233, -333.4151289067050357 ) ) ;
#92388 = CARTESIAN_POINT ( 'NONE',  ( -98.94016388745465918, -248.7537405824094208, -334.3288800165568659 ) ) ;
#92389 = ORIENTED_EDGE ( 'NONE', *, *, #40510, .T. ) ;
#92390 = CARTESIAN_POINT ( 'NONE',  ( -16.14516622885952657, -276.3268667587246910, -198.5384683514388087 ) ) ;
#92391 = CARTESIAN_POINT ( 'NONE',  ( -64.16662707700760393, -182.5074878589848026, -362.2231175211663299 ) ) ;
#92392 = CARTESIAN_POINT ( 'NONE',  ( -93.42800663272525696, -277.2600484248416137, -221.0854839873903757 ) ) ;
#92393 = CARTESIAN_POINT ( 'NONE',  ( -1.304463679438762069, -294.2836156537364900, -203.4634976634465318 ) ) ;
#92394 = CARTESIAN_POINT ( 'NONE',  ( 18.04424157008249807, -293.5794663659752928, -318.0906837000248402 ) ) ;
#92395 = CARTESIAN_POINT ( 'NONE',  ( -80.51127564382603907, -289.1276099087729108, -334.1115455632428279 ) ) ;
#92396 = DIRECTION ( 'NONE',  ( -1.000000000000000000, 0.000000000000000000, 0.000000000000000000 ) ) ;
#92398 = CARTESIAN_POINT ( 'NONE',  ( -84.13960492805603053, -283.7965362980150985, -213.2298892644596435 ) ) ;
#92397 = CARTESIAN_POINT ( 'NONE',  ( -11.27540808798117844, -293.2939136892524061, -342.2445051051164455 ) ) ;
#92399 = CARTESIAN_POINT ( 'NONE',  ( -70.79826222694117632, -293.4663746965425730, -204.0925437123178483 ) ) ;
#92400 = CARTESIAN_POINT ( 'NONE',  ( -94.51618866481463499, -286.5161646675685461, -224.1641012833078719 ) ) ;
#92401 = EDGE_LOOP ( 'NONE', ( #90762, #36420 ) ) ;
#92402 = CARTESIAN_POINT ( 'NONE',  ( -66.93584214508034336, -292.6148942695525079, -199.5302845020301561 ) ) ;
#92403 = CARTESIAN_POINT ( 'NONE',  ( -56.32885733811063034, -283.7958517097265485, -340.9123497404513046 ) ) ;
#92404 = CARTESIAN_POINT ( 'NONE',  ( -16.62907155743504006, -293.5853953982571056, -344.1656097387794375 ) ) ;
#92405 = CARTESIAN_POINT ( 'NONE',  ( 22.28632056984372056, -289.0067130362657508, -318.8447835755719666 ) ) ;
#92406 = CARTESIAN_POINT ( 'NONE',  ( -51.66769595194030984, -289.7230598291117758, -345.9540590995590605 ) ) ;
#92407 = CARTESIAN_POINT ( 'NONE',  ( 34.56702236190806588, -287.5491843030301879, -257.5008271373959587 ) ) ;
#92408 = ORIENTED_EDGE ( 'NONE', *, *, #28179, .T. ) ;
#92409 = CARTESIAN_POINT ( 'NONE',  ( 208.4306832106271088, -74.55766379199613425, -7.500000000000013323 ) ) ;
#92410 = CARTESIAN_POINT ( 'NONE',  ( -89.83885599784697717, -297.6436107370255399, -325.0625676247297520 ) ) ;
#92411 = CARTESIAN_POINT ( 'NONE',  ( -54.46838210687174353, -296.5213727501273979, -195.7958778514147582 ) ) ;
#92412 = CARTESIAN_POINT ( 'NONE',  ( 2.843076177543889305, -279.6644179167183211, -209.0745134814166590 ) ) ;
#92413 = CARTESIAN_POINT ( 'NONE',  ( -55.31315761928669872, -273.3345801644555877, -195.5510008947174470 ) ) ;
#92414 = CARTESIAN_POINT ( 'NONE',  ( -58.62682165520693189, -293.8123267978988338, -340.9135903176421039 ) ) ;
#92415 = CARTESIAN_POINT ( 'NONE',  ( 33.82829857066034407, -277.0451818656903242, -249.8605770083961772 ) ) ;
#92416 = CARTESIAN_POINT ( 'NONE',  ( -70.01359868815212906, -271.7566574197194313, -203.7021911362464834 ) ) ;
#92417 = CARTESIAN_POINT ( 'NONE',  ( -12.86141856604536571, -295.9319840631955572, -339.6089355899658813 ) ) ;
#92418 = CARTESIAN_POINT ( 'NONE',  ( -35.62966877391741605, -296.1098791767777811, -343.6627862385698791 ) ) ;
#92419 = DIRECTION ( 'NONE',  ( -1.000000000000000000, 0.000000000000000000, 0.000000000000000000 ) ) ;
#92420 = CARTESIAN_POINT ( 'NONE',  ( -6.106797634887838555, -296.2486052104973737, -339.8652278160894866 ) ) ;
#92421 = CARTESIAN_POINT ( 'NONE',  ( -94.21152794698913624, -293.8718696533530306, -319.5124263356717620 ) ) ;
#92422 = CARTESIAN_POINT ( 'NONE',  ( -47.01615458380901202, -292.5774353946418387, -197.9021806525712179 ) ) ;
#92423 = CARTESIAN_POINT ( 'NONE',  ( -49.70335915969832996, -274.7013014873882071, -194.4697808734456430 ) ) ;
#92424 = CARTESIAN_POINT ( 'NONE',  ( -110.2816767919995868, -289.2594485418899239, -260.2301535650274218 ) ) ;
#92425 = CARTESIAN_POINT ( 'NONE',  ( -40.89449690936561410, -276.0077436718352715, -195.3942487085843993 ) ) ;
#92426 = CARTESIAN_POINT ( 'NONE',  ( -114.1200850071242030, -273.1161426097481808, -264.6370713041806653 ) ) ;
#92427 = CARTESIAN_POINT ( 'NONE',  ( -68.06028761040789732, -297.9706619686879208, -204.1020277631467081 ) ) ;
#92428 = CARTESIAN_POINT ( 'NONE',  ( -83.57803754824804798, -281.4018631775118706, -210.7920609206440474 ) ) ;
#92429 = CARTESIAN_POINT ( 'NONE',  ( -2.599025925956609751, -279.1866888084022094, -202.1831143562232285 ) ) ;
#92430 = CARTESIAN_POINT ( 'NONE',  ( -35.72198420555046283, -276.3809561960087535, -347.2552317297560194 ) ) ;
#92431 = CARTESIAN_POINT ( 'NONE',  ( 0.9893635474065419766, -278.9542227553109228, -204.4438417663529890 ) ) ;
#92432 = CARTESIAN_POINT ( 'NONE',  ( 14.47094055627969844, -280.3251422888931756, -324.8173269029031189 ) ) ;
#92433 = CARTESIAN_POINT ( 'NONE',  ( -13.86038227978747805, -272.9376484031900532, -200.6187160415323092 ) ) ;
#92434 = CARTESIAN_POINT ( 'NONE',  ( -96.50257124089317529, -279.9198143362530118, -316.4792577836873875 ) ) ;
#92435 = CYLINDRICAL_SURFACE ( 'NONE', #4990, 4.000000000000003553 ) ;
#92436 = FACE_BOUND ( 'NONE', #39753, .T. ) ;
#92437 = CARTESIAN_POINT ( 'NONE',  ( -72.78770741631151964, -295.8294909808643638, -203.0903015163875409 ) ) ;
#92438 = CARTESIAN_POINT ( 'NONE',  ( 20.07395324843201578, -290.8997583614815312, -221.5372004775421715 ) ) ;
#92439 = VECTOR ( 'NONE', #74049, 1000.000000000000000 ) ;
#92440 = CARTESIAN_POINT ( 'NONE',  ( -42.05396223094423647, -291.9942947593717690, -193.5054442435709916 ) ) ;
#92441 = CARTESIAN_POINT ( 'NONE',  ( 24.57163989498581813, -278.1297590531165724, -313.0747946223415283 ) ) ;
#92442 = CARTESIAN_POINT ( 'NONE',  ( -32.53817334128842731, -272.1125250108581781, -195.5022281464653986 ) ) ;
#92443 = DIRECTION ( 'NONE',  ( -1.000000000000000000, -0.000000000000000000, -0.000000000000000000 ) ) ;
#92444 = CARTESIAN_POINT ( 'NONE',  ( 33.25105002310052527, -283.8199065750541195, -297.3050936023727218 ) ) ;
#92445 = DIRECTION ( 'NONE',  ( -0.000000000000000000, -0.000000000000000000, -1.000000000000000000 ) ) ;
#92446 = CARTESIAN_POINT ( 'NONE',  ( -38.72469510748567956, -284.0346815335708470, -195.3612413815589832 ) ) ;
#92447 = DIRECTION ( 'NONE',  ( 0.000000000000000000, 1.000000000000000000, 0.000000000000000000 ) ) ;
#92448 = CARTESIAN_POINT ( 'NONE',  ( -53.25031351071658747, -294.0555033401352603, -342.0656486522744899 ) ) ;
#92449 = CARTESIAN_POINT ( 'NONE',  ( 36.34751924726685957, -285.8083108793463794, -279.3480210927828011 ) ) ;
#92450 = DIRECTION ( 'NONE',  ( 1.000000000000000000, 0.000000000000000000, 0.000000000000000000 ) ) ;
#92451 = CARTESIAN_POINT ( 'NONE',  ( -20.42106327112575315, -292.8348034784260676, -343.4810037941167025 ) ) ;
#92452 = CARTESIAN_POINT ( 'NONE',  ( -107.2828137259667898, -283.4260554701794490, -239.7176304780192595 ) ) ;
#92453 = CARTESIAN_POINT ( 'NONE',  ( -90.05916104119076238, -280.8923796812117075, -218.6426686473634220 ) ) ;
#92454 = CARTESIAN_POINT ( 'NONE',  ( -67.04930770811191110, -286.8763560446274710, -199.7532800959490373 ) ) ;
#92455 = CARTESIAN_POINT ( 'NONE',  ( 38.26740856491498022, -279.8943142389313721, -278.4334528982410575 ) ) ;
#92456 = CARTESIAN_POINT ( 'NONE',  ( 33.02926598127910296, -287.2956113131820075, -250.9465067622640504 ) ) ;
#92457 = CARTESIAN_POINT ( 'NONE',  ( -101.0842191552740559, -279.4760126265431381, -307.2365895810415282 ) ) ;
#92458 = CARTESIAN_POINT ( 'NONE',  ( -97.77646495367817181, -278.7825651350120779, -311.5950958110067290 ) ) ;
#92459 = CARTESIAN_POINT ( 'NONE',  ( -31.04692836020613100, -288.1111822576340842, -195.2562791383247145 ) ) ;
#92460 = ORIENTED_EDGE ( 'NONE', *, *, #68768, .F. ) ;
#92461 = CARTESIAN_POINT ( 'NONE',  ( 99.18810204040222800, -299.5506171838408136, -193.3647305641561047 ) ) ;
#92462 = CARTESIAN_POINT ( 'NONE',  ( -111.4187789823227774, -292.4135038073661690, -279.5498714609097988 ) ) ;
#92463 = CARTESIAN_POINT ( 'NONE',  ( -111.2869819898779866, -293.4805209788416391, -234.7871824221999191 ) ) ;
#92464 = ORIENTED_EDGE ( 'NONE', *, *, #5711, .T. ) ;
#92465 = CARTESIAN_POINT ( 'NONE',  ( -21.71057506694973682, -272.2519085613607785, -196.8376771436088859 ) ) ;
#92466 = CARTESIAN_POINT ( 'NONE',  ( -110.4536339652047303, -294.6793314764457818, -291.8800870402612304 ) ) ;
#92467 = CARTESIAN_POINT ( 'NONE',  ( 94.55604251903913848, -299.2547878850892289, -197.3111030628182903 ) ) ;
#92468 = CARTESIAN_POINT ( 'NONE',  ( 31.13656435624857721, -289.4347994536315127, -297.7281449038080723 ) ) ;
#92469 = CARTESIAN_POINT ( 'NONE',  ( -7.612708556557906014, -282.2074094431987987, -202.5670169396713902 ) ) ;
#92470 = CARTESIAN_POINT ( 'NONE',  ( -100.1855814773067976, -291.3989491297747918, -313.8266545614586676 ) ) ;
#92471 = CARTESIAN_POINT ( 'NONE',  ( -109.3954133496011849, -291.5387920046486556, -296.2389033494619071 ) ) ;
#92472 = CARTESIAN_POINT ( 'NONE',  ( -37.30477823177420760, -288.0527346064550898, -195.3483429767250925 ) ) ;
#92473 = CARTESIAN_POINT ( 'NONE',  ( -36.75468551780674886, -280.2260185924430402, -193.3503100811241211 ) ) ;
#92474 = CARTESIAN_POINT ( 'NONE',  ( -36.31893663002138339, -293.1193119070928219, -345.9270587204782146 ) ) ;
#92475 = CARTESIAN_POINT ( 'NONE',  ( 29.76085774804294104, -281.8766870924667955, -308.2354617066612832 ) ) ;
#92476 = CARTESIAN_POINT ( 'NONE',  ( 21.83568164135893142, -278.0319096686571925, -315.1819052347053685 ) ) ;
#92477 = EDGE_CURVE ( 'NONE', #58726, #75846, #89337, .T. ) ;
#92478 = CARTESIAN_POINT ( 'NONE',  ( -106.6379572354042296, -298.6233781216988632, -303.7686719486574702 ) ) ;
#92479 = CARTESIAN_POINT ( 'NONE',  ( 9.878578092673036437, -274.6522206064715306, -329.9616376689355661 ) ) ;
#92480 = CARTESIAN_POINT ( 'NONE',  ( 154.6618932926284913, 20.39585521906777643, -12.36951983184901493 ) ) ;
#92481 = CARTESIAN_POINT ( 'NONE',  ( 18.01525293269430250, -280.3811044283108345, -222.6596693763912356 ) ) ;
#92482 = CARTESIAN_POINT ( 'NONE',  ( -111.0542265122078760, -279.4946281539255892, -291.2051140777136311 ) ) ;
#92483 = CARTESIAN_POINT ( 'NONE',  ( -110.3777054418884518, -273.9745742520231033, -262.1766567663059959 ) ) ;
#92484 = CARTESIAN_POINT ( 'NONE',  ( -91.72781268998785720, -284.3583672805116862, -216.1857455974873119 ) ) ;
#92485 = CARTESIAN_POINT ( 'NONE',  ( -99.68339717852953186, -291.7680111256601094, -310.2545613256325510 ) ) ;
#92486 = CARTESIAN_POINT ( 'NONE',  ( -73.58253832576244235, -275.1799639612625583, -203.2722967066240471 ) ) ;
#92487 = CARTESIAN_POINT ( 'NONE',  ( -113.3744484654679496, -273.9743643694620800, -261.8570335280117547 ) ) ;
#92488 = DIRECTION ( 'NONE',  ( -1.000000000000000000, 0.000000000000000000, 0.000000000000000000 ) ) ;
#92489 = CARTESIAN_POINT ( 'NONE',  ( 22.46461596077932299, -275.9702737849684695, -312.3072407396416565 ) ) ;
#92490 = CARTESIAN_POINT ( 'NONE',  ( -111.6211050277696870, -298.4300368581620546, -279.8632869663230167 ) ) ;
#92491 = CARTESIAN_POINT ( 'NONE',  ( -93.96256545681870875, -281.8717741524594658, -319.3102295882197836 ) ) ;
#92492 = CARTESIAN_POINT ( 'NONE',  ( -108.3459963112656084, -290.5971806542126501, -240.6267235045343966 ) ) ;
#92493 = CARTESIAN_POINT ( 'NONE',  ( 34.82610822964737451, -273.8185249060819615, -289.4308385419566889 ) ) ;
#92494 = CARTESIAN_POINT ( 'NONE',  ( 36.01980672278555318, -289.4137326234675811, -291.0131357640676697 ) ) ;
#92495 = CARTESIAN_POINT ( 'NONE',  ( -110.6159212601936872, -289.4258526416617201, -273.9102701976490266 ) ) ;
#92496 = EDGE_LOOP ( 'NONE', ( #66437, #43230, #74966, #36154 ) ) ;
#92497 = CARTESIAN_POINT ( 'NONE',  ( -113.0795934929261648, -289.2592741451185816, -259.8562414806100946 ) ) ;
#92498 = CARTESIAN_POINT ( 'NONE',  ( -92.56970891164738191, -290.8993613513613923, -222.5913102308176690 ) ) ;
#92499 = ORIENTED_EDGE ( 'NONE', *, *, #42244, .F. ) ;
#92500 = CARTESIAN_POINT ( 'NONE',  ( 7.352582380548118302, -287.7250305501481762, -207.9746668260836202 ) ) ;
#92501 = CARTESIAN_POINT ( 'NONE',  ( -67.31884827615527911, -279.9811627624397374, -203.7632894113078805 ) ) ;
#92502 = EDGE_CURVE ( 'NONE', #21926, #84200, #76530, .T. ) ;
#92503 = CARTESIAN_POINT ( 'NONE',  ( -58.77815523803668185, -294.2432934187202704, -344.0505035224324502 ) ) ;
#92504 = CARTESIAN_POINT ( 'NONE',  ( -52.88888448907410123, -283.8976531718593606, -345.7255481955066330 ) ) ;
#92505 = CARTESIAN_POINT ( 'NONE',  ( -64.54369072844005473, -286.0398866648573630, -198.3344827668701100 ) ) ;
#92506 = CARTESIAN_POINT ( 'NONE',  ( -45.63765681737091739, -283.4933357034532833, -342.9604870063594717 ) ) ;
#92507 = CARTESIAN_POINT ( 'NONE',  ( -39.58618975457473255, -139.6688266294182768, -364.8155837051159551 ) ) ;
#92508 = CIRCLE ( 'NONE', #75887, 1.000000000000000888 ) ;
#92509 = CARTESIAN_POINT ( 'NONE',  ( 172.5651499870576231, 243.3239573015568453, -178.9755940783880988 ) ) ;
#92510 = CARTESIAN_POINT ( 'NONE',  ( -102.8603717599729350, -253.7444470676181822, -324.0947072860470826 ) ) ;
#92511 = TOROIDAL_SURFACE ( 'NONE', #35072, 5.603083949679977138, 1.500000000000000000 ) ;
#92512 = CARTESIAN_POINT ( 'NONE',  ( 20.95941956308728038, -275.3690919381396611, -314.5604524820059851 ) ) ;
#92513 = CARTESIAN_POINT ( 'NONE',  ( -32.65760476330481765, -273.0328654814960032, -197.1892240351786256 ) ) ;
#92514 = CARTESIAN_POINT ( 'NONE',  ( -108.3206973038857939, -295.6803290092203156, -300.1892476724093513 ) ) ;
#92515 = CARTESIAN_POINT ( 'NONE',  ( -20.76932496182354271, -109.4398534507196246, -359.3069450751410159 ) ) ;
#92516 = CARTESIAN_POINT ( 'NONE',  ( 25.74745274442921783, -273.6618922733635486, -227.0590612495184928 ) ) ;
#92517 = CARTESIAN_POINT ( 'NONE',  ( -110.4970624660761160, -298.5762250677697693, -257.7453166657177235 ) ) ;
#92518 = CARTESIAN_POINT ( 'NONE',  ( -52.44683329288052676, -292.9339375586183110, -198.5729441275987313 ) ) ;
#92519 = ORIENTED_EDGE ( 'NONE', *, *, #35848, .T. ) ;
#92520 = CARTESIAN_POINT ( 'NONE',  ( -98.05527222062868020, -298.1226551495561807, -223.3645609732990920 ) ) ;
#92521 = VECTOR ( 'NONE', #51453, 1000.000000000000114 ) ;
#92522 = CARTESIAN_POINT ( 'NONE',  ( 33.44662823560920373, -287.8054138151556458, -252.2274694614163195 ) ) ;
#92523 = CARTESIAN_POINT ( 'NONE',  ( -69.45110713615979137, -296.2668742305835963, -340.1834333749815187 ) ) ;
#92524 = CARTESIAN_POINT ( 'NONE',  ( -53.27037787407919467, -295.7433601446153375, -345.6871525281212030 ) ) ;
#92525 = CARTESIAN_POINT ( 'NONE',  ( 18.47521582680869656, -293.0504065899468742, -223.3135686541082805 ) ) ;
#92526 = EDGE_LOOP ( 'NONE', ( #5788, #28170, #18824, #89565 ) ) ;
#92527 = CARTESIAN_POINT ( 'NONE',  ( 29.95645263875353592, -277.0213912549139081, -236.0060189523225347 ) ) ;
#92528 = EDGE_LOOP ( 'NONE', ( #32109, #21138, #25734, #6830 ) ) ;
#92529 = CARTESIAN_POINT ( 'NONE',  ( 21.02351632912151302, -280.3824454693394728, -220.2109681438771247 ) ) ;
#92530 = CARTESIAN_POINT ( 'NONE',  ( -5.215624345412746443, -275.4269267851343557, -204.5344578001107436 ) ) ;
#92531 = CARTESIAN_POINT ( 'NONE',  ( 23.65289900751695740, -276.7016712331484882, -225.0440914682972107 ) ) ;
#92532 = CARTESIAN_POINT ( 'NONE',  ( -92.15527082730963571, -275.8501680888918486, -322.1455895656765165 ) ) ;
#92533 = CARTESIAN_POINT ( 'NONE',  ( -86.17453365271745724, -298.0045697617848646, -215.9621562474705740 ) ) ;
#92534 = CARTESIAN_POINT ( 'NONE',  ( -88.92774287512330034, -294.3687337769426335, -322.9137460969129165 ) ) ;
#92535 = CARTESIAN_POINT ( 'NONE',  ( 152.8567950062365242, 19.85971597382232190, -11.17893457255801337 ) ) ;
#92536 = CARTESIAN_POINT ( 'NONE',  ( -88.89486020009987044, -279.8428512276703373, -213.2489599978644605 ) ) ;
#92537 = CARTESIAN_POINT ( 'NONE',  ( -53.95186679877729574, -277.4379230936123690, -341.4984353207633490 ) ) ;
#92538 = CARTESIAN_POINT ( 'NONE',  ( -35.14550288652753096, -284.7639856951500974, -193.8727361304423482 ) ) ;
#92539 = CARTESIAN_POINT ( 'NONE',  ( -45.94591216823866375, -299.9434374326102102, -195.6885262199777173 ) ) ;
#92540 = DIRECTION ( 'NONE',  ( 1.000000000000000000, 0.000000000000000000, -0.000000000000000000 ) ) ;
#92541 = CARTESIAN_POINT ( 'NONE',  ( 33.18765048848243282, -286.4929084700483486, -250.9134335727029566 ) ) ;
#92542 = CARTESIAN_POINT ( 'NONE',  ( -1.455390797629685151, -278.7747988070152019, -205.6297745915796327 ) ) ;
#92544 = CARTESIAN_POINT ( 'NONE',  ( -97.09191659137582064, -282.0213189636901348, -314.7596070663852288 ) ) ;
#92543 = CARTESIAN_POINT ( 'NONE',  ( -92.63930732343847296, -277.8145787173258441, -221.7873507051324111 ) ) ;
#92545 = CARTESIAN_POINT ( 'NONE',  ( -1.595886038607218005, -288.5257171740798867, -204.3704180865621254 ) ) ;
#92546 = CARTESIAN_POINT ( 'NONE',  ( -3.671716595751149725, -277.8025039403691494, -335.5796944374403097 ) ) ;
#92547 = CARTESIAN_POINT ( 'NONE',  ( 113.5000000000000568, -218.8335761803644743, -447.4016117689005796 ) ) ;
#92548 = CARTESIAN_POINT ( 'NONE',  ( -100.0267504248804613, -293.1090998541118893, -229.0903940957017255 ) ) ;
#92549 = CARTESIAN_POINT ( 'NONE',  ( -81.96948824083577279, -275.8910997205643980, -331.8618052930501108 ) ) ;
#92550 = CARTESIAN_POINT ( 'NONE',  ( 33.60610856450742290, -275.9714382879130312, -252.7457522400398204 ) ) ;
#92551 = CARTESIAN_POINT ( 'NONE',  ( 30.35889149930225983, -283.1217076853852177, -237.5817215595189396 ) ) ;
#92552 = CARTESIAN_POINT ( 'NONE',  ( 115.2448031289451222, -296.6656502513747569, -195.3611179825600175 ) ) ;
#92553 = CARTESIAN_POINT ( 'NONE',  ( 37.25736755183265103, -289.6294585688051484, -282.6920613661519610 ) ) ;
#92554 = CARTESIAN_POINT ( 'NONE',  ( -39.59235620295065416, -293.0802274217718377, -345.3399974340590006 ) ) ;
#92555 = CARTESIAN_POINT ( 'NONE',  ( 207.7524637998687638, 30.27509731313811869, 14.39153753875996244 ) ) ;
#92556 = CARTESIAN_POINT ( 'NONE',  ( -59.60922381712671836, -272.4425950688236071, -200.2692765529102132 ) ) ;
#92557 = CARTESIAN_POINT ( 'NONE',  ( 25.91257362791393604, -291.1639128296090462, -231.4078223145774587 ) ) ;
#92558 = CARTESIAN_POINT ( 'NONE',  ( 185.2614386149834900, 255.8498544563436212, -168.8850006258623466 ) ) ;
#92559 = PLANE ( 'NONE',  #92793 ) ;
#92560 = CARTESIAN_POINT ( 'NONE',  ( -40.33115375556467086, -287.5689444528201193, -346.6221696820359170 ) ) ;
#92561 = CARTESIAN_POINT ( 'NONE',  ( -108.8635532650809381, -285.9147292358250638, -288.5563080322319820 ) ) ;
#92562 = CARTESIAN_POINT ( 'NONE',  ( 34.11183131551798198, -286.1246203789885385, -296.3668695348035271 ) ) ;
#92563 = CARTESIAN_POINT ( 'NONE',  ( -109.5103547139871267, -286.1657300977041700, -255.9715309889180048 ) ) ;
#92564 = CARTESIAN_POINT ( 'NONE',  ( -106.6886409418972761, -285.6658981906218742, -246.8871124019647141 ) ) ;
#92565 = CARTESIAN_POINT ( 'NONE',  ( -36.42427561246834244, -294.0434887318140795, -194.9987451145523494 ) ) ;
#92566 = CARTESIAN_POINT ( 'NONE',  ( 38.19202618707399211, -273.6066014436967180, -268.3685356935095001 ) ) ;
#92567 = CIRCLE ( 'NONE', #63899, 12.40608546931776957 ) ;
#92568 = CARTESIAN_POINT ( 'NONE',  ( 21.71713412213653882, -276.5500505333026808, -319.7351839345006397 ) ) ;
#92569 = AXIS2_PLACEMENT_3D ( 'NONE', #23055, #51933, #80823 ) ;
#92570 = CARTESIAN_POINT ( 'NONE',  ( -87.67176597078768907, -289.4354698685853009, -214.0033441812990986 ) ) ;
#92571 = CARTESIAN_POINT ( 'NONE',  ( -2.725110648043647110, -276.6072517076405006, -339.1558201891682529 ) ) ;
#92572 = CARTESIAN_POINT ( 'NONE',  ( -111.3707607570620439, -298.6605334229448090, -260.4017289942382263 ) ) ;
#92573 = DIRECTION ( 'NONE',  ( -0.000000000000000000, -0.000000000000000000, 1.000000000000000000 ) ) ;
#92574 = DIRECTION ( 'NONE',  ( -0.000000000000000000, -0.000000000000000000, -1.000000000000000000 ) ) ;
#92575 = CARTESIAN_POINT ( 'NONE',  ( -109.1431343510291185, -283.4431751508562911, -254.6244932806141605 ) ) ;
#92576 = AXIS2_PLACEMENT_3D ( 'NONE', #86280, #85820, #49838 ) ;
#92577 = CARTESIAN_POINT ( 'NONE',  ( -33.97878292851464721, -278.0943049767492994, -195.4365463201227726 ) ) ;
#92578 = CARTESIAN_POINT ( 'NONE',  ( 175.2296996224750103, 154.6894116713782807, -24.16304133878946558 ) ) ;
#92579 = CARTESIAN_POINT ( 'NONE',  ( 21.33028221965052751, -273.3699046859019859, -221.5727357356213076 ) ) ;
#92580 = CARTESIAN_POINT ( 'NONE',  ( -95.35897416353009248, -277.2759307164053553, -314.8345772815358714 ) ) ;
#92581 = VECTOR ( 'NONE', #2905, 1000.000000000000000 ) ;
#92582 = CARTESIAN_POINT ( 'NONE',  ( -38.33237814269151755, -296.5849167835328899, -344.0477946042022950 ) ) ;
#92583 = CARTESIAN_POINT ( 'NONE',  ( 38.49119835734698825, -280.3245098778544389, -258.5767065696824716 ) ) ;
#92584 = CARTESIAN_POINT ( 'NONE',  ( -72.22613468238559165, -296.4668535342543692, -334.7686355178615827 ) ) ;
#92585 = CARTESIAN_POINT ( 'NONE',  ( -110.3242968023328530, -297.5765356712250309, -293.3579071742995552 ) ) ;
#92586 = CARTESIAN_POINT ( 'NONE',  ( -77.51020470942363261, -297.3301747459440207, -209.3455464253848959 ) ) ;
#92587 = CARTESIAN_POINT ( 'NONE',  ( -30.65330466139904075, -294.1368928967606848, -195.6599398481674257 ) ) ;
#92588 = CARTESIAN_POINT ( 'NONE',  ( -9.995946222698144368, -286.5660639713516389, -198.3236971908257544 ) ) ;
#92589 = CARTESIAN_POINT ( 'NONE',  ( -49.49733294339457501, -272.0384817288738759, -195.5248500825431677 ) ) ;
#92590 = CARTESIAN_POINT ( 'NONE',  ( -37.98031595921003856, -285.8776791959257935, -193.3637662465722258 ) ) ;
#92591 = CARTESIAN_POINT ( 'NONE',  ( -27.36290517942728684, -282.1593308363171104, -196.3339794954778199 ) ) ;
#92592 = EDGE_CURVE ( 'NONE', #20083, #87746, #76096, .T. ) ;
#92593 = CARTESIAN_POINT ( 'NONE',  ( -73.66194086058604285, -284.6161423653227871, -206.7521696973063570 ) ) ;
#92594 = CARTESIAN_POINT ( 'NONE',  ( -59.46233846113180732, -287.3384259614666121, -342.0247629238015747 ) ) ;
#92595 = CARTESIAN_POINT ( 'NONE',  ( 185.7741171649701926, 251.7621132184994508, -165.9827577097485118 ) ) ;
#92596 = CARTESIAN_POINT ( 'NONE',  ( 19.56707197325058445, -286.4123357593953187, -224.5223012479260944 ) ) ;
#92597 = CARTESIAN_POINT ( 'NONE',  ( 11.35262850330516926, -283.3376542625996990, -329.7736788346502976 ) ) ;
#92598 = CARTESIAN_POINT ( 'NONE',  ( -110.2037608184899398, -289.9178898456356706, -246.0299938682769607 ) ) ;
#92599 = CARTESIAN_POINT ( 'NONE',  ( -70.90081936161800513, -281.2168859418254101, -201.9489411800058178 ) ) ;
#92600 = CARTESIAN_POINT ( 'NONE',  ( -96.44720905804928179, -280.5242289289388395, -221.7625866177410785 ) ) ;
#92601 = CARTESIAN_POINT ( 'NONE',  ( 34.23025929059489414, -281.5758460622283224, -284.7925453191211886 ) ) ;
#92602 = CARTESIAN_POINT ( 'NONE',  ( 10.74849234607196102, -276.7166477329472514, -212.7402473473817963 ) ) ;
#92603 = CARTESIAN_POINT ( 'NONE',  ( -27.74783466667040344, -294.9336544129975550, -346.8143956828052410 ) ) ;
#92604 = CARTESIAN_POINT ( 'NONE',  ( -107.5888038298831333, -288.2434894918519603, -295.6037648891197591 ) ) ;
#92605 = CARTESIAN_POINT ( 'NONE',  ( -93.84304463315147871, -296.1320722921035440, -223.6315930993400514 ) ) ;
#92606 = ORIENTED_EDGE ( 'NONE', *, *, #68122, .F. ) ;
#92607 = ORIENTED_EDGE ( 'NONE', *, *, #58963, .T. ) ;
#92608 = CARTESIAN_POINT ( 'NONE',  ( 26.81223256635550811, -283.9820507180563709, -308.2199796537997258 ) ) ;
#92609 = CARTESIAN_POINT ( 'NONE',  ( -96.42802146085365678, -295.6183382412937704, -313.2881037232178869 ) ) ;
#92610 = CARTESIAN_POINT ( 'NONE',  ( 34.16958999451200896, -294.2777507999552995, -242.5083317978782134 ) ) ;
#92611 = CARTESIAN_POINT ( 'NONE',  ( 5.658734947701425710, -283.1033929054121927, -329.4784187595963658 ) ) ;
#92612 = EDGE_CURVE ( 'NONE', #47975, #33034, #54768, .T. ) ;
#92613 = CARTESIAN_POINT ( 'NONE',  ( 25.95735759923632457, -274.0357539459441796, -226.9091428178749652 ) ) ;
#92614 = CARTESIAN_POINT ( 'NONE',  ( -98.07399181643657471, -290.5727831894181463, -317.5299798870772179 ) ) ;
#92615 = CARTESIAN_POINT ( 'NONE',  ( -93.49979086451075716, -281.9894643474612508, -321.2387422337883436 ) ) ;
#92616 = CARTESIAN_POINT ( 'NONE',  ( -108.7772606237062263, -290.5213165391426742, -299.0439523635328101 ) ) ;
#92617 = CARTESIAN_POINT ( 'NONE',  ( 5.860550149236601669, -288.7817084345722947, -329.2939333119965113 ) ) ;
#92618 = DIRECTION ( 'NONE',  ( -0.9531768234071978929, 0.3024135303179465439, 0.000000000000000000 ) ) ;
#92619 = FACE_OUTER_BOUND ( 'NONE', #8916, .T. ) ;
#92620 = CARTESIAN_POINT ( 'NONE',  ( 200.9980625852972764, 289.9378660408568749, -82.33773636192533729 ) ) ;
#92621 = CARTESIAN_POINT ( 'NONE',  ( -110.4542110544635705, -288.2666405000204577, -253.6410175316879361 ) ) ;
#92622 = ORIENTED_EDGE ( 'NONE', *, *, #19812, .F. ) ;
#92623 = CARTESIAN_POINT ( 'NONE',  ( -92.43168022879876844, -278.1601237746265269, -221.9755070720262040 ) ) ;
#92624 = CARTESIAN_POINT ( 'NONE',  ( 16.01543713708688799, -274.4508111130603538, -214.8745412785359576 ) ) ;
#92625 = CARTESIAN_POINT ( 'NONE',  ( -112.2264314465326009, -280.5483375777556034, -270.6704305942496376 ) ) ;
#92626 = CARTESIAN_POINT ( 'NONE',  ( 155.2251193104848710, 204.5823050655612860, -215.4134129893866998 ) ) ;
#92627 = CARTESIAN_POINT ( 'NONE',  ( 38.59930615872821136, -280.0144127159293248, -261.4369446313376670 ) ) ;
#92628 = CARTESIAN_POINT ( 'NONE',  ( -72.19880938486630839, -281.5357693747013172, -336.3673960131706053 ) ) ;
#92629 = CARTESIAN_POINT ( 'NONE',  ( -95.71834651478569356, -297.6490401164263062, -319.0243394009386293 ) ) ;
#92630 = CARTESIAN_POINT ( 'NONE',  ( 31.60020728302153614, -294.3678309350707991, -294.6994515822245262 ) ) ;
#92631 = VERTEX_POINT ( 'NONE', #25427 ) ;
#92632 = CARTESIAN_POINT ( 'NONE',  ( -82.01562743920962362, -290.1137337338688553, -211.9402093550817483 ) ) ;
#92633 = CARTESIAN_POINT ( 'NONE',  ( 13.89037694804752121, -275.3997153851897224, -212.9437639542252043 ) ) ;
#92634 = CARTESIAN_POINT ( 'NONE',  ( -64.56878677730624361, -273.6865639375479873, -202.6151809828252226 ) ) ;
#92635 = EDGE_LOOP ( 'NONE', ( #20192, #1706, #51946, #44394 ) ) ;
#92636 = DIRECTION ( 'NONE',  ( -0.6056179655966478226, 0.7957555401921982963, 0.000000000000000000 ) ) ;
#92637 = CARTESIAN_POINT ( 'NONE',  ( 197.2558782386354892, 42.34377483820648536, 11.92135876141209394 ) ) ;
#92638 = EDGE_CURVE ( 'NONE', #24966, #36396, #11690, .T. ) ;
#92639 = VECTOR ( 'NONE', #63722, 1000.000000000000000 ) ;
#92640 = DIRECTION ( 'NONE',  ( -0.000000000000000000, -0.000000000000000000, -1.000000000000000000 ) ) ;
#92641 = AXIS2_PLACEMENT_3D ( 'NONE', #63114, #19520, #20476 ) ;
#92642 = CARTESIAN_POINT ( 'NONE',  ( 15.47257245861199237, -281.9001003777036090, -219.4469127431976574 ) ) ;
#92643 = CARTESIAN_POINT ( 'NONE',  ( -95.14968307826980265, -280.9864978662519661, -221.0236730041305862 ) ) ;
#92644 = CARTESIAN_POINT ( 'NONE',  ( -109.7328037496047131, -283.4608186238167491, -281.7744903052087579 ) ) ;
#92645 = CARTESIAN_POINT ( 'NONE',  ( 18.88484054146146462, -282.7334872640489039, -221.8705737250467962 ) ) ;
#92646 = CARTESIAN_POINT ( 'NONE',  ( 36.04268951173919788, -274.1201099776182559, -277.1019716827017874 ) ) ;
#92648 = DIRECTION ( 'NONE',  ( 0.000000000000000000, -1.000000000000000000, -0.000000000000000000 ) ) ;
#92647 = VECTOR ( 'NONE', #36568, 1000.000000000000000 ) ;
#92649 = DIRECTION ( 'NONE',  ( 0.000000000000000000, 0.000000000000000000, -1.000000000000000000 ) ) ;
#92650 = VECTOR ( 'NONE', #86010, 1000.000000000000000 ) ;
#92651 = CARTESIAN_POINT ( 'NONE',  ( -67.63551481766778295, -278.2424812026052905, -340.9758729023049568 ) ) ;
#92652 = ORIENTED_EDGE ( 'NONE', *, *, #64250, .T. ) ;
#92653 = ORIENTED_EDGE ( 'NONE', *, *, #54065, .F. ) ;
#92654 = CYLINDRICAL_SURFACE ( 'NONE', #3565, 4.000000000000003553 ) ;
#92655 = CARTESIAN_POINT ( 'NONE',  ( -112.2657325385600586, -286.4291764931783746, -278.4107247322160106 ) ) ;
#92656 = CARTESIAN_POINT ( 'NONE',  ( 20.31645664254551775, -292.1157217921819438, -225.3059721731350464 ) ) ;
#92657 = CARTESIAN_POINT ( 'NONE',  ( 39.60034901838157140, -286.9157285095449765, -271.5579925626856266 ) ) ;
#92658 = CARTESIAN_POINT ( 'NONE',  ( -72.84061110800165295, -283.8150037965478987, -205.4021040435784471 ) ) ;
#92660 = CARTESIAN_POINT ( 'NONE',  ( 24.34180251449186727, -286.3521244846036780, -311.2880405816613347 ) ) ;
#92659 = CARTESIAN_POINT ( 'NONE',  ( -93.69471392446111224, -283.7935980199576989, -223.0355143973431495 ) ) ;
#92661 = CARTESIAN_POINT ( 'NONE',  ( 35.74624249197428583, -282.6619248833271172, -263.0968682974351509 ) ) ;
#92662 = CARTESIAN_POINT ( 'NONE',  ( 10.52924183781424716, -272.7126596815619450, -212.5582384100262914 ) ) ;
#92663 = CARTESIAN_POINT ( 'NONE',  ( -111.5757103880138459, -283.1693687970175688, -253.1636722546211615 ) ) ;
#92664 = CARTESIAN_POINT ( 'NONE',  ( -56.89354169956914831, -299.8003121456598592, -197.9005983948055416 ) ) ;
#92665 = CARTESIAN_POINT ( 'NONE',  ( -79.87921786420695014, -283.4785847636560447, -208.3258274069511060 ) ) ;
#92666 = CARTESIAN_POINT ( 'NONE',  ( -81.43908271641872432, -280.3770999615201731, -211.8266766385823132 ) ) ;
#92667 = CARTESIAN_POINT ( 'NONE',  ( 34.09843068951497713, -289.2491378171986867, -246.8209998709012609 ) ) ;
#92668 = DIRECTION ( 'NONE',  ( 0.2916739763039743472, 0.000000000000000000, 0.9565177946839404921 ) ) ;
#92669 = CARTESIAN_POINT ( 'NONE',  ( 175.2296996224750103, 275.0000000000000568, 24.00000000000000355 ) ) ;
#92670 = CARTESIAN_POINT ( 'NONE',  ( 10.19353815006491715, -294.6215679275500179, -211.5595428712367720 ) ) ;
#92671 = CIRCLE ( 'NONE', #6524, 3.842139515347647638 ) ;
#92672 = VECTOR ( 'NONE', #68259, 1000.000000000000000 ) ;
#92673 = CARTESIAN_POINT ( 'NONE',  ( -108.1609338607598403, -276.2304972267014591, -295.2096012446178861 ) ) ;
#92674 = CARTESIAN_POINT ( 'NONE',  ( -113.8450395044615959, -289.8460501988727174, -262.6429917538795848 ) ) ;
#92675 = CARTESIAN_POINT ( 'NONE',  ( -68.87749863574900644, -293.8736536370661270, -337.0978145567249271 ) ) ;
#92676 = CARTESIAN_POINT ( 'NONE',  ( -92.56802169174439143, -277.9246592105881746, -221.8518060719377161 ) ) ;
#92677 = CARTESIAN_POINT ( 'NONE',  ( -34.39520772895804868, -296.2290015565217232, -196.1268563079971727 ) ) ;
#92678 = CARTESIAN_POINT ( 'NONE',  ( -57.80822982711061542, -293.0975594957903354, -199.7220131558359242 ) ) ;
#92679 = CARTESIAN_POINT ( 'NONE',  ( -95.95921662488163406, -286.4090924074130839, -317.1477375740089997 ) ) ;
#92680 = CARTESIAN_POINT ( 'NONE',  ( -112.7017298340046381, -295.1842929837864631, -258.2962494915011575 ) ) ;
#92681 = CARTESIAN_POINT ( 'NONE',  ( 20.14938420122146923, -289.7993748913999070, -316.6343893207871929 ) ) ;
#92682 = CARTESIAN_POINT ( 'NONE',  ( -61.34692068096671846, -289.9845997026833402, -198.2104676535045371 ) ) ;
#92683 = ADVANCED_FACE ( 'NONE', ( #75165 ), #46721, .F. ) ;
#92684 = CARTESIAN_POINT ( 'NONE',  ( -107.9658625752614114, -292.2493396486327129, -249.6377814691441301 ) ) ;
#92685 = CARTESIAN_POINT ( 'NONE',  ( 197.1513938986460062, -147.7221692137691775, 1.978481845683761620 ) ) ;
#92686 = CARTESIAN_POINT ( 'NONE',  ( -20.04387780123211371, -293.0828868104173921, -199.2215553212956536 ) ) ;
#92687 = CARTESIAN_POINT ( 'NONE',  ( 219.8344101925596021, 35.72494958537217968, -10.00000000000000000 ) ) ;
#92688 = CARTESIAN_POINT ( 'NONE',  ( -106.9063117174093378, -292.1710781583050220, -238.1601826525033516 ) ) ;
#92690 = CARTESIAN_POINT ( 'NONE',  ( -25.40909225615754252, -292.2083475194318112, -198.2914966976853464 ) ) ;
#92689 = CARTESIAN_POINT ( 'NONE',  ( 37.77418962071515551, -279.4955715038523749, -264.3602923769542485 ) ) ;
#92691 = CARTESIAN_POINT ( 'NONE',  ( -16.99199079425166303, -280.3078913178703715, -196.0988171157767113 ) ) ;
#92692 = CARTESIAN_POINT ( 'NONE',  ( 13.66360259252715359, -282.0274083300692496, -328.0879720463673266 ) ) ;
#92693 = CARTESIAN_POINT ( 'NONE',  ( 30.01301615046398652, -285.9869643770724110, -303.3511595203857496 ) ) ;
#92694 = CARTESIAN_POINT ( 'NONE',  ( 32.50892429892402902, -280.0226914016827777, -295.6477215796933251 ) ) ;
#92695 = CARTESIAN_POINT ( 'NONE',  ( -65.11249984092846432, -283.6891656544832472, -200.6782345273111332 ) ) ;
#92696 = PLANE ( 'NONE',  #60832 ) ;
#92697 = CARTESIAN_POINT ( 'NONE',  ( -61.80684417870997294, -278.2198669557403150, -198.0270152615564712 ) ) ;
#92698 = CARTESIAN_POINT ( 'NONE',  ( 11.88971723974640682, -285.6377477441452015, -211.4890898157504751 ) ) ;
#92699 = CARTESIAN_POINT ( 'NONE',  ( 23.18017701616185278, -275.7843138273685213, -229.2326404529472939 ) ) ;
#92700 = CARTESIAN_POINT ( 'NONE',  ( 195.0937532148314233, 39.77461757279066035, 15.17963093583605705 ) ) ;
#92701 = CARTESIAN_POINT ( 'NONE',  ( 21.62081414357954756, -294.5357465397808596, -225.9779868656659119 ) ) ;
#92702 = CARTESIAN_POINT ( 'NONE',  ( 11.39579676911217554, -276.1375412612125047, -211.4428845380559778 ) ) ;
#92703 = CARTESIAN_POINT ( 'NONE',  ( -68.05017661106406024, -277.1335245801039378, -336.6249791158144262 ) ) ;
#92704 = CARTESIAN_POINT ( 'NONE',  ( -114.1879726621797317, -290.7796524376174716, -265.4979500743418157 ) ) ;
#92705 = CONICAL_SURFACE ( 'NONE', #30741, 2.888540232138026020, 0.09862129276974965220 ) ;
#92706 = CARTESIAN_POINT ( 'NONE',  ( 0.6710972074730073844, -278.6342487142701998, -204.9996133326930590 ) ) ;
#92707 = CARTESIAN_POINT ( 'NONE',  ( -69.10885461959507836, -290.6825606475176755, -204.3604820173550252 ) ) ;
#92708 = ADVANCED_FACE ( 'NONE', ( #11229 ), #69000, .F. ) ;
#92709 = AXIS2_PLACEMENT_3D ( 'NONE', #41783, #59160, #8019 ) ;
#92710 = CARTESIAN_POINT ( 'NONE',  ( -25.25587232342336819, -292.8980477486874747, -344.4335943646663623 ) ) ;
#92711 = VERTEX_POINT ( 'NONE', #24978 ) ;
#92712 = CARTESIAN_POINT ( 'NONE',  ( 153.4245301327627828, 19.61868323047014329, 10.85241966622267462 ) ) ;
#92713 = AXIS2_PLACEMENT_3D ( 'NONE', #7537, #71495, #49234 ) ;
#92714 = CARTESIAN_POINT ( 'NONE',  ( 4.544050151169820140, -292.1418306738939350, -210.4361500949838160 ) ) ;
#92715 = CARTESIAN_POINT ( 'NONE',  ( 208.9486937585552937, 28.83547737520457588, 12.90287354992395130 ) ) ;
#92716 = CARTESIAN_POINT ( 'NONE',  ( 34.45848030099739390, -273.0523547857346784, -270.3937649182068412 ) ) ;
#92717 = CARTESIAN_POINT ( 'NONE',  ( -113.7103600977389561, -295.5132081979551231, -278.1487997306520015 ) ) ;
#92718 = CARTESIAN_POINT ( 'NONE',  ( -92.06920271828326463, -285.1291852741715616, -323.8232422630305791 ) ) ;
#92719 = CARTESIAN_POINT ( 'NONE',  ( 35.55278243395914473, -287.3225164958134314, -265.5888179833442564 ) ) ;
#92720 = CARTESIAN_POINT ( 'NONE',  ( 34.50543289770274669, -276.8574090467004680, -253.9127791127628768 ) ) ;
#92721 = CARTESIAN_POINT ( 'NONE',  ( -111.3640211395889139, -294.7013876501425784, -260.3517381561532034 ) ) ;
#92722 = CARTESIAN_POINT ( 'NONE',  ( -111.3885459438542824, -298.3334891209181592, -268.7326610350772853 ) ) ;
#92723 = CARTESIAN_POINT ( 'NONE',  ( 28.37925123826012808, -274.7891584195456858, -303.1541860474146688 ) ) ;
#92724 = VERTEX_POINT ( 'NONE', #82259 ) ;
#92725 = CARTESIAN_POINT ( 'NONE',  ( -111.6005434785387536, -296.4752008878752463, -249.8819710408546939 ) ) ;
#92726 = CARTESIAN_POINT ( 'NONE',  ( 4.442736434292411829, -290.4042467313579436, -332.0299016112302866 ) ) ;
#92727 = CARTESIAN_POINT ( 'NONE',  ( -28.85729229363806780, -296.1582027931529524, -195.3640018882764195 ) ) ;
#92728 = AXIS2_PLACEMENT_3D ( 'NONE', #17696, #74995, #24314 ) ;
#92729 = CARTESIAN_POINT ( 'NONE',  ( -34.56583242676096290, -289.6679083174312268, -343.4599794784073197 ) ) ;
#92730 = EDGE_LOOP ( 'NONE', ( #13007, #13694, #93221, #6741, #55252, #37792, #88671, #84151, #63232, #50830, #25401, #24696, #30771, #150, #83305, #882, #82552, #56914, #42894, #80491, #60297, #78430, #12915, #68093, #78229 ) ) ;
#92731 = CARTESIAN_POINT ( 'NONE',  ( -3.749715823618728461, -279.5433076938443833, -201.3220181983409418 ) ) ;
#92732 = CARTESIAN_POINT ( 'NONE',  ( -95.49945937741655655, -297.8847213535917717, -219.9727116720819993 ) ) ;
#92733 = CARTESIAN_POINT ( 'NONE',  ( -109.6109264662099463, -288.3992524881264785, -293.2805329165127546 ) ) ;
#92734 = CARTESIAN_POINT ( 'NONE',  ( -112.2842387552876176, -296.6646875703952446, -288.0067575520780565 ) ) ;
#92735 = CARTESIAN_POINT ( 'NONE',  ( 21.00813975319014659, -293.2691042099392575, -226.4591399783664372 ) ) ;
#92736 = CARTESIAN_POINT ( 'NONE',  ( 198.3166830480494411, 65.26573560487175030, -9.728010558291394716 ) ) ;
#92737 = AXIS2_PLACEMENT_3D ( 'NONE', #459, #28416, #63486 ) ;
#92738 = DIRECTION ( 'NONE',  ( 0.000000000000000000, 0.000000000000000000, -1.000000000000000000 ) ) ;
#92739 = PLANE ( 'NONE',  #89960 ) ;
#92740 = CARTESIAN_POINT ( 'NONE',  ( 35.72713028738823482, -289.3513168716552855, -292.3986689058187380 ) ) ;
#92741 = CARTESIAN_POINT ( 'NONE',  ( -19.11405058567862625, -276.7662352645559167, -190.3538533559490702 ) ) ;
#92742 = ORIENTED_EDGE ( 'NONE', *, *, #71254, .F. ) ;
#92743 = CARTESIAN_POINT ( 'NONE',  ( 35.23424366332909585, -280.5779367435727636, -244.7846100892792265 ) ) ;
#92744 = CARTESIAN_POINT ( 'NONE',  ( -93.01229214289865865, -285.8538830925358525, -320.3885274131033043 ) ) ;
#92745 = CARTESIAN_POINT ( 'NONE',  ( 39.05135671310836898, -286.1061451333618493, -268.7157737124992423 ) ) ;
#92746 = CARTESIAN_POINT ( 'NONE',  ( -79.00013505429254224, -287.6980962825746246, -332.1150732710872830 ) ) ;
#92747 = CARTESIAN_POINT ( 'NONE',  ( 34.55025634783915933, -277.1047257664152994, -246.2824693394957194 ) ) ;
#92748 = VECTOR ( 'NONE', #51144, 1000.000000000000000 ) ;
#92750 = ORIENTED_EDGE ( 'NONE', *, *, #6869, .T. ) ;
#92749 = EDGE_CURVE ( 'NONE', #93680, #8064, #992, .T. ) ;
#92752 = CARTESIAN_POINT ( 'NONE',  ( -39.69621630988346084, -279.3704233127705265, -197.2845749876478578 ) ) ;
#92751 = CARTESIAN_POINT ( 'NONE',  ( -97.64882855119962812, -277.9798621266210148, -311.4956565281365215 ) ) ;
#92753 = CARTESIAN_POINT ( 'NONE',  ( 31.58353368740714373, -277.0666814910394464, -304.1095602022843423 ) ) ;
#92754 = CARTESIAN_POINT ( 'NONE',  ( -104.4383647096886705, -277.8282942715412673, -233.4010541350342862 ) ) ;
#92755 = CARTESIAN_POINT ( 'NONE',  ( -104.2745392939568347, -253.7788420816588371, -324.7530620101808836 ) ) ;
#92756 = CARTESIAN_POINT ( 'NONE',  ( -78.72482614818748914, -274.4503635723456227, -205.7062102539960051 ) ) ;
#92757 = EDGE_CURVE ( 'NONE', #77857, #16264, #84081, .T. ) ;
#92758 = CARTESIAN_POINT ( 'NONE',  ( 75.28772777193687205, -300.8615142928297246, -193.9236106809661919 ) ) ;
#92759 = CARTESIAN_POINT ( 'NONE',  ( -4.829096099716510437, -288.9805209788416391, -202.7746430608542312 ) ) ;
#92760 = CARTESIAN_POINT ( 'NONE',  ( 82.61715650332634198, -302.0474575487106677, -194.9843264058633849 ) ) ;
#92761 = CARTESIAN_POINT ( 'NONE',  ( 26.63043373960363525, -288.1429156043636794, -234.4551642000964478 ) ) ;
#92762 = CARTESIAN_POINT ( 'NONE',  ( -112.4887677409936373, -286.4594547617298304, -258.7488280938900971 ) ) ;
#92763 = CARTESIAN_POINT ( 'NONE',  ( 31.93984256809328315, -286.5913410514270367, -247.0381569831579043 ) ) ;
#92764 = CARTESIAN_POINT ( 'NONE',  ( -111.8169800973878978, -283.8173155669605876, -289.7255276703332356 ) ) ;
#92765 = CARTESIAN_POINT ( 'NONE',  ( 7.645952984501175997, -279.0773445473428183, -211.7938697157454726 ) ) ;
#92766 = CARTESIAN_POINT ( 'NONE',  ( -35.93339486472894606, -287.9304181423797786, -196.1392737618143087 ) ) ;
#92767 = CARTESIAN_POINT ( 'NONE',  ( 15.77240783317803619, -279.3007262354486215, -219.2039608641025268 ) ) ;
#92768 = CARTESIAN_POINT ( 'NONE',  ( -69.45185937936612675, -278.7989468334097296, -336.4823929597917527 ) ) ;
#92769 = CARTESIAN_POINT ( 'NONE',  ( -4.082266448267762193, -274.9953844965841654, -205.2947985567448370 ) ) ;
#92770 = CARTESIAN_POINT ( 'NONE',  ( -67.90959968146094639, -288.2395223493836056, -340.6007950629511356 ) ) ;
#92771 = CARTESIAN_POINT ( 'NONE',  ( 15.64958087279715038, -283.1276838130997362, -326.0035744167684584 ) ) ;
#92772 = CARTESIAN_POINT ( 'NONE',  ( -109.9212842186116319, -285.3668021540639188, -244.8320977037900548 ) ) ;
#92773 = CARTESIAN_POINT ( 'NONE',  ( 18.49572707474300159, -282.3870067893979581, -317.4037272379866863 ) ) ;
#92774 = ORIENTED_EDGE ( 'NONE', *, *, #75186, .T. ) ;
#92775 = ORIENTED_EDGE ( 'NONE', *, *, #28532, .F. ) ;
#92776 = CARTESIAN_POINT ( 'NONE',  ( 186.2362647323748206, 250.0000000000000568, 22.80382896336985965 ) ) ;
#92777 = CARTESIAN_POINT ( 'NONE',  ( -23.51374020987026725, -290.7377699108475326, -344.9066014553536093 ) ) ;
#92778 = CARTESIAN_POINT ( 'NONE',  ( -11.30522686547490885, -291.0691197055824091, -198.3651785395221623 ) ) ;
#92779 = CARTESIAN_POINT ( 'NONE',  ( -90.35869808522477342, -272.3373592992242038, -219.8194490478255148 ) ) ;
#92780 = CARTESIAN_POINT ( 'NONE',  ( 38.22660939108778422, -292.7224300935576480, -256.1223194633552112 ) ) ;
#92781 = CARTESIAN_POINT ( 'NONE',  ( -82.99076951297975313, -288.1699095240115867, -328.2132589522969965 ) ) ;
#92782 = CARTESIAN_POINT ( 'NONE',  ( 25.27272622487605247, -292.3308470801798080, -309.9213489643938715 ) ) ;
#92783 = CARTESIAN_POINT ( 'NONE',  ( 19.83240214985690031, -289.4043862012323416, -316.3855955452976332 ) ) ;
#92784 = CARTESIAN_POINT ( 'NONE',  ( 39.58706461736021254, -296.0519495502702512, -270.3284710469133074 ) ) ;
#92785 = CIRCLE ( 'NONE', #80683, 25.00000000000000355 ) ;
#92786 = CARTESIAN_POINT ( 'NONE',  ( -99.02093906268960666, -291.9737445061645644, -313.0304528031829818 ) ) ;
#92787 = CARTESIAN_POINT ( 'NONE',  ( -111.5541497753442854, -288.3990361921856334, -282.3001608637193272 ) ) ;
#92788 = CARTESIAN_POINT ( 'NONE',  ( -110.8914229348953597, -292.3630273195871041, -285.1029486988791746 ) ) ;
#92789 = CARTESIAN_POINT ( 'NONE',  ( -8.172210052900707566, -287.3850792342683462, -203.1856068390513883 ) ) ;
#92790 = CARTESIAN_POINT ( 'NONE',  ( 34.52645792512056744, -295.2690317622800649, -248.3384867775273221 ) ) ;
#92791 = CARTESIAN_POINT ( 'NONE',  ( -113.1481451663846372, -270.7100043341520745, -270.3376630279467463 ) ) ;
#92792 = CARTESIAN_POINT ( 'NONE',  ( 189.9243309297870610, 215.0000000000000568, 20.22542485937349355 ) ) ;
#92793 = AXIS2_PLACEMENT_3D ( 'NONE', #57089, #71285, #64676 ) ;
#92794 = CARTESIAN_POINT ( 'NONE',  ( 32.18599689650407925, -277.1528831882408213, -241.1695116136054082 ) ) ;
#92795 = CARTESIAN_POINT ( 'NONE',  ( -40.33910760393814599, -281.0896855089778228, -345.3012020471741153 ) ) ;
#92796 = CARTESIAN_POINT ( 'NONE',  ( -111.4635745307208481, -296.0057253443188188, -249.9135207091414657 ) ) ;
#92797 = CARTESIAN_POINT ( 'NONE',  ( -24.39747877565732637, -272.4593499031792021, -197.4361741901698224 ) ) ;
#92798 = CARTESIAN_POINT ( 'NONE',  ( -110.7094331762306183, -276.4681587035067309, -283.0258827709869252 ) ) ;
#92799 = CARTESIAN_POINT ( 'NONE',  ( -99.62549899168176637, -274.2902654152014179, -231.5299590561883178 ) ) ;
#92800 = AXIS2_PLACEMENT_3D ( 'NONE', #35642, #7220, #64559 ) ;
#92801 = VECTOR ( 'NONE', #55262, 1000.000000000000000 ) ;
#92802 = CARTESIAN_POINT ( 'NONE',  ( -82.70891359407991672, -297.1111712945385079, -328.3673454429822982 ) ) ;
#92803 = CARTESIAN_POINT ( 'NONE',  ( 197.1933712184921603, 24.89666632552609826, 12.64285714285712992 ) ) ;
#92804 = CARTESIAN_POINT ( 'NONE',  ( -102.6811405173542369, -297.8020784537931718, -237.3338632265739250 ) ) ;
#92805 = DIRECTION ( 'NONE',  ( 0.9531768234071978929, -0.3024135303179465439, 0.000000000000000000 ) ) ;
#92807 = CARTESIAN_POINT ( 'NONE',  ( -109.1293176453904721, -272.5638151817186667, -256.8416908511349561 ) ) ;
#92806 = CARTESIAN_POINT ( 'NONE',  ( 19.07251357880367948, -284.8800978417655756, -220.3256434277620883 ) ) ;
#92808 = VECTOR ( 'NONE', #44363, 1000.000000000000000 ) ;
#92809 = CARTESIAN_POINT ( 'NONE',  ( -7.343129295381475075, -286.4346928648794233, -199.3884152920370525 ) ) ;
#92810 = CARTESIAN_POINT ( 'NONE',  ( 18.33913858318828005, -286.4911293135903065, -217.1298548559292954 ) ) ;
#92811 = CARTESIAN_POINT ( 'NONE',  ( -72.53538336964163591, -299.5689175071598243, -203.6716065847124355 ) ) ;
#92812 = CARTESIAN_POINT ( 'NONE',  ( -4.765896197686079638, -292.6219760243730548, -337.7462264828085949 ) ) ;
#92813 = EDGE_CURVE ( 'NONE', #16098, #74457, #67603, .T. ) ;
#92814 = CARTESIAN_POINT ( 'NONE',  ( -5.002626537620225911, -279.6643596081917735, -200.6593020770489204 ) ) ;
#92815 = EDGE_CURVE ( 'NONE', #65891, #31, #18880, .T. ) ;
#92816 = CARTESIAN_POINT ( 'NONE',  ( -114.2704648735229114, -282.0523547857346216, -270.3284710469133074 ) ) ;
#92817 = CARTESIAN_POINT ( 'NONE',  ( 205.2296996224750103, 68.12454877777268791, 0.000000000000000000 ) ) ;
#92818 = CARTESIAN_POINT ( 'NONE',  ( -29.14392665854766307, -287.7408694713238901, -343.2989477736718982 ) ) ;
#92819 = CARTESIAN_POINT ( 'NONE',  ( 197.1181226030119262, 72.74206317236959762, -12.08813930015187488 ) ) ;
#92820 = CARTESIAN_POINT ( 'NONE',  ( -42.83515596486595456, -287.1211847443145757, -345.2116553274981925 ) ) ;
#92821 = CARTESIAN_POINT ( 'NONE',  ( -60.78917333951024204, -299.3430539754077699, -200.3309442646652485 ) ) ;
#92822 = CARTESIAN_POINT ( 'NONE',  ( 14.74629461529344887, -282.1936574969902836, -214.3831060242029309 ) ) ;
#92824 = CARTESIAN_POINT ( 'NONE',  ( -4.827162856289269222, -282.6115206781774418, -335.7201637681377520 ) ) ;
#92823 = CARTESIAN_POINT ( 'NONE',  ( -89.59019870554278953, -293.8039212067739072, -324.7330857885210662 ) ) ;
#92825 = CARTESIAN_POINT ( 'NONE',  ( -112.8890979635703644, -296.9058484947580610, -255.4073796362336566 ) ) ;
#92826 = CARTESIAN_POINT ( 'NONE',  ( -84.53354290713501484, -298.9089797542448537, -213.6937905886628926 ) ) ;
#92827 = CARTESIAN_POINT ( 'NONE',  ( 37.62160898672623688, -283.5824370682346967, -272.7069509557205720 ) ) ;
#92828 = CARTESIAN_POINT ( 'NONE',  ( -95.79936664164830518, -294.9929660865950041, -314.4965136002880968 ) ) ;
#92829 = VERTEX_POINT ( 'NONE', #69456 ) ;
#92830 = CYLINDRICAL_SURFACE ( 'NONE', #58939, 7.500000000000013323 ) ;
#92831 = CARTESIAN_POINT ( 'NONE',  ( 20.64539316579068995, -284.1826044300177614, -317.3849305712267324 ) ) ;
#92832 = CARTESIAN_POINT ( 'NONE',  ( 104.1717476309105166, -299.5541904835127980, -192.9651424135224715 ) ) ;
#92833 = CARTESIAN_POINT ( 'NONE',  ( 21.27581636871891391, -285.6952119285919025, -317.1477375740089997 ) ) ;
#92834 = CARTESIAN_POINT ( 'NONE',  ( 39.39372618803411541, -274.6879006864496660, -265.4602870448940735 ) ) ;
#92835 = CARTESIAN_POINT ( 'NONE',  ( 31.80172097998576319, -293.0725072112369958, -246.7903474453153763 ) ) ;
#92836 = CARTESIAN_POINT ( 'NONE',  ( 36.21068992604088521, -283.0127505857650476, -265.8054985685174074 ) ) ;
#92837 = CARTESIAN_POINT ( 'NONE',  ( 34.60920556017164529, -276.9374025108861019, -253.8880014605112763 ) ) ;
#92838 = CARTESIAN_POINT ( 'NONE',  ( -38.70370545048507438, -284.4941871834200242, -346.7597517165867771 ) ) ;
#92839 = CARTESIAN_POINT ( 'NONE',  ( 35.09296335587882254, -280.5025075061399207, -282.2080598349747333 ) ) ;
#92840 = CARTESIAN_POINT ( 'NONE',  ( -106.2904436542752649, -280.9382004337196008, -240.8471990272735468 ) ) ;
#92841 = CARTESIAN_POINT ( 'NONE',  ( -78.84334023757111254, -273.6759164488199758, -205.5027039353578573 ) ) ;
#92842 = CARTESIAN_POINT ( 'NONE',  ( 22.63966541114735165, -276.0327784411712742, -318.6648456798098437 ) ) ;
#92843 = CARTESIAN_POINT ( 'NONE',  ( 22.12979309200113320, -294.8557204715738749, -225.5899699650828722 ) ) ;
#92844 = FACE_OUTER_BOUND ( 'NONE', #88328, .T. ) ;
#92845 = DIRECTION ( 'NONE',  ( 1.000000000000000000, 0.000000000000000000, 0.000000000000000000 ) ) ;
#92846 = CARTESIAN_POINT ( 'NONE',  ( -98.90385110540442781, -295.2865493959877767, -226.1977049698182896 ) ) ;
#92847 = CARTESIAN_POINT ( 'NONE',  ( 35.08233664242854388, -274.9328666446943430, -260.7305759664939160 ) ) ;
#92848 = VECTOR ( 'NONE', #29580, 1000.000000000000000 ) ;
#92849 = CARTESIAN_POINT ( 'NONE',  ( 28.98171758952452137, -295.5679498969847714, -308.2026640136495530 ) ) ;
#92850 = CARTESIAN_POINT ( 'NONE',  ( -13.88894752603242999, -295.9594982902865468, -343.2855796754116113 ) ) ;
#92851 = CARTESIAN_POINT ( 'NONE',  ( 33.13433877471279487, -289.8791274025601297, -295.5237165324286366 ) ) ;
#92852 = CARTESIAN_POINT ( 'NONE',  ( -70.07579912940701661, -275.4841491643225595, -337.6694883478669453 ) ) ;
#92853 = AXIS2_PLACEMENT_3D ( 'NONE', #88944, #15599, #59163 ) ;
#92854 = CARTESIAN_POINT ( 'NONE',  ( -88.05911419239056670, -279.6886364666779059, -324.8501820822274340 ) ) ;
#92855 = CARTESIAN_POINT ( 'NONE',  ( -48.02337380076793494, -293.2687780946819771, -344.0830528402298114 ) ) ;
#92856 = CARTESIAN_POINT ( 'NONE',  ( 12.16684849994686246, -282.5929109843434048, -213.0094912340223914 ) ) ;
#92857 = CARTESIAN_POINT ( 'NONE',  ( -49.45914084493316665, -284.8144938107437838, -198.0086857638848699 ) ) ;
#92858 = CARTESIAN_POINT ( 'NONE',  ( 181.7997601335249556, 252.1859019497369445, -165.9525674339327850 ) ) ;
#92859 = VERTEX_POINT ( 'NONE', #27309 ) ;
#92860 = CARTESIAN_POINT ( 'NONE',  ( -49.42084836320960051, -285.5607638911498611, -198.2944561798227596 ) ) ;
#92861 = ORIENTED_EDGE ( 'NONE', *, *, #27400, .T. ) ;
#92862 = CARTESIAN_POINT ( 'NONE',  ( 37.94859159815776195, -282.4486168879772094, -255.7712419592744766 ) ) ;
#92863 = AXIS2_PLACEMENT_3D ( 'NONE', #67667, #52971, #2793 ) ;
#92864 = CARTESIAN_POINT ( 'NONE',  ( -111.8366280341288217, -283.1220266745824574, -288.2636631830587248 ) ) ;
#92865 = VECTOR ( 'NONE', #23236, 1000.000000000000000 ) ;
#92866 = CARTESIAN_POINT ( 'NONE',  ( -112.1750488634762775, -279.7080529226809631, -253.2500066417094899 ) ) ;
#92867 = CARTESIAN_POINT ( 'NONE',  ( -111.4967616055142514, -279.8445091054852014, -288.4084171103550034 ) ) ;
#92868 = CARTESIAN_POINT ( 'NONE',  ( -53.28691492658256834, -297.7662352645559167, -340.3683826091709079 ) ) ;
#92869 = CARTESIAN_POINT ( 'NONE',  ( 85.57369694988886977, 82.79219029714946032, -302.3637402596039010 ) ) ;
#92870 = EDGE_LOOP ( 'NONE', ( #80852, #20107, #57715, #8161 ) ) ;
#92871 = CARTESIAN_POINT ( 'NONE',  ( -51.94351526458655144, -275.8651589396186523, -196.9130963471600069 ) ) ;
#92872 = CARTESIAN_POINT ( 'NONE',  ( -90.47616956950605527, -230.2765260023237204, -347.7368331188681623 ) ) ;
#92873 = AXIS2_PLACEMENT_3D ( 'NONE', #38387, #25578, #12316 ) ;
#92874 = CARTESIAN_POINT ( 'NONE',  ( -8.591038903044097452, -278.4504038211729835, -201.4753699399532820 ) ) ;
#92875 = CARTESIAN_POINT ( 'NONE',  ( -76.66431668589918047, -293.2940619400229707, -205.2796147166539811 ) ) ;
#92876 = CARTESIAN_POINT ( 'NONE',  ( 33.87284088849880703, -293.1188054656516329, -286.9202305669654152 ) ) ;
#92877 = CARTESIAN_POINT ( 'NONE',  ( -93.55212778230500703, -289.3421493711076664, -322.9727977038713220 ) ) ;
#92878 = CARTESIAN_POINT ( 'NONE',  ( 158.6539576904058606, 293.9636489450775230, 0.000000000000000000 ) ) ;
#92880 = CARTESIAN_POINT ( 'NONE',  ( -16.93128338593110627, -284.7198704381099787, -199.3862139363613437 ) ) ;
#92879 = CARTESIAN_POINT ( 'NONE',  ( -16.68376090604201778, -293.3652342773754640, -343.9812407148490934 ) ) ;
#92881 = CARTESIAN_POINT ( 'NONE',  ( -9.282195404500859226, -294.2831771746835443, -201.5784922947043185 ) ) ;
#92882 = CARTESIAN_POINT ( 'NONE',  ( -19.63065460626670244, -284.7639404852479288, -198.8277228649770336 ) ) ;
#92883 = CARTESIAN_POINT ( 'NONE',  ( 18.88237579884572170, -283.5353150190501879, -317.7103196935150322 ) ) ;
#92884 = VERTEX_POINT ( 'NONE', #84579 ) ;
#92885 = CARTESIAN_POINT ( 'NONE',  ( -103.0207607332826996, -292.0147752144574724, -230.5209505443164630 ) ) ;
#92886 = CARTESIAN_POINT ( 'NONE',  ( 26.50958233963024568, -281.5593876900824739, -234.8505256370674772 ) ) ;
#92887 = CARTESIAN_POINT ( 'NONE',  ( 15.19515410428097368, -293.1248168212677001, -326.1095499348656404 ) ) ;
#92888 = AXIS2_PLACEMENT_3D ( 'NONE', #27049, #54513, #48340 ) ;
#92889 = CARTESIAN_POINT ( 'NONE',  ( 36.63174046260067485, -288.6165656147635445, -291.1961425369566427 ) ) ;
#92890 = ADVANCED_FACE ( 'NONE', ( #92619 ), #13123, .T. ) ;
#92891 = CARTESIAN_POINT ( 'NONE',  ( -37.49516900964340493, -289.5463332417454012, -347.3124881977668679 ) ) ;
#92892 = CARTESIAN_POINT ( 'NONE',  ( 17.82692498352302835, -288.4008067648674114, -318.2429006435521615 ) ) ;
#92893 = VERTEX_POINT ( 'NONE', #34877 ) ;
#92894 = CARTESIAN_POINT ( 'NONE',  ( 194.4923472626465752, 26.08759934769913258, 14.31634348551539659 ) ) ;
#92895 = CARTESIAN_POINT ( 'NONE',  ( -36.26780400159414341, -296.8992701365683047, -346.1312037958138035 ) ) ;
#92896 = CARTESIAN_POINT ( 'NONE',  ( -70.50006269974683448, -296.3089134298974727, -201.4131574120132200 ) ) ;
#92897 = CARTESIAN_POINT ( 'NONE',  ( -91.14884666236504529, -276.8990072520734884, -320.1158736413113388 ) ) ;
#92898 = CARTESIAN_POINT ( 'NONE',  ( -76.39607400263459169, -273.0525669962132156, -204.0101741712486216 ) ) ;
#92899 = CARTESIAN_POINT ( 'NONE',  ( -10.25298149166816764, -293.1719150093079520, -338.8951173952573868 ) ) ;
#92900 = CARTESIAN_POINT ( 'NONE',  ( 34.88703270323007644, -277.5232384338306133, -286.5738290956944070 ) ) ;
#92901 = CARTESIAN_POINT ( 'NONE',  ( -101.7783570804827065, -271.1896539146687246, -233.3961333614975899 ) ) ;
#92902 = CARTESIAN_POINT ( 'NONE',  ( -2.944157319955445384, -295.7919262268183047, -335.1989121650426569 ) ) ;
#92903 = CARTESIAN_POINT ( 'NONE',  ( -82.53962862501616371, -296.7656260072712371, -328.1438806329443878 ) ) ;
#92904 = CARTESIAN_POINT ( 'NONE',  ( -25.01691449717860394, -296.4977570206539781, -345.6113000395394010 ) ) ;
#92905 = CARTESIAN_POINT ( 'NONE',  ( -112.4046897001549041, -294.4900537445482200, -275.1954604732495682 ) ) ;
#92906 = CARTESIAN_POINT ( 'NONE',  ( -31.92679025380941482, -298.7696888616834485, -193.4624692755411388 ) ) ;
#92907 = CARTESIAN_POINT ( 'NONE',  ( -79.85644511805752188, -290.0396288688492632, -210.2331097033479352 ) ) ;
#92908 = CARTESIAN_POINT ( 'NONE',  ( -103.8145530635746496, -275.0136687216667042, -235.5158606163035131 ) ) ;
#92909 = CARTESIAN_POINT ( 'NONE',  ( -49.71552673843546444, -274.3908660882439676, -194.3704383794815271 ) ) ;
#92910 = CARTESIAN_POINT ( 'NONE',  ( -108.9045957971519698, -296.6931218976637865, -284.9436818444152664 ) ) ;
#92911 = CARTESIAN_POINT ( 'NONE',  ( 27.85071668681591106, -283.0298027938352448, -232.5675260595379825 ) ) ;
#92912 = CARTESIAN_POINT ( 'NONE',  ( 33.10525203171939523, -280.6207722733769288, -300.3380091289097891 ) ) ;
#92913 = CARTESIAN_POINT ( 'NONE',  ( -30.23258465161730157, -282.3130283196431947, -346.9298665922988789 ) ) ;
#92914 = CARTESIAN_POINT ( 'NONE',  ( 39.21666439910256230, -274.8035345910203091, -262.5988920357814891 ) ) ;
#92915 = CARTESIAN_POINT ( 'NONE',  ( -2.735067194011227887, -278.9017805312781775, -202.4582409639698710 ) ) ;
#92916 = CARTESIAN_POINT ( 'NONE',  ( -95.38508574367567405, -277.2094317739892517, -222.5813593959834691 ) ) ;
#92917 = CARTESIAN_POINT ( 'NONE',  ( 3.270126175024986370, -273.1840322527841067, -208.9320209849939545 ) ) ;
#92918 = CARTESIAN_POINT ( 'NONE',  ( 32.90753917720181221, -277.8951031929577198, -296.7759385152284608 ) ) ;
#92919 = DIRECTION ( 'NONE',  ( 0.000000000000000000, 1.000000000000000000, -0.000000000000000000 ) ) ;
#92920 = DIRECTION ( 'NONE',  ( 0.000000000000000000, 0.000000000000000000, 1.000000000000000000 ) ) ;
#92921 = CARTESIAN_POINT ( 'NONE',  ( -55.84550241976100438, -293.5270836603111775, -344.0603941803383350 ) ) ;
#92922 = CARTESIAN_POINT ( 'NONE',  ( -53.02191043809781945, -289.8723591186568456, -196.6020361752016470 ) ) ;
#92923 = CARTESIAN_POINT ( 'NONE',  ( -7.190202469943082875, -292.4368558564719933, -199.4956340707202287 ) ) ;
#92924 = CARTESIAN_POINT ( 'NONE',  ( -20.51121980868179051, -278.8368119763187565, -343.6727349932750144 ) ) ;
#92925 = CARTESIAN_POINT ( 'NONE',  ( -16.04911868242266948, -272.3271897846799448, -198.3929367641325143 ) ) ;
#92926 = ADVANCED_FACE ( 'NONE', ( #27790 ), #56196, .F. ) ;
#92927 = CARTESIAN_POINT ( 'NONE',  ( 185.2519943799831879, 3.000000000000000000, 10.00000000000000000 ) ) ;
#92928 = CARTESIAN_POINT ( 'NONE',  ( -16.51482975628218597, -284.7053831647747870, -343.0483961740949326 ) ) ;
#92929 = DIRECTION ( 'NONE',  ( -0.000000000000000000, -0.000000000000000000, -1.000000000000000000 ) ) ;
#92930 = CARTESIAN_POINT ( 'NONE',  ( -55.16793606341359890, -283.8228492554528657, -197.4575361682418588 ) ) ;
#92931 = CARTESIAN_POINT ( 'NONE',  ( 157.7238125175282732, 19.47471017779399105, -10.32097897594415592 ) ) ;
#92932 = CARTESIAN_POINT ( 'NONE',  ( 29.84741888892822814, -292.7423746513612741, -299.9035076864358302 ) ) ;
#92933 = CARTESIAN_POINT ( 'NONE',  ( 36.89010749396630473, -285.7009403480349761, -271.0711986815784940 ) ) ;
#92934 = CARTESIAN_POINT ( 'NONE',  ( 164.2231345125756263, 249.5000000000000568, 22.80382896337008702 ) ) ;
#92935 = CARTESIAN_POINT ( 'NONE',  ( -39.77886561469352245, -293.0825783057031799, -345.3342840592745802 ) ) ;
#92936 = CARTESIAN_POINT ( 'NONE',  ( -109.5746610762987814, -282.7192859744682778, -294.9600428515508952 ) ) ;
#92937 = CARTESIAN_POINT ( 'NONE',  ( -65.13610088866967374, -281.2829201111977113, -201.9951052112525360 ) ) ;
#92938 = CARTESIAN_POINT ( 'NONE',  ( -49.29797004043021502, -287.1082131275349525, -194.6435561421023124 ) ) ;
#92939 = CARTESIAN_POINT ( 'NONE',  ( 25.45599057564264811, -279.2191912456597152, -227.4858155928311305 ) ) ;
#92940 = CARTESIAN_POINT ( 'NONE',  ( 27.03046584175159950, -288.0227341230162210, -304.8957891121283978 ) ) ;
#92941 = AXIS2_PLACEMENT_3D ( 'NONE', #44015, #79566, #43562 ) ;
#92942 = CARTESIAN_POINT ( 'NONE',  ( -68.26866413860632576, -278.8917934645388073, -337.1499535678766506 ) ) ;
#92943 = CARTESIAN_POINT ( 'NONE',  ( -91.07952257907312799, -278.6428103739348217, -320.0820335829324677 ) ) ;
#92944 = CARTESIAN_POINT ( 'NONE',  ( -65.29124487541788824, -287.6685758785660596, -200.3670538258703573 ) ) ;
#92945 = ORIENTED_EDGE ( 'NONE', *, *, #10705, .F. ) ;
#92946 = CARTESIAN_POINT ( 'NONE',  ( -31.90740253627349077, -297.9517514386424182, -193.3612665261361485 ) ) ;
#92947 = CARTESIAN_POINT ( 'NONE',  ( 37.32495697097782283, -289.5047005553334998, -268.2411436631842889 ) ) ;
#92948 = DIRECTION ( 'NONE',  ( 0.000000000000000000, 1.000000000000000000, 0.000000000000000000 ) ) ;
#92949 = CARTESIAN_POINT ( 'NONE',  ( -19.11405058567862625, -276.7662352645559167, -190.3538533559490702 ) ) ;
#92950 = ORIENTED_EDGE ( 'NONE', *, *, #75324, .F. ) ;
#92951 = CARTESIAN_POINT ( 'NONE',  ( -16.26637843760867597, -272.3236647173372376, -198.1554498022277642 ) ) ;
#92952 = CARTESIAN_POINT ( 'NONE',  ( 25.04781221936262270, -292.5368937865397356, -314.1330434568142209 ) ) ;
#92953 = CARTESIAN_POINT ( 'NONE',  ( -91.88666206080398524, -296.7543274982097614, -221.7521109003415631 ) ) ;
#92954 = CARTESIAN_POINT ( 'NONE',  ( 5.109105701991394355, -288.1575443531618816, -210.0605157465149944 ) ) ;
#92955 = AXIS2_PLACEMENT_3D ( 'NONE', #10381, #44511, #61078 ) ;
#92956 = CARTESIAN_POINT ( 'NONE',  ( 33.20391960337276060, -283.6070405065344175, -292.9176950231448018 ) ) ;
#92957 = CARTESIAN_POINT ( 'NONE',  ( -59.83636354609197383, -290.7633070791865180, -343.3857467687143981 ) ) ;
#92958 = CARTESIAN_POINT ( 'NONE',  ( -69.13698276741453697, -290.7768347648495819, -339.9625028512141967 ) ) ;
#92959 = CARTESIAN_POINT ( 'NONE',  ( -92.18709541518154538, -285.8362080841440616, -321.5175766653520100 ) ) ;
#92960 = CARTESIAN_POINT ( 'NONE',  ( -111.4399386335719129, -278.4564002010822037, -291.3003408645210470 ) ) ;
#92961 = CARTESIAN_POINT ( 'NONE',  ( 33.10004141577986303, -291.9849371363591217, -297.6974535867205987 ) ) ;
#92962 = CARTESIAN_POINT ( 'NONE',  ( -2.388245089953710654, -280.3349970199848258, -201.7369448303928152 ) ) ;
#92963 = VECTOR ( 'NONE', #70526, 1000.000000000000000 ) ;
#92964 = CARTESIAN_POINT ( 'NONE',  ( -29.88902839056538951, -276.0079089227348845, -196.5009584666116780 ) ) ;
#92965 = CARTESIAN_POINT ( 'NONE',  ( 39.58706461736021254, -296.0519495502702512, -270.3284710469133074 ) ) ;
#92966 = CARTESIAN_POINT ( 'NONE',  ( 35.61928822639121961, -273.5201355730913519, -248.9481044826185610 ) ) ;
#92967 = DIRECTION ( 'NONE',  ( 0.000000000000000000, 0.000000000000000000, 1.000000000000000000 ) ) ;
#92968 = CARTESIAN_POINT ( 'NONE',  ( 32.03701970916272046, -280.7541136489308542, -247.2978729372258613 ) ) ;
#92969 = CARTESIAN_POINT ( 'NONE',  ( -82.30077473322948833, -278.8558393342300405, -332.3828103828726626 ) ) ;
#92970 = CARTESIAN_POINT ( 'NONE',  ( -99.70776026949154414, -274.4003459515403165, -231.4802998328978276 ) ) ;
#92971 = CARTESIAN_POINT ( 'NONE',  ( -7.423735994318076514, -285.4935929101841339, -199.6099661249866983 ) ) ;
#92972 = CARTESIAN_POINT ( 'NONE',  ( -110.7924322208123442, -292.1937882761323522, -279.4695738358672656 ) ) ;
#92973 = CARTESIAN_POINT ( 'NONE',  ( -111.6675224746108910, -274.3645386415125813, -253.5649115234457440 ) ) ;
#92974 = CARTESIAN_POINT ( 'NONE',  ( -27.07935770312077395, -275.4950453770099443, -194.4925801084156944 ) ) ;
#92975 = CARTESIAN_POINT ( 'NONE',  ( 157.5411741086738004, 275.0000000000000568, 16.22085278731064761 ) ) ;
#92976 = CARTESIAN_POINT ( 'NONE',  ( 7.173461836765138600, -296.4447451395572557, -330.5790886482362794 ) ) ;
#92977 = CARTESIAN_POINT ( 'NONE',  ( -101.9976272784508069, -282.0475739665027959, -308.0392218192928908 ) ) ;
#92978 = CARTESIAN_POINT ( 'NONE',  ( -84.25010434077037758, -291.0938097002024847, -209.2583270212768980 ) ) ;
#92979 = CARTESIAN_POINT ( 'NONE',  ( 14.66019250744243863, -272.8088843864364890, -216.8106748148640861 ) ) ;
#92980 = CARTESIAN_POINT ( 'NONE',  ( -18.40079044007968179, -287.8922198484396517, -196.4981751354647770 ) ) ;
#92981 = CARTESIAN_POINT ( 'NONE',  ( -70.34762781056551262, -290.5267630775066436, -204.9024683449930819 ) ) ;
#92982 = ORIENTED_EDGE ( 'NONE', *, *, #61610, .T. ) ;
#92983 = CARTESIAN_POINT ( 'NONE',  ( -105.9921682239077114, -288.6913632245349959, -304.0331896521166755 ) ) ;
#92984 = CARTESIAN_POINT ( 'NONE',  ( -110.3582371856074502, -290.2080515255307205, -271.1813635585348266 ) ) ;
#92985 = ORIENTED_EDGE ( 'NONE', *, *, #36695, .F. ) ;
#92986 = CARTESIAN_POINT ( 'NONE',  ( 22.74110137478180960, -287.9912237450164412, -222.6794168877924847 ) ) ;
#92987 = CARTESIAN_POINT ( 'NONE',  ( -29.70699456949141037, -277.2862492517654687, -343.0329638910351377 ) ) ;
#92988 = CARTESIAN_POINT ( 'NONE',  ( 17.33149365582932333, -293.2145233336383399, -324.2170639801052516 ) ) ;
#92989 = CARTESIAN_POINT ( 'NONE',  ( -27.37707892590487901, -283.5802477009421523, -346.6641243589059513 ) ) ;
#92990 = CARTESIAN_POINT ( 'NONE',  ( -80.92972839828624387, -285.8116507127966202, -206.8473613274224761 ) ) ;
#92991 = CARTESIAN_POINT ( 'NONE',  ( -26.73551153524960000, -283.2469477231186374, -342.6592061572064836 ) ) ;
#92992 = CARTESIAN_POINT ( 'NONE',  ( -13.02681774958086436, -91.53595701093347259, -360.0716045900807103 ) ) ;
#92993 = CARTESIAN_POINT ( 'NONE',  ( -49.28614775429143435, -154.2781463013184862, -364.0998538831054816 ) ) ;
#92994 = CARTESIAN_POINT ( 'NONE',  ( 201.3567858607021890, 292.7456558654927790, -53.99999999998547651 ) ) ;
#92995 = CARTESIAN_POINT ( 'NONE',  ( 51.83402786492749215, -298.5460828057790081, -197.2694149549886049 ) ) ;
#92996 = CARTESIAN_POINT ( 'NONE',  ( -43.49441721609006350, -272.8930728635862124, -197.2597297665910787 ) ) ;
#92997 = CARTESIAN_POINT ( 'NONE',  ( -94.60996724338600927, -295.3619624269710471, -321.7604380975172944 ) ) ;
#92998 = CARTESIAN_POINT ( 'NONE',  ( -75.80676782499371313, -208.7722911414634837, -353.9980045067355263 ) ) ;
#92999 = CARTESIAN_POINT ( 'NONE',  ( -67.32683342920005032, -272.3518792780071749, -199.9751104633308216 ) ) ;
#93000 = CARTESIAN_POINT ( 'NONE',  ( -102.3067754879293716, -298.8953373668895779, -234.4389178631257948 ) ) ;
#93001 = CARTESIAN_POINT ( 'NONE',  ( 33.56211362645411356, -289.1233028498329531, -289.8864344532447035 ) ) ;
#93002 = CARTESIAN_POINT ( 'NONE',  ( -108.0536675058858975, -291.8862691770031574, -251.0209074405942431 ) ) ;
#93003 = ORIENTED_EDGE ( 'NONE', *, *, #59598, .F. ) ;
#93004 = CARTESIAN_POINT ( 'NONE',  ( -102.1242746498049883, -298.0348313538002003, -229.1781330127871854 ) ) ;
#93005 = CARTESIAN_POINT ( 'NONE',  ( 35.02219564102053795, -288.1784640545204184, -280.5247508595293198 ) ) ;
#93006 = CARTESIAN_POINT ( 'NONE',  ( 37.62863802467123264, -294.5667830215093090, -287.2611824451497569 ) ) ;
#93007 = CARTESIAN_POINT ( 'NONE',  ( -1.990168916674266431, -295.0889824890612090, -338.6970246820822013 ) ) ;
#93008 = CARTESIAN_POINT ( 'NONE',  ( 4.501905968599356989, -292.8007518216258518, -210.4818265202907241 ) ) ;
#93009 = ORIENTED_EDGE ( 'NONE', *, *, #57561, .F. ) ;
#93010 = CIRCLE ( 'NONE', #52169, 5.568361562975243650 ) ;
#93011 = CARTESIAN_POINT ( 'NONE',  ( 32.85570986290937867, -277.8353555829073116, -298.4600837444673971 ) ) ;
#93012 = EDGE_LOOP ( 'NONE', ( #49071, #19376, #17538 ) ) ;
#93013 = CARTESIAN_POINT ( 'NONE',  ( -72.47311556739037997, -279.1074464091064442, -201.8971504870321212 ) ) ;
#93014 = CARTESIAN_POINT ( 'NONE',  ( 28.24655160184914138, -276.9351408064773068, -303.0575238390532604 ) ) ;
#93015 = CARTESIAN_POINT ( 'NONE',  ( -41.16451793200949538, -275.7649309509974387, -194.4190989342198463 ) ) ;
#93016 = CARTESIAN_POINT ( 'NONE',  ( 2.607674430618251993, -274.5398401645783792, -334.3166156221017786 ) ) ;
#93017 = CARTESIAN_POINT ( 'NONE',  ( -102.6270985249105792, -297.6506834490274400, -237.3590328285499425 ) ) ;
#93018 = CIRCLE ( 'NONE', #38529, 0.5000000000000004441 ) ;
#93019 = CARTESIAN_POINT ( 'NONE',  ( -110.7993925224842826, -295.1844250214292060, -265.9631248194395425 ) ) ;
#93020 = DIRECTION ( 'NONE',  ( -1.000000000000000000, 0.000000000000000000, 0.000000000000000000 ) ) ;
#93021 = CARTESIAN_POINT ( 'NONE',  ( -103.5496369594317798, -278.5323347258338345, -309.6578755844608963 ) ) ;
#93022 = CARTESIAN_POINT ( 'NONE',  ( -9.986393335047198505, -276.8514442498514541, -338.0554580504505111 ) ) ;
#93023 = CIRCLE ( 'NONE', #24964, 25.00000000000000355 ) ;
#93024 = CARTESIAN_POINT ( 'NONE',  ( 21.72021964146207651, -285.5794136726498778, -221.7299766454424059 ) ) ;
#93025 = CARTESIAN_POINT ( 'NONE',  ( -112.1870949185858848, -274.6237131154039730, -264.8005701362116042 ) ) ;
#93026 = CARTESIAN_POINT ( 'NONE',  ( 82.65242050738238788, -299.2778291467535610, -197.8518630440875086 ) ) ;
#93027 = CARTESIAN_POINT ( 'NONE',  ( 32.82773924352123629, -286.4753734195056722, -249.6081724534010391 ) ) ;
#93028 = ADVANCED_FACE ( 'NONE', ( #6471 ), #6003, .F. ) ;
#93029 = CARTESIAN_POINT ( 'NONE',  ( -71.38812873509660051, -277.8360507084383926, -204.6291472771451083 ) ) ;
#93030 = CARTESIAN_POINT ( 'NONE',  ( -106.0580368999380880, -277.4774390692523411, -243.8852364212453381 ) ) ;
#93031 = CARTESIAN_POINT ( 'NONE',  ( -109.9380293223078127, -286.3097024978841318, -289.2464904731759248 ) ) ;
#93032 = CARTESIAN_POINT ( 'NONE',  ( -18.90245113411350886, -278.0144995283549747, -341.4042358773270394 ) ) ;
#93033 = LINE ( 'NONE', #27238, #24578 ) ;
#93034 = CARTESIAN_POINT ( 'NONE',  ( -9.602886348971278352, -274.9345012027821440, -341.1038365056431303 ) ) ;
#93035 = CARTESIAN_POINT ( 'NONE',  ( 15.51476457488577587, -275.4754439798660997, -219.7894674575021838 ) ) ;
#93036 = CARTESIAN_POINT ( 'NONE',  ( 26.75531443692228706, -284.0789346990802073, -309.7230377057543933 ) ) ;
#93037 = PLANE ( 'NONE',  #6628 ) ;
#93038 = CARTESIAN_POINT ( 'NONE',  ( 26.24644227083116732, -290.0190225437839899, -311.2726156472203911 ) ) ;
#93039 = CARTESIAN_POINT ( 'NONE',  ( -2.318195957178805777, -292.5889292846150056, -336.7378603377529203 ) ) ;
#93040 = CARTESIAN_POINT ( 'NONE',  ( 165.2494399300530290, 8.542400036368780647, 9.974999999999996092 ) ) ;
#93041 = CARTESIAN_POINT ( 'NONE',  ( -51.64112410093822803, -272.5503579319287155, -198.2203552791679613 ) ) ;
#93042 = CARTESIAN_POINT ( 'NONE',  ( 24.38120489545429592, -291.1285111381977231, -229.1161367624762590 ) ) ;
#93043 = CARTESIAN_POINT ( 'NONE',  ( -78.59295187722810283, -208.2960365483323244, -357.4574221067172743 ) ) ;
#93044 = CARTESIAN_POINT ( 'NONE',  ( 199.1087447750284980, 64.61450673763175701, -10.46317447812566570 ) ) ;
#93045 = CARTESIAN_POINT ( 'NONE',  ( -75.33541529648984181, -288.0290666810647622, -336.5365315481849962 ) ) ;
#93046 = CARTESIAN_POINT ( 'NONE',  ( -104.8368268042791556, -285.7549519031385898, -300.2081997175055221 ) ) ;
#93047 = CARTESIAN_POINT ( 'NONE',  ( -0.1917901401555877350, -284.7790798864511999, -204.0600822206697842 ) ) ;
#93048 = EDGE_CURVE ( 'NONE', #4223, #27414, #37191, .T. ) ;
#93049 = CARTESIAN_POINT ( 'NONE',  ( -66.77873918761075345, -284.8708354357335679, -337.8198532561770548 ) ) ;
#93050 = CARTESIAN_POINT ( 'NONE',  ( -37.53069501245036577, -283.8574474257169982, -343.5348076018982511 ) ) ;
#93051 = CARTESIAN_POINT ( 'NONE',  ( -93.50266628165103100, -293.2283898004811249, -220.1181813164247671 ) ) ;
#93052 = CARTESIAN_POINT ( 'NONE',  ( 29.97862184496998950, -273.1817012103730917, -236.0494808218185199 ) ) ;
#93053 = CARTESIAN_POINT ( 'NONE',  ( -46.88258587029088886, -274.2674179150606051, -193.9758066280504352 ) ) ;
#93054 = CARTESIAN_POINT ( 'NONE',  ( -110.2370002989357829, -288.8864269982775568, -250.4226518658473424 ) ) ;
#93055 = CARTESIAN_POINT ( 'NONE',  ( -17.35789933755228986, -276.8011508202511095, -344.7227190005884268 ) ) ;
#93056 = CARTESIAN_POINT ( 'NONE',  ( -25.93166203061819886, -296.8860210818939436, -344.1287113486369549 ) ) ;
#93057 = CARTESIAN_POINT ( 'NONE',  ( -48.18343439339133738, -253.0206516614774728, -463.6603765730280315 ) ) ;
#93058 = CARTESIAN_POINT ( 'NONE',  ( 209.3354045562396379, 36.47363971095035140, 13.48243931971275167 ) ) ;
#93059 = CARTESIAN_POINT ( 'NONE',  ( -107.8698714033939865, -282.9648861105554261, -291.0705614155507988 ) ) ;
#93060 = CARTESIAN_POINT ( 'NONE',  ( -76.42789811154166557, -277.5296757881509393, -206.2910869157447848 ) ) ;
#93061 = CARTESIAN_POINT ( 'NONE',  ( 169.9462594094670180, 275.5000000000000568, -23.92352941176469727 ) ) ;
#93062 = CARTESIAN_POINT ( 'NONE',  ( -108.5128642368318452, -271.3854633129844274, -242.6953564316367249 ) ) ;
#93063 = CARTESIAN_POINT ( 'NONE',  ( -97.73771417988540122, -277.3285540484964713, -311.5462385349812848 ) ) ;
#93064 = CARTESIAN_POINT ( 'NONE',  ( -28.03782170694745446, -293.6923771513891097, -197.2062251197209832 ) ) ;
#93065 = CARTESIAN_POINT ( 'NONE',  ( -19.81345734441296003, -279.1925818874099718, -195.6456432837802026 ) ) ;
#93066 = CARTESIAN_POINT ( 'NONE',  ( 21.98831031567865324, -293.8944293638078875, -227.4054485807543529 ) ) ;
#93067 = EDGE_CURVE ( 'NONE', #91019, #26459, #61407, .T. ) ;
#93068 = CARTESIAN_POINT ( 'NONE',  ( -47.54909627123434035, -296.4944988658038483, -346.1839861415475639 ) ) ;
#93069 = CARTESIAN_POINT ( 'NONE',  ( -99.89569917015704448, -296.9044136526502484, -232.6330814757076553 ) ) ;
#93070 = CARTESIAN_POINT ( 'NONE',  ( -79.27202385440597254, -291.6177795216910908, -332.6076168281423406 ) ) ;
#93071 = CARTESIAN_POINT ( 'NONE',  ( -106.6800326892034576, -285.1484475823513662, -236.8768583651322501 ) ) ;
#93072 = CARTESIAN_POINT ( 'NONE',  ( -78.15589703447028569, -271.6491471499148247, -206.5292543873677857 ) ) ;
#93073 = CARTESIAN_POINT ( 'NONE',  ( 39.34725525326049933, -287.4719423508337854, -277.2751708469426148 ) ) ;
#93074 = CARTESIAN_POINT ( 'NONE',  ( -84.49587380032733108, -281.3795587611379005, -212.4294362897949497 ) ) ;
#93075 = CARTESIAN_POINT ( 'NONE',  ( -44.03398219609740494, -285.0242068742987840, -197.4322361261056358 ) ) ;
#93076 = CARTESIAN_POINT ( 'NONE',  ( -12.90021255846555803, -286.7344887951414876, -341.3212026923465032 ) ) ;
#93077 = CARTESIAN_POINT ( 'NONE',  ( 65.71450562203199297, 45.78484130816451625, -315.1169351998001389 ) ) ;
#93078 = CARTESIAN_POINT ( 'NONE',  ( -35.92599322437101250, -285.5780356783108118, -197.3132965515756041 ) ) ;
#93079 = CARTESIAN_POINT ( 'NONE',  ( -1.732611843408993213, -283.5332029453692826, -338.3670959927394506 ) ) ;
#93080 = CARTESIAN_POINT ( 'NONE',  ( -92.63425842660852538, -290.3428300924794598, -217.0355948503207628 ) ) ;
#93081 = CARTESIAN_POINT ( 'NONE',  ( -110.5741047771483068, -280.4190676228725465, -249.3027389963448854 ) ) ;
#93082 = CARTESIAN_POINT ( 'NONE',  ( -68.48720090725359455, -280.9666015271668584, -200.4665246857018701 ) ) ;
#93083 = CARTESIAN_POINT ( 'NONE',  ( 33.45610174191814679, -281.1500165434163137, -252.5150661209417535 ) ) ;
#93084 = CARTESIAN_POINT ( 'NONE',  ( 35.85051572032931944, -277.7632188498862433, -286.7872602501676056 ) ) ;
#93085 = CARTESIAN_POINT ( 'NONE',  ( -1.967479606768923972, -294.5967149062826707, -338.7545717812208750 ) ) ;
#93086 = CARTESIAN_POINT ( 'NONE',  ( 21.64198774099219946, -286.2026102814044179, -316.1286215399728690 ) ) ;
#93087 = CIRCLE ( 'NONE', #3867, 0.5000000000000003331 ) ;
#93088 = CARTESIAN_POINT ( 'NONE',  ( -95.06833701218657495, -292.8311306700215368, -220.6010848072217243 ) ) ;
#93089 = CARTESIAN_POINT ( 'NONE',  ( -94.68454819221240371, -296.1147713699570545, -224.6881078929420426 ) ) ;
#93090 = EDGE_LOOP ( 'NONE', ( #72130, #89577 ) ) ;
#93091 = CARTESIAN_POINT ( 'NONE',  ( -38.89100651573278355, -284.9918561178558321, -344.7977351325462223 ) ) ;
#93092 = CARTESIAN_POINT ( 'NONE',  ( -93.96163396402897661, -295.5661548307197677, -316.4922725720511494 ) ) ;
#93093 = CARTESIAN_POINT ( 'NONE',  ( 21.06605969209302742, -293.9588272986272273, -220.6417030200217653 ) ) ;
#93094 = CARTESIAN_POINT ( 'NONE',  ( -90.81036690005215917, -284.4876784674281112, -320.2108355532662358 ) ) ;
#93095 = CARTESIAN_POINT ( 'NONE',  ( 24.29811901751222791, -274.0007147202811097, -224.6079442208886974 ) ) ;
#93096 = CARTESIAN_POINT ( 'NONE',  ( -59.98933079607509455, -289.9895726250152848, -343.8485156196079515 ) ) ;
#93097 = CARTESIAN_POINT ( 'NONE',  ( -83.15545261262880672, -281.8111243733034144, -330.7710974910717709 ) ) ;
#93098 = CARTESIAN_POINT ( 'NONE',  ( 26.38375981320465868, -287.3966455321070157, -234.6044379002715061 ) ) ;
#93099 = DIRECTION ( 'NONE',  ( 0.9764705882352963107, -0.000000000000000000, 0.2156506209390885997 ) ) ;
#93100 = DIRECTION ( 'NONE',  ( 0.000000000000000000, 0.000000000000000000, 1.000000000000000000 ) ) ;
#93101 = CARTESIAN_POINT ( 'NONE',  ( 5.919522898407217681, -59.40102248639579585, -350.9217243335569378 ) ) ;
#93102 = CARTESIAN_POINT ( 'NONE',  ( -69.85430415644619018, -271.1237833571632905, -202.7746430608542312 ) ) ;
#93103 = CARTESIAN_POINT ( 'NONE',  ( -66.12383106651755327, -278.8627301550951074, -203.0853455465862965 ) ) ;
#93104 = VERTEX_POINT ( 'NONE', #33461 ) ;
#93105 = CARTESIAN_POINT ( 'NONE',  ( -1.804242960465771040, -279.4551587318641737, -206.2415795241771264 ) ) ;
#93106 = CARTESIAN_POINT ( 'NONE',  ( 38.90381832115386374, -275.0862650558409541, -259.7608723289450268 ) ) ;
#93107 = CARTESIAN_POINT ( 'NONE',  ( 200.8605831797993062, 286.2175693065611313, -96.73721376744219924 ) ) ;
#93108 = CARTESIAN_POINT ( 'NONE',  ( -25.46910903888736044, -278.7753607374153830, -194.8783525826691516 ) ) ;
#93109 = CARTESIAN_POINT ( 'NONE',  ( 6.539107288121340567, -280.4725110617044948, -330.7458970281825259 ) ) ;
#93110 = CARTESIAN_POINT ( 'NONE',  ( -87.91408334400087199, -297.5075524510115770, -327.1450434393960904 ) ) ;
#93111 = CARTESIAN_POINT ( 'NONE',  ( 10.33641514772100400, -294.8652731128516393, -325.7216252528195923 ) ) ;
#93112 = VERTEX_POINT ( 'NONE', #19268 ) ;
#93113 = CARTESIAN_POINT ( 'NONE',  ( -91.10862421313703408, -289.9527849138713691, -220.2390095541911990 ) ) ;
#93114 = CARTESIAN_POINT ( 'NONE',  ( 23.54704104386278374, -275.5756721324939917, -223.3729548992785965 ) ) ;
#93115 = CARTESIAN_POINT ( 'NONE',  ( -74.27338320858079612, -273.5467846817364261, -207.3339124957474837 ) ) ;
#93116 = ORIENTED_EDGE ( 'NONE', *, *, #68258, .F. ) ;
#93117 = DIRECTION ( 'NONE',  ( 0.000000000000000000, 0.000000000000000000, -1.000000000000000000 ) ) ;
#93118 = CARTESIAN_POINT ( 'NONE',  ( 196.0143093133015384, 73.40565171261609123, -11.99999999999998046 ) ) ;
#93119 = CARTESIAN_POINT ( 'NONE',  ( 9.463374133154447421, -281.7927296435440212, -213.8723435883612467 ) ) ;
#93120 = CARTESIAN_POINT ( 'NONE',  ( -11.87042734609747008, -282.1392417980473510, -198.7154593833747356 ) ) ;
#93121 = CARTESIAN_POINT ( 'NONE',  ( -97.73315469419704016, -283.0350247642923591, -311.8775397146829960 ) ) ;
#93122 = CARTESIAN_POINT ( 'NONE',  ( 32.21957138567422874, -283.0708036584871365, -244.2889745518489519 ) ) ;
#93123 = CARTESIAN_POINT ( 'NONE',  ( 35.71033753081844253, -273.9052576440688540, -260.6602135802889393 ) ) ;
#93124 = DIRECTION ( 'NONE',  ( -1.000000000000000000, 4.440892098500622123E-13, 0.000000000000000000 ) ) ;
#93125 = CARTESIAN_POINT ( 'NONE',  ( 202.4316997032785537, 63.54496854667812755, -6.999999999999996447 ) ) ;
#93126 = CARTESIAN_POINT ( 'NONE',  ( -42.78450690990434424, -277.9220227374310070, -347.0066310598303403 ) ) ;
#93127 = ORIENTED_EDGE ( 'NONE', *, *, #51125, .T. ) ;
#93128 = ORIENTED_EDGE ( 'NONE', *, *, #78174, .T. ) ;
#93129 = CARTESIAN_POINT ( 'NONE',  ( 208.3305877567938751, 27.64722171545246709, 11.99999999999999822 ) ) ;
#93130 = CARTESIAN_POINT ( 'NONE',  ( -111.9668163267544685, -286.3936198589705100, -281.1929735122029115 ) ) ;
#93131 = CARTESIAN_POINT ( 'NONE',  ( 30.00838957883324198, -292.3649631812576217, -241.6558253157915885 ) ) ;
#93132 = CARTESIAN_POINT ( 'NONE',  ( -36.09682285605904895, -288.3855521207364063, -347.2622014783534041 ) ) ;
#93133 = ADVANCED_FACE ( 'NONE', ( #56683 ), #55175, .F. ) ;
#93134 = CARTESIAN_POINT ( 'NONE',  ( -109.0042749793001065, -283.0329551182600198, -251.8557300806889998 ) ) ;
#93136 = CARTESIAN_POINT ( 'NONE',  ( -40.01690294164932027, -287.3259529322153298, -344.3763600051889853 ) ) ;
#93135 = CARTESIAN_POINT ( 'NONE',  ( -94.56889780037019477, -283.7761620456114429, -224.0764497911150954 ) ) ;
#93137 = CARTESIAN_POINT ( 'NONE',  ( 8.051511651281192172, -283.6210873779231179, -328.1026085126521821 ) ) ;
#93138 = CARTESIAN_POINT ( 'NONE',  ( 0.2165205984923093130, -272.5520562238553453, -205.4279655805774780 ) ) ;
#93139 = CARTESIAN_POINT ( 'NONE',  ( -103.3372930389460862, -283.4536427480870771, -232.1639501995029491 ) ) ;
#93140 = CARTESIAN_POINT ( 'NONE',  ( -66.13250785542608412, -297.4290927360626711, -339.6287572299213480 ) ) ;
#93141 = CARTESIAN_POINT ( 'NONE',  ( -109.9436069472899078, -282.8039599072970418, -250.6980402026196089 ) ) ;
#93142 = CARTESIAN_POINT ( 'NONE',  ( -94.98345866781528457, -280.1284964571382829, -225.1653147560482751 ) ) ;
#93143 = CARTESIAN_POINT ( 'NONE',  ( 28.51277332754802885, -289.0702739978530076, -234.0148528554576615 ) ) ;
#93144 = CARTESIAN_POINT ( 'NONE',  ( 195.4479150618181791, 27.22655798642326985, 13.98918657931467635 ) ) ;
#93145 = FACE_BOUND ( 'NONE', #44508, .T. ) ;
#93146 = CARTESIAN_POINT ( 'NONE',  ( 34.08324848750269354, -295.1537932293272206, -245.5494747685061441 ) ) ;
#93147 = AXIS2_PLACEMENT_3D ( 'NONE', #41114, #43031, #70046 ) ;
#93148 = CARTESIAN_POINT ( 'NONE',  ( -46.16807715613111185, -275.1638176601100554, -344.8919588464014510 ) ) ;
#93149 = CARTESIAN_POINT ( 'NONE',  ( -101.5434026802915497, -290.3065588331792810, -228.0483588684395500 ) ) ;
#93150 = CARTESIAN_POINT ( 'NONE',  ( -2.787021886263308712, -292.9871755478962996, -335.5716587581698604 ) ) ;
#93151 = CARTESIAN_POINT ( 'NONE',  ( -85.79684564789548062, -278.0491499384419285, -215.1040609725515651 ) ) ;
#93152 = CARTESIAN_POINT ( 'NONE',  ( -111.7817001273664914, -270.6323071128609854, -270.3367258320721476 ) ) ;
#93153 = CARTESIAN_POINT ( 'NONE',  ( -82.04217990329473764, -292.7436585343715478, -211.9605230838566854 ) ) ;
#93154 = CARTESIAN_POINT ( 'NONE',  ( 10.59707575819634329, -277.1948066931274184, -210.1954327657594490 ) ) ;
#93155 = CARTESIAN_POINT ( 'NONE',  ( -1.053108605244923890, -293.0594187530589920, -337.5014653714754900 ) ) ;
#93156 = CARTESIAN_POINT ( 'NONE',  ( 23.42002051306367250, -289.7295423746724055, -312.2696011030996601 ) ) ;
#93157 = CARTESIAN_POINT ( 'NONE',  ( -7.566342243576914761, -290.6769990101252574, -200.4370257377942153 ) ) ;
#93158 = EDGE_CURVE ( 'NONE', #39909, #39706, #85530, .T. ) ;
#93159 = CARTESIAN_POINT ( 'NONE',  ( -45.40916316825265397, -290.5816462755353768, -343.5068010866767167 ) ) ;
#93160 = EDGE_CURVE ( 'NONE', #12543, #27549, #93018, .T. ) ;
#93161 = CARTESIAN_POINT ( 'NONE',  ( 10.41963433625062230, -229.5268262511776527, 21.50000000000000000 ) ) ;
#93162 = CARTESIAN_POINT ( 'NONE',  ( -13.22502340328375325, -289.5335340590501687, -339.4334542002155217 ) ) ;
#93163 = B_SPLINE_CURVE_WITH_KNOTS ( 'NONE', 3,
 ( #10571, #25258, #83004, #92927 ),
 .UNSPECIFIED., .F., .F.,
 ( 4, 4 ),
 ( 0.000000000000000000, 1.000000000000000000 ),
 .UNSPECIFIED. ) ;
#93164 = CARTESIAN_POINT ( 'NONE',  ( 144.7857639756989272, -299.5541904835127980, -195.3611179825600175 ) ) ;
#93165 = CARTESIAN_POINT ( 'NONE',  ( -106.1500589670266663, -291.3212879949576291, -304.1479227005356734 ) ) ;
#93167 = CARTESIAN_POINT ( 'NONE',  ( -102.4095665108567346, -291.0029521426351948, -237.1558258851979417 ) ) ;
#93166 = CARTESIAN_POINT ( 'NONE',  ( 24.93581247954994851, -278.9994757435598558, -227.8445861780787425 ) ) ;
#93168 = CARTESIAN_POINT ( 'NONE',  ( -28.23171886346071346, -280.4978958992466005, -193.8696082705689889 ) ) ;
#93169 = CARTESIAN_POINT ( 'NONE',  ( 36.45719177757317198, -281.4957414389079418, -292.4412136093652066 ) ) ;
#93170 = CARTESIAN_POINT ( 'NONE',  ( 28.78206567304079400, -286.0228955512463926, -305.8643518758161690 ) ) ;
#93171 = CARTESIAN_POINT ( 'NONE',  ( 209.2568086740256206, 34.98978593258855341, 14.00000000000000000 ) ) ;
#93172 = CARTESIAN_POINT ( 'NONE',  ( 21.13964999677434164, -280.3255648648585066, -316.0863535890235312 ) ) ;
#93173 = CARTESIAN_POINT ( 'NONE',  ( -110.4054452489891389, -282.7694014932187656, -253.4292013009956008 ) ) ;
#93174 = DIRECTION ( 'NONE',  ( -1.000000000000000000, -0.000000000000000000, -0.000000000000000000 ) ) ;
#93175 = CARTESIAN_POINT ( 'NONE',  ( -6.492755947594490706, -278.9298411078752906, -200.5540615095610519 ) ) ;
#93176 = CARTESIAN_POINT ( 'NONE',  ( 23.62410741522981539, -285.8494631136304633, -223.8136448187762824 ) ) ;
#93177 = CARTESIAN_POINT ( 'NONE',  ( 19.11695759141926487, -275.6969973515500101, -223.8313243444474097 ) ) ;
#93178 = CARTESIAN_POINT ( 'NONE',  ( 164.2231345125756263, 264.6571197653884155, -7.500000000000000000 ) ) ;
#93179 = CARTESIAN_POINT ( 'NONE',  ( -37.57268920814497193, -293.6493788064684054, -196.5488969111771951 ) ) ;
#93180 = CARTESIAN_POINT ( 'NONE',  ( 19.58466405522391085, -276.2800653926019550, -219.3128497882555052 ) ) ;
#93181 = CARTESIAN_POINT ( 'NONE',  ( -83.02329073002005089, -277.3637853461275427, -327.3935549608236215 ) ) ;
#93182 = CARTESIAN_POINT ( 'NONE',  ( -104.6110077779511158, -291.2045613214863806, -232.8932617215579626 ) ) ;
#93183 = CARTESIAN_POINT ( 'NONE',  ( 33.97680217068388941, -279.3094003535211982, -245.2450221761572209 ) ) ;
#93184 = CARTESIAN_POINT ( 'NONE',  ( -86.51140065456102946, -291.2244386477576086, -211.0353227272537993 ) ) ;
#93185 = CARTESIAN_POINT ( 'NONE',  ( -77.37378323696128746, -290.5592624433946867, -209.0354237774879209 ) ) ;
#93186 = CARTESIAN_POINT ( 'NONE',  ( -50.15165102018294618, -293.2153406318451516, -344.3116058711942173 ) ) ;
#93187 = ORIENTED_EDGE ( 'NONE', *, *, #48476, .F. ) ;
#93188 = CARTESIAN_POINT ( 'NONE',  ( 151.6573119020196145, 20.00000000000000000, 4.897109440894215737 ) ) ;
#93189 = CARTESIAN_POINT ( 'NONE',  ( -41.59015181807210126, -291.5049936054648470, -197.3733166614469212 ) ) ;
#93190 = DIRECTION ( 'NONE',  ( -0.000000000000000000, -0.000000000000000000, -1.000000000000000000 ) ) ;
#93191 = CARTESIAN_POINT ( 'NONE',  ( 17.40634833298269157, -272.4094976428775681, -226.7417163044926838 ) ) ;
#93192 = CARTESIAN_POINT ( 'NONE',  ( -108.6655231179850318, -295.9736987428496491, -241.8329011001955564 ) ) ;
#93193 = CARTESIAN_POINT ( 'NONE',  ( -111.8830607454059702, -286.0841991713620587, -253.1308007344528903 ) ) ;
#93194 = CARTESIAN_POINT ( 'NONE',  ( 28.81085032344271113, -286.9686574778456247, -239.4930102783042685 ) ) ;
#93195 = CARTESIAN_POINT ( 'NONE',  ( 31.76181859306231914, -276.7340999501711849, -244.7601130837306300 ) ) ;
#93196 = CARTESIAN_POINT ( 'NONE',  ( 32.10680081907952399, -291.9317833439520200, -297.8657594590737290 ) ) ;
#93197 = CARTESIAN_POINT ( 'NONE',  ( -104.8518433362911395, -297.9077449048450603, -300.8236596657920927 ) ) ;
#93198 = CARTESIAN_POINT ( 'NONE',  ( -11.12647552631010583, -275.4976091959406403, -338.9168799870798807 ) ) ;
#93199 = VERTEX_POINT ( 'NONE', #20677 ) ;
#93200 = CARTESIAN_POINT ( 'NONE',  ( 175.2296996224750103, 250.0000000000000568, 0.000000000000000000 ) ) ;
#93201 = CARTESIAN_POINT ( 'NONE',  ( -70.80251967740142049, -295.1481565284537965, -339.7017943972039120 ) ) ;
#93202 = CARTESIAN_POINT ( 'NONE',  ( 24.72336272961265990, -290.0318261111931974, -311.4848030009810600 ) ) ;
#93203 = CARTESIAN_POINT ( 'NONE',  ( -39.82724512258611327, -296.0207706036652553, -195.3991614904663834 ) ) ;
#93204 = CARTESIAN_POINT ( 'NONE',  ( 10.18782403219246291, -289.0279254370976787, -325.9693646830477292 ) ) ;
#93205 = ORIENTED_EDGE ( 'NONE', *, *, #82436, .F. ) ;
#93206 = CARTESIAN_POINT ( 'NONE',  ( -42.40253659557587440, -279.0485423625825661, -193.7634147053533979 ) ) ;
#93207 = CARTESIAN_POINT ( 'NONE',  ( -72.02063264983242163, -296.1500618565520995, -338.9955439375869446 ) ) ;
#93208 = CARTESIAN_POINT ( 'NONE',  ( -94.54158972101012637, -288.0092790155520106, -320.0448991685104829 ) ) ;
#93209 = CARTESIAN_POINT ( 'NONE',  ( -97.38827637270021853, -296.2396469624651445, -318.5499442493396032 ) ) ;
#93210 = CARTESIAN_POINT ( 'NONE',  ( 32.77166751017819735, -294.1557543438928519, -290.8071271024535349 ) ) ;
#93211 = DIRECTION ( 'NONE',  ( 1.000000000000000000, 0.000000000000000000, 0.000000000000000000 ) ) ;
#93212 = PRESENTATION_STYLE_ASSIGNMENT (( #19840 ) ) ;
#93213 = CARTESIAN_POINT ( 'NONE',  ( 199.9311642430735105, 312.1715086799357550, -9.103929867429124911 ) ) ;
#93214 = CARTESIAN_POINT ( 'NONE',  ( 23.29855873569807301, -288.4488359496038470, -224.0205176423681621 ) ) ;
#93215 = CARTESIAN_POINT ( 'NONE',  ( 108.6256185021308909, -297.2649936051623740, -190.4191791630918544 ) ) ;
#93216 = CARTESIAN_POINT ( 'NONE',  ( -99.34076080730291380, -278.5059570782535161, -224.8479177433979146 ) ) ;
#93217 = CARTESIAN_POINT ( 'NONE',  ( -90.17095008656997379, -285.8008580657005950, -323.4347564590783577 ) ) ;
#93218 = CARTESIAN_POINT ( 'NONE',  ( -40.77171308501063862, -284.5846698096116825, -193.9755741433193066 ) ) ;
#93219 = CARTESIAN_POINT ( 'NONE',  ( 36.88578273420901610, -285.7130431712475342, -276.6264036958883707 ) ) ;
#93220 = CARTESIAN_POINT ( 'NONE',  ( 33.04566781476661674, -277.7756270724763681, -298.5370105251740256 ) ) ;
#93221 = ORIENTED_EDGE ( 'NONE', *, *, #5681, .T. ) ;
#93223 = CARTESIAN_POINT ( 'NONE',  ( -87.59468463720851616, -278.6769310511675144, -217.2013385646314418 ) ) ;
#93222 = CARTESIAN_POINT ( 'NONE',  ( -87.09553140190301690, -277.7687916458238533, -323.7798064125101973 ) ) ;
#93224 = CARTESIAN_POINT ( 'NONE',  ( -31.29819022591435385, -275.2064340972066248, -193.8954962995532014 ) ) ;
#93225 = CARTESIAN_POINT ( 'NONE',  ( -112.6031698240258407, -277.5273917225454170, -256.0179914359422355 ) ) ;
#93226 = CARTESIAN_POINT ( 'NONE',  ( 191.7767904288494378, 277.8504399066188739, -124.6329446178930596 ) ) ;
#93227 = CARTESIAN_POINT ( 'NONE',  ( -95.85613748882796870, -274.1654335761859898, -220.6530411189235963 ) ) ;
#93228 = EDGE_CURVE ( 'NONE', #15791, #57748, #24956, .T. ) ;
#93229 = CARTESIAN_POINT ( 'NONE',  ( -34.09648980177933453, -299.5172960264183644, -193.9495737372290876 ) ) ;
#93230 = CARTESIAN_POINT ( 'NONE',  ( -110.4683760289727132, -281.2662352645559167, -253.7030783399848985 ) ) ;
#93231 = VERTEX_POINT ( 'NONE', #62854 ) ;
#93232 = CARTESIAN_POINT ( 'NONE',  ( 195.2846006655043425, -165.1985023605670619, -21.50000000000000000 ) ) ;
#93233 = CARTESIAN_POINT ( 'NONE',  ( -77.22873350587327934, -286.5835819542757577, -208.7927466873358355 ) ) ;
#93234 = CARTESIAN_POINT ( 'NONE',  ( -103.1738990033099412, -286.8133712669272768, -232.3078380909712166 ) ) ;
#93235 = CARTESIAN_POINT ( 'NONE',  ( 5.898248701612346601, -287.7971725074971232, -329.3665380403085123 ) ) ;
#93236 = CARTESIAN_POINT ( 'NONE',  ( -102.8689525709657033, -283.5324068435402296, -310.6811637466795446 ) ) ;
#93237 = CARTESIAN_POINT ( 'NONE',  ( -65.09831104353023079, -278.0831800794574633, -201.9797538079899653 ) ) ;
#93238 = CARTESIAN_POINT ( 'NONE',  ( 22.98168641837745696, -288.8168386370695089, -227.0083982521929613 ) ) ;
#93239 = CARTESIAN_POINT ( 'NONE',  ( 27.45557632168236495, -280.5064568608930244, -305.4612706237875273 ) ) ;
#93240 = CARTESIAN_POINT ( 'NONE',  ( -61.93920510712349170, -278.6937564520988531, -339.6698644878733830 ) ) ;
#93241 = CARTESIAN_POINT ( 'NONE',  ( 31.32174707990530749, -276.3786278270961816, -295.4745358232566446 ) ) ;
#93242 = CARTESIAN_POINT ( 'NONE',  ( -74.24954294168227875, -288.3264413884608643, -337.5014992780453440 ) ) ;
#93243 = CARTESIAN_POINT ( 'NONE',  ( 2.020217356878742265, -283.3420920574939714, -336.3520133569123800 ) ) ;
#93244 = CARTESIAN_POINT ( 'NONE',  ( -111.8138159825695226, -284.8018507506114361, -289.7376920111759091 ) ) ;
#93245 = CARTESIAN_POINT ( 'NONE',  ( 2.702210927790849926, -280.7721714879038473, -209.2637113911700055 ) ) ;
#93246 = ORIENTED_EDGE ( 'NONE', *, *, #49257, .T. ) ;
#93247 = EDGE_LOOP ( 'NONE', ( #91791, #32426, #7944, #76791 ) ) ;
#93248 = DIRECTION ( 'NONE',  ( 0.000000000000000000, 1.000000000000000000, 0.000000000000000000 ) ) ;
#93249 = CARTESIAN_POINT ( 'NONE',  ( -34.68600440572502919, -290.8795236966608400, -346.0793638883434937 ) ) ;
#93250 = CARTESIAN_POINT ( 'NONE',  ( -104.7295647735549835, -288.7656358596715904, -306.5850599277380297 ) ) ;
#93251 = CARTESIAN_POINT ( 'NONE',  ( -110.5765481139782196, -271.6469838737972964, -267.6165227046483892 ) ) ;
#93252 = CARTESIAN_POINT ( 'NONE',  ( -8.434063738488317696, -294.0322482892400444, -341.6752324797988081 ) ) ;
#93253 = CARTESIAN_POINT ( 'NONE',  ( -80.83214107322541508, -288.1339781007159786, -329.9165559745742939 ) ) ;
#93254 = CARTESIAN_POINT ( 'NONE',  ( 36.54783670435628551, -291.7257453472619204, -265.2686451037963593 ) ) ;
#93255 = CARTESIAN_POINT ( 'NONE',  ( 10.38504338120647752, -289.5814988634830343, -326.1893255028828662 ) ) ;
#93256 = CARTESIAN_POINT ( 'NONE',  ( -95.99890600148557951, -287.6948066931273615, -223.6242672951989618 ) ) ;
#93257 = CARTESIAN_POINT ( 'NONE',  ( -5.167333334178064064, -290.6288725286586327, -338.1233663568738734 ) ) ;
#93258 = CARTESIAN_POINT ( 'NONE',  ( -47.47051817817688146, -289.9236734089861898, -195.8274979675384770 ) ) ;
#93259 = CARTESIAN_POINT ( 'NONE',  ( -91.72135787159771780, -293.2776441320560252, -218.6364017236690813 ) ) ;
#93260 = CARTESIAN_POINT ( 'NONE',  ( -89.05196576053039337, -284.7421202252446619, -322.2922591787229294 ) ) ;
#93261 = CARTESIAN_POINT ( 'NONE',  ( 3.132385292289554979, -294.5941410494969546, -206.9600567826655322 ) ) ;
#93262 = DIRECTION ( 'NONE',  ( 0.000000000000000000, 1.000000000000000000, 0.000000000000000000 ) ) ;
#93263 = CARTESIAN_POINT ( 'NONE',  ( 197.2116943569230330, 275.5000000000000568, -12.92446933126074882 ) ) ;
#93264 = CARTESIAN_POINT ( 'NONE',  ( -80.33314189798755933, -275.4532652014053156, -208.4097262069114151 ) ) ;
#93265 = CARTESIAN_POINT ( 'NONE',  ( 10.00543177577010923, -281.5774892429994907, -326.2027343632244651 ) ) ;
#93266 = CARTESIAN_POINT ( 'NONE',  ( -109.6971933644954476, -282.2975897089835371, -290.1500638363548319 ) ) ;
#93267 = CARTESIAN_POINT ( 'NONE',  ( -72.01034808124663300, -294.6960513229583967, -338.9340256811822769 ) ) ;
#93268 = CARTESIAN_POINT ( 'NONE',  ( -31.23405102780345644, -272.3701744045952182, -196.5873909089060589 ) ) ;
#93269 = CARTESIAN_POINT ( 'NONE',  ( -72.35265904695719996, -275.5989812871129629, -336.0683205116607724 ) ) ;
#93270 = CARTESIAN_POINT ( 'NONE',  ( -108.4424471954553297, -297.6228236523456303, -289.0099496874532861 ) ) ;
#93271 = CARTESIAN_POINT ( 'NONE',  ( -69.86435409441874356, -272.2070019753833776, -201.2028845899655209 ) ) ;
#93272 = CARTESIAN_POINT ( 'NONE',  ( -55.93479655009908669, -296.7214404505634775, -341.6155472440119070 ) ) ;
#93273 = FACE_OUTER_BOUND ( 'NONE', #87403, .T. ) ;
#93274 = CARTESIAN_POINT ( 'NONE',  ( -68.12476745079561624, -298.4401372515159210, -203.9772147238924731 ) ) ;
#93275 = FACE_OUTER_BOUND ( 'NONE', #12412, .T. ) ;
#93277 = CARTESIAN_POINT ( 'NONE',  ( -52.63508903548208906, -297.8508622236386145, -198.9291775584406423 ) ) ;
#93276 = CARTESIAN_POINT ( 'NONE',  ( 4.292381753523367038, -284.6301468204551952, -207.4896404317160545 ) ) ;
#93278 = CARTESIAN_POINT ( 'NONE',  ( -33.72732828725057175, -286.0964577531777309, -193.4459938768536915 ) ) ;
#93279 = CARTESIAN_POINT ( 'NONE',  ( 37.48286012622866537, -287.4457620360851138, -288.5007465700223861 ) ) ;
#93280 = CARTESIAN_POINT ( 'NONE',  ( 14.36870489703889930, -296.3092717248750319, -325.1738976320864936 ) ) ;
#93281 = CARTESIAN_POINT ( 'NONE',  ( -6.491756904026782848, -290.4580877301786472, -202.1826064635637579 ) ) ;
#93282 = CARTESIAN_POINT ( 'NONE',  ( -31.07670702468217883, -279.3264374759253315, -193.7258460152913813 ) ) ;
#93283 = CARTESIAN_POINT ( 'NONE',  ( -20.25526795762938548, -292.3380690714490129, -345.3683826091709648 ) ) ;
#93284 = DIRECTION ( 'NONE',  ( -0.000000000000000000, -1.000000000000000000, -0.000000000000000000 ) ) ;
#93285 = CARTESIAN_POINT ( 'NONE',  ( -17.04743965292329477, -285.1148594994880909, -199.7723608643943578 ) ) ;
#93286 = EDGE_CURVE ( 'NONE', #1451, #20790, #32825, .T. ) ;
#93287 = CARTESIAN_POINT ( 'NONE',  ( 198.6673011211816515, 69.03676313268820763, -9.597248819411134946 ) ) ;
#93288 = CARTESIAN_POINT ( 'NONE',  ( 13.49318756761085858, -286.3408371416484215, -325.5752490717426326 ) ) ;
#93289 = CARTESIAN_POINT ( 'NONE',  ( -63.38060158658408483, -299.3074077254074155, -201.2533270183511149 ) ) ;
#93290 = CARTESIAN_POINT ( 'NONE',  ( -81.91000493751778322, -280.8831249738808538, -208.2944401444763969 ) ) ;
#93292 = CARTESIAN_POINT ( 'NONE',  ( 21.81193784710044525, -282.1508164467197730, -313.1592329575821623 ) ) ;
#93291 = CARTESIAN_POINT ( 'NONE',  ( -107.3509338238933708, -294.9352257619309512, -242.3442498308210418 ) ) ;
#93293 = CARTESIAN_POINT ( 'NONE',  ( -95.58010622918196475, -296.0383599629009268, -320.7326184498346606 ) ) ;
#93294 = CARTESIAN_POINT ( 'NONE',  ( 52.71383863060632535, -300.7196638740886101, -196.6439986017678336 ) ) ;
#93295 = CARTESIAN_POINT ( 'NONE',  ( 36.61912566161930727, -285.4341290740508157, -254.8351783483052202 ) ) ;
#93296 = ADVANCED_FACE ( 'NONE', ( #13579 ), #46090, .T. ) ;
#93297 = CARTESIAN_POINT ( 'NONE',  ( 34.67203289475921935, -283.2820090330147309, -249.3622583848950285 ) ) ;
#93298 = CARTESIAN_POINT ( 'NONE',  ( -109.1177205576019986, -295.4187948998850857, -284.9704867222752682 ) ) ;
#93299 = EDGE_LOOP ( 'NONE', ( #29534, #53965, #28033, #69603 ) ) ;
#93300 = FACE_OUTER_BOUND ( 'NONE', #56442, .T. ) ;
#93301 = CARTESIAN_POINT ( 'NONE',  ( -2.839196279003161738, -284.5737230785408656, -336.5677667542994413 ) ) ;
#93302 = DIRECTION ( 'NONE',  ( 0.000000000000000000, 0.000000000000000000, 1.000000000000000000 ) ) ;
#93303 = CARTESIAN_POINT ( 'NONE',  ( -110.4683760289727132, -293.8380690714490129, -287.0191576251351080 ) ) ;
#93304 = CARTESIAN_POINT ( 'NONE',  ( 39.46971532985821085, -274.7237430993175167, -268.3202173590611324 ) ) ;
#93305 = CARTESIAN_POINT ( 'NONE',  ( 34.21691060942654872, -293.1950517655050135, -255.9262562289091250 ) ) ;
#93306 = CARTESIAN_POINT ( 'NONE',  ( 35.01130376753191342, -282.8885804716250618, -256.3036385444580674 ) ) ;
#93307 = CARTESIAN_POINT ( 'NONE',  ( 34.28070615558948475, -276.9199999627544457, -252.5658563827510363 ) ) ;
#93308 = CARTESIAN_POINT ( 'NONE',  ( 22.78437203438852521, -283.7843979327710713, -317.1934895650267094 ) ) ;
#93309 = CARTESIAN_POINT ( 'NONE',  ( 33.84443509571659092, -280.1117888279570707, -252.4308431735550187 ) ) ;
#93310 = CARTESIAN_POINT ( 'NONE',  ( -111.6057779990163255, -280.6915240885984417, -259.5190959958131884 ) ) ;
#93311 = CARTESIAN_POINT ( 'NONE',  ( -35.47191091186855516, -298.0749566773375250, -193.3611179589730114 ) ) ;
#93312 = CARTESIAN_POINT ( 'NONE',  ( 39.63091839200972544, -275.3597932469244824, -268.3078272955459624 ) ) ;
#93313 = CARTESIAN_POINT ( 'NONE',  ( 36.26555900383650055, -295.6202948441273293, -281.8005251867387528 ) ) ;
#93314 = CARTESIAN_POINT ( 'NONE',  ( 201.6445761222588544, 62.92800856396105047, -6.999999999998341771 ) ) ;
#93315 = CARTESIAN_POINT ( 'NONE',  ( 200.9306832106270804, -199.2391364535880882, 0.000000000000000000 ) ) ;
#93316 = CARTESIAN_POINT ( 'NONE',  ( 37.38402868702716120, -291.8516765407208027, -282.9444184885438744 ) ) ;
#93317 = CARTESIAN_POINT ( 'NONE',  ( -85.34588000748786385, -272.8754448530427794, -215.2156834523604516 ) ) ;
#93318 = CARTESIAN_POINT ( 'NONE',  ( 36.79108678526437615, -295.3011602620046006, -288.5000327931616084 ) ) ;
#93319 = CARTESIAN_POINT ( 'NONE',  ( -44.87335835601073342, -293.1640258718359746, -194.0766977850057060 ) ) ;
#93320 = CARTESIAN_POINT ( 'NONE',  ( -74.43204382939174479, -291.5467401000939844, -335.3707720548350721 ) ) ;
#93321 = CARTESIAN_POINT ( 'NONE',  ( -110.6789582931641576, -276.7444154536066776, -255.4081223257527142 ) ) ;
#93322 = CARTESIAN_POINT ( 'NONE',  ( -8.151917034199209766, -278.5870405011910975, -338.8531802630988636 ) ) ;
#93323 = CARTESIAN_POINT ( 'NONE',  ( -23.27013289461709533, -292.9508071713839854, -343.5116525890737194 ) ) ;
#93324 = CARTESIAN_POINT ( 'NONE',  ( 29.61888168925902320, -282.9460514792619392, -234.8009771056352690 ) ) ;
#93325 = CARTESIAN_POINT ( 'NONE',  ( -57.46609736118185907, -284.7066698001199256, -199.8154861949709868 ) ) ;
#93326 = CARTESIAN_POINT ( 'NONE',  ( 27.36018454229470720, -24.35185690934844516, -343.9753583313619174 ) ) ;
#93327 = VERTEX_POINT ( 'NONE', #71341 ) ;
#93328 = CARTESIAN_POINT ( 'NONE',  ( -78.39201907150409454, -283.2884260675377845, -330.7511734665007452 ) ) ;
#93329 = CARTESIAN_POINT ( 'NONE',  ( -68.55933889872609655, -280.7311369922315407, -200.2971523889772243 ) ) ;
#93330 = CARTESIAN_POINT ( 'NONE',  ( -111.4944852100812227, -283.1047022657428442, -289.6322467330157338 ) ) ;
#93331 = CARTESIAN_POINT ( 'NONE',  ( -53.72199561105000498, -280.7882851932529888, -195.3100066458064248 ) ) ;
#93333 = CARTESIAN_POINT ( 'NONE',  ( -45.55556898334211979, -278.6744293241106902, -346.2769971086904093 ) ) ;
#93332 = B_SPLINE_CURVE_WITH_KNOTS ( 'NONE', 3,
 ( #83698, #90324, #55316, #18860, #47717, #46771, #19778, #84167, #76617, #40593, #69507, #82768, #4638, #33998, #33512, #47235 ),
 .UNSPECIFIED., .F., .F.,
 ( 4, 2, 2, 2, 2, 2, 2, 4 ),
 ( 0.000000000000000000, 0.0007636009008559850987, 0.001145401351284006108, 0.001527201801712027227, 0.001909002252140048128, 0.002290802702568069029, 0.002672603152996090147, 0.003054403603424111265 ),
 .UNSPECIFIED. ) ;
#93334 = CARTESIAN_POINT ( 'NONE',  ( 34.45848030099739390, -296.0519495502701943, -270.3284710469131937 ) ) ;
#93335 = ORIENTED_EDGE ( 'NONE', *, *, #34144, .T. ) ;
#93336 = ORIENTED_EDGE ( 'NONE', *, *, #54642, .F. ) ;
#93337 = CARTESIAN_POINT ( 'NONE',  ( -97.77667142547001333, -275.1561204509398522, -226.1428834626578066 ) ) ;
#93338 = CARTESIAN_POINT ( 'NONE',  ( -35.59969422421068685, -278.0941927101180795, -195.7239614331422786 ) ) ;
#93339 = CARTESIAN_POINT ( 'NONE',  ( -111.8696634739424098, -292.1236695618717931, -285.2444201393055891 ) ) ;
#93340 = CARTESIAN_POINT ( 'NONE',  ( 12.41819523943533632, -293.6858028803654292, -323.9827584333213508 ) ) ;
#93341 = CARTESIAN_POINT ( 'NONE',  ( -38.92519833999234891, -288.5791756989824535, -347.2832827784969822 ) ) ;
#93342 = CARTESIAN_POINT ( 'NONE',  ( 196.8803347170859865, 42.36571313990103249, 12.49999999999999289 ) ) ;
#93344 = CARTESIAN_POINT ( 'NONE',  ( -49.53384484530918286, -284.2941206061042863, -197.5231245158441311 ) ) ;
#93343 = CARTESIAN_POINT ( 'NONE',  ( 29.05361676038690177, -292.6230298726919159, -308.2868464497824448 ) ) ;
#93345 = CARTESIAN_POINT ( 'NONE',  ( -41.68845706475383395, -293.8573768313712549, -196.2025939599754736 ) ) ;
#93346 = CARTESIAN_POINT ( 'NONE',  ( 18.31239808476545150, -285.3499201719639018, -222.0565725876165288 ) ) ;
#93347 = CARTESIAN_POINT ( 'NONE',  ( 24.55476209715605052, -283.4128955366576292, -310.0788312290978865 ) ) ;
#93348 = CARTESIAN_POINT ( 'NONE',  ( -113.4345562563489551, -291.6254167333763689, -259.8375318194370607 ) ) ;
#93349 = CARTESIAN_POINT ( 'NONE',  ( 19.72015016035604873, -281.4004084286986540, -224.7329064950718305 ) ) ;
#93350 = CARTESIAN_POINT ( 'NONE',  ( 36.70877110848037717, -292.5938523750085665, -289.9707184176549504 ) ) ;
#93351 = CARTESIAN_POINT ( 'NONE',  ( 37.95210925836853733, -288.5471032869760393, -285.6908632237289680 ) ) ;
#93352 = CARTESIAN_POINT ( 'NONE',  ( -28.97763250525009227, -289.4413137809881960, -346.8970783663022530 ) ) ;
#93353 = CARTESIAN_POINT ( 'NONE',  ( -4.596464110547775483, -286.6627916813097272, -205.1173479911695097 ) ) ;
#93354 = VERTEX_POINT ( 'NONE', #55497 ) ;
#93355 = CARTESIAN_POINT ( 'NONE',  ( 194.7518928364593478, 26.86155445384702034, 13.97733162193927114 ) ) ;
#93356 = CARTESIAN_POINT ( 'NONE',  ( 37.39189077831895247, -295.5719075428073666, -282.8976365775211548 ) ) ;
#93357 = CARTESIAN_POINT ( 'NONE',  ( -94.29573271656752809, -294.5392684802084773, -321.4642638720558807 ) ) ;
#93358 = CARTESIAN_POINT ( 'NONE',  ( -101.0104740308733966, -278.1049622890552087, -234.1714001431494410 ) ) ;
#93359 = CARTESIAN_POINT ( 'NONE',  ( -109.1069308216474667, -272.4130725769809942, -242.4786282469997616 ) ) ;
#93360 = CARTESIAN_POINT ( 'NONE',  ( 10.72929207825920273, -292.8531278653502454, -326.2170707445384323 ) ) ;
#93361 = CARTESIAN_POINT ( 'NONE',  ( 8.221610683803218578, -278.1796416044845159, -328.7527519124992637 ) ) ;
#93362 = CARTESIAN_POINT ( 'NONE',  ( -49.04723166040062665, -272.0411600202263003, -197.0025594693185553 ) ) ;
#93363 = B_SPLINE_CURVE_WITH_KNOTS ( 'NONE', 3,
 ( #43081, #63952, #57763, #92791, #43538, #56849, #7552, #20837, #20378, #87083, #49706, #49249, #13745, #85690, #42594, #86609 ),
 .UNSPECIFIED., .F., .F.,
 ( 4, 2, 2, 2, 2, 2, 2, 4 ),
 ( 0.6790892544725759539, 0.7192030976635021000, 0.7593169408544281351, 0.7994307840453542813, 0.8395446272362804274, 0.8796584704272065736, 0.9197723136181326087, 1.000000000000000000 ),
 .UNSPECIFIED. ) ;
#93364 = CARTESIAN_POINT ( 'NONE',  ( 30.96068055187923562, -295.1162384671271184, -297.3687305822743951 ) ) ;
#93365 = CARTESIAN_POINT ( 'NONE',  ( -101.7322937367429603, -297.1555027337522006, -305.4050550830162365 ) ) ;
#93366 = CARTESIAN_POINT ( 'NONE',  ( -43.27403345252375289, -275.1145486516829237, -431.5602653418008003 ) ) ;
#93367 = CARTESIAN_POINT ( 'NONE',  ( -79.57341909547156433, -295.4833137061534103, -208.1172801465939983 ) ) ;
#93368 = CARTESIAN_POINT ( 'NONE',  ( -54.58039129470394357, -298.4876434721509213, -195.4202058375244633 ) ) ;
#93369 = CARTESIAN_POINT ( 'NONE',  ( 29.95662235446795307, -286.5258288642655202, -300.2584461071188002 ) ) ;
#93370 = CARTESIAN_POINT ( 'NONE',  ( -109.8808681630931119, -274.7995226287691253, -251.1073299375090073 ) ) ;
#93371 = CARTESIAN_POINT ( 'NONE',  ( -72.46119749723085590, -290.4704361033876694, -334.6264224092256541 ) ) ;
#93372 = CARTESIAN_POINT ( 'NONE',  ( -88.00056946223183729, -273.8583572385398384, -212.3834080900900858 ) ) ;
#93373 = CARTESIAN_POINT ( 'NONE',  ( -71.67869562670523464, -297.9185484927414791, -205.9026899569780085 ) ) ;
#93374 = CARTESIAN_POINT ( 'NONE',  ( -108.9937543560073578, -280.8338736804565201, -246.8631647424808193 ) ) ;
#93375 = CARTESIAN_POINT ( 'NONE',  ( 37.50573183366711305, -280.0367153198178585, -254.4503454605764432 ) ) ;
#93376 = ORIENTED_EDGE ( 'NONE', *, *, #54119, .T. ) ;
#93377 = CARTESIAN_POINT ( 'NONE',  ( -65.22297454738438205, -282.7556847950644396, -342.0408276124356917 ) ) ;
#93378 = CARTESIAN_POINT ( 'NONE',  ( 16.87746370896037718, -275.6533848292824587, -324.9661437295197857 ) ) ;
#93379 = CARTESIAN_POINT ( 'NONE',  ( -19.91912720295708183, -278.6722086477174685, -196.1254167293053001 ) ) ;
#93380 = CARTESIAN_POINT ( 'NONE',  ( -53.34471614677429585, -277.8473460212447321, -196.8644592883882751 ) ) ;
#93381 = CARTESIAN_POINT ( 'NONE',  ( -109.7057917503941837, -271.3054263375146320, -256.7167939506281868 ) ) ;
#93382 = CARTESIAN_POINT ( 'NONE',  ( 19.54902106401569029, -278.2297495938773864, -319.2522849109691379 ) ) ;
#93383 = CARTESIAN_POINT ( 'NONE',  ( 169.2494399300530290, 8.542400036368780647, 9.000000000000001776 ) ) ;
#93384 = CARTESIAN_POINT ( 'NONE',  ( 25.14345832407315839, -291.0041463908388550, -228.1502657429280134 ) ) ;
#93385 = CARTESIAN_POINT ( 'NONE',  ( -106.0041104324170220, -291.0021413791034774, -235.3942584584674762 ) ) ;
#93386 = CARTESIAN_POINT ( 'NONE',  ( 27.52695381552508991, -278.0586348456372434, -308.3359275282518297 ) ) ;
#93387 = CARTESIAN_POINT ( 'NONE',  ( -109.1029005865617307, -270.8350489111158481, -248.3813384008189757 ) ) ;
#93388 = CARTESIAN_POINT ( 'NONE',  ( -33.72468060359333464, -285.2937548822400800, -193.6077728402057403 ) ) ;
#93389 = FACE_OUTER_BOUND ( 'NONE', #77177, .T. ) ;
#93390 = FACE_OUTER_BOUND ( 'NONE', #14139, .T. ) ;
#93391 = CARTESIAN_POINT ( 'NONE',  ( -97.91278823630773331, -283.1550164924902333, -226.1114543003701840 ) ) ;
#93392 = LINE ( 'NONE', #56978, #63363 ) ;
#93393 = CARTESIAN_POINT ( 'NONE',  ( 35.81900950809895079, -292.4242918366943513, -276.2467844365119731 ) ) ;
#93394 = CARTESIAN_POINT ( 'NONE',  ( 32.13892928045079600, -285.3470132185835269, -244.0757299866895664 ) ) ;
#93395 = FACE_OUTER_BOUND ( 'NONE', #19491, .T. ) ;
#93396 = CARTESIAN_POINT ( 'NONE',  ( 159.0442047513579951, 16.98551211945800432, -9.330684800570146820 ) ) ;
#93397 = CARTESIAN_POINT ( 'NONE',  ( -74.30981107682269737, -293.5435474178731852, -335.6172243832690469 ) ) ;
#93398 = CARTESIAN_POINT ( 'NONE',  ( -102.3377423507916859, -282.5047976998575905, -310.3388898952244972 ) ) ;
#93399 = CARTESIAN_POINT ( 'NONE',  ( -102.8755574070748793, -280.6101255035393933, -236.3123390918978544 ) ) ;
#93400 = CARTESIAN_POINT ( 'NONE',  ( -35.17492549822232917, -287.2838279302326328, -193.7757638536210720 ) ) ;
#93401 = CARTESIAN_POINT ( 'NONE',  ( -1.592100343325223877, -278.7592742957497762, -203.3093459649720671 ) ) ;
#93402 = CARTESIAN_POINT ( 'NONE',  ( 29.42505706653262365, -287.9508718134921423, -300.0026327109038675 ) ) ;
#93403 = CARTESIAN_POINT ( 'NONE',  ( -71.91508889801768589, -278.9438669585422303, -335.3372857805192666 ) ) ;
#93404 = CARTESIAN_POINT ( 'NONE',  ( -103.2721016708898532, -278.9254593197376266, -302.1924037059603165 ) ) ;
#93405 = CARTESIAN_POINT ( 'NONE',  ( -107.5064108168476338, -286.8896419441156240, -242.7359989365525905 ) ) ;
#93406 = ORIENTED_EDGE ( 'NONE', *, *, #73224, .T. ) ;
#93407 = CARTESIAN_POINT ( 'NONE',  ( -37.60553200451163747, -297.8822550093572659, -193.3615699496105265 ) ) ;
#93408 = CARTESIAN_POINT ( 'NONE',  ( 34.67537222130464869, -289.7879136342854736, -290.1844754086752687 ) ) ;
#93409 = CARTESIAN_POINT ( 'NONE',  ( 183.0442525570908288, 300.2961574867697436, 4.888549259831427740 ) ) ;
#93410 = CARTESIAN_POINT ( 'NONE',  ( -37.30987171927208124, -285.5519495502701375, -350.3611179825600175 ) ) ;
#93411 = ORIENTED_EDGE ( 'NONE', *, *, #3118, .T. ) ;
#93412 = CARTESIAN_POINT ( 'NONE',  ( -31.37946563810588430, -272.1270991627338276, -195.4183176735483016 ) ) ;
#93413 = CARTESIAN_POINT ( 'NONE',  ( 19.79250794923519052, -291.2619682345053320, -219.9219310330756230 ) ) ;
#93414 = CARTESIAN_POINT ( 'NONE',  ( -66.08311528030476723, -294.9464099139960354, -337.5319412381646202 ) ) ;
#93415 = CARTESIAN_POINT ( 'NONE',  ( -6.746146657060896779, -287.9813622172252963, -203.3053366861183520 ) ) ;
#93416 = CARTESIAN_POINT ( 'NONE',  ( -6.365495103167028823, -282.2248403249021749, -203.1278769479647224 ) ) ;
#93417 = CARTESIAN_POINT ( 'NONE',  ( -4.569199117443258018, -290.0540774315262524, -339.4013495191113634 ) ) ;
#93418 = CARTESIAN_POINT ( 'NONE',  ( -29.01410460794515700, -290.2640079778120707, -346.4665827955946042 ) ) ;
#93419 = CARTESIAN_POINT ( 'NONE',  ( -90.28865002906135828, -285.8008580650235899, -323.5529205773983108 ) ) ;
#93420 = CARTESIAN_POINT ( 'NONE',  ( -71.56894305999588823, -277.6585219453281184, -339.3357208869135206 ) ) ;
#93421 = VERTEX_POINT ( 'NONE', #18557 ) ;
#93422 = CARTESIAN_POINT ( 'NONE',  ( 36.93707770848498484, -291.8094766409882936, -284.2864993430272307 ) ) ;
#93423 = CARTESIAN_POINT ( 'NONE',  ( 3.823765122875361300, -280.4229418822373532, -205.2258335575434103 ) ) ;
#93424 = CARTESIAN_POINT ( 'NONE',  ( -109.1407697003461124, -274.6598007323320871, -251.3021906120513904 ) ) ;
#93425 = CARTESIAN_POINT ( 'NONE',  ( -4.829096099716510437, -294.9805209788416391, -202.7746430608542312 ) ) ;
#93426 = CARTESIAN_POINT ( 'NONE',  ( 16.22477106298412508, -274.5448354871925858, -324.3289756100926411 ) ) ;
#93427 = FACE_OUTER_BOUND ( 'NONE', #3090, .T. ) ;
#93428 = CARTESIAN_POINT ( 'NONE',  ( -43.75024467819104501, -279.4767736568892360, -197.5309062623671252 ) ) ;
#93429 = CARTESIAN_POINT ( 'NONE',  ( 35.68873695956158798, -277.0493261069672712, -293.4817576209982235 ) ) ;
#93430 = CARTESIAN_POINT ( 'NONE',  ( -36.49290927759641789, -299.4882554922018016, -196.7716739771189793 ) ) ;
#93431 = CARTESIAN_POINT ( 'NONE',  ( -18.98631019523740804, -281.8803485584491000, -344.9538147036035411 ) ) ;
#93432 = CARTESIAN_POINT ( 'NONE',  ( -102.0199626533828337, -292.7987792331045966, -234.2739070329792810 ) ) ;
#93433 = CARTESIAN_POINT ( 'NONE',  ( -69.80961249357252996, -275.2319125000711892, -201.4101059853202855 ) ) ;
#93434 = CARTESIAN_POINT ( 'NONE',  ( -58.00463181270065149, -275.1059523535773224, -196.6423389768230265 ) ) ;
#93435 = CARTESIAN_POINT ( 'NONE',  ( 37.45292602031227602, -295.5213466841288437, -267.9543934762687059 ) ) ;
#93436 = CARTESIAN_POINT ( 'NONE',  ( -48.62974823152696757, -281.1960574144940210, -344.3381981781935792 ) ) ;
#93437 = CARTESIAN_POINT ( 'NONE',  ( -112.8480888415426762, -290.0305856769971342, -285.4122601950525677 ) ) ;
#93438 = CARTESIAN_POINT ( 'NONE',  ( 35.99407092260890551, -273.3927036144502267, -256.4430904783872620 ) ) ;
#93439 = CARTESIAN_POINT ( 'NONE',  ( -33.78526479030544039, -287.6963276090850741, -194.2441541422848275 ) ) ;
#93440 = CARTESIAN_POINT ( 'NONE',  ( -109.4855542413283160, -289.3014611403405070, -283.3799653929628448 ) ) ;
#93441 = ORIENTED_EDGE ( 'NONE', *, *, #41040, .T. ) ;
#93442 = CARTESIAN_POINT ( 'NONE',  ( -101.1816048158095072, -289.6842194989674795, -228.2772408569960874 ) ) ;
#93443 = CARTESIAN_POINT ( 'NONE',  ( -97.36870871009104178, -289.6394715030056659, -311.9624778839516352 ) ) ;
#93444 = ORIENTED_EDGE ( 'NONE', *, *, #19910, .F. ) ;
#93445 = CARTESIAN_POINT ( 'NONE',  ( -3.637656833744716156, -287.5661836699939045, -201.4588427515063813 ) ) ;
#93446 = CARTESIAN_POINT ( 'NONE',  ( -74.02022723481208288, -277.8872971944346659, -333.5020170581052525 ) ) ;
#93447 = CARTESIAN_POINT ( 'NONE',  ( -4.723082304384085717, -291.3921507254633525, -200.9527735095904291 ) ) ;
#93448 = CARTESIAN_POINT ( 'NONE',  ( -96.18694882895684373, -284.5358883346564767, -319.8845140957773765 ) ) ;
#93449 = CARTESIAN_POINT ( 'NONE',  ( -113.5778257278640950, -284.7472744917134833, -281.4050597008513819 ) ) ;
#93450 = CARTESIAN_POINT ( 'NONE',  ( -5.553124193766756811, -280.8155175398274537, -204.6224389043356382 ) ) ;
#93451 = CARTESIAN_POINT ( 'NONE',  ( -113.8400438337849607, -273.7182392849545067, -284.1715810343901580 ) ) ;
#93452 = CARTESIAN_POINT ( 'NONE',  ( 184.2263671677063712, 263.6655576831765870, -152.9503626755218590 ) ) ;
#93453 = CARTESIAN_POINT ( 'NONE',  ( 183.3501064672990992, 261.6236131564620564, -151.2791749291968415 ) ) ;
#93454 = CARTESIAN_POINT ( 'NONE',  ( -54.23893091208370265, -273.0266867937696702, -199.1776555895956733 ) ) ;
#93455 = CARTESIAN_POINT ( 'NONE',  ( -24.52894948609698744, -273.1397102019383851, -198.1285675201764604 ) ) ;
#93456 = CARTESIAN_POINT ( 'NONE',  ( -8.416994874107269098, -294.1912886284904971, -341.7119300439276230 ) ) ;
#93457 = CARTESIAN_POINT ( 'NONE',  ( 199.6417264645343721, 285.7069599252702119, -96.38872539580104615 ) ) ;
#93458 = EDGE_CURVE ( 'NONE', #59451, #42812, #46038, .T. ) ;
#93459 = CARTESIAN_POINT ( 'NONE',  ( -85.48484136407371636, -272.0869869860615609, -210.9007427453300068 ) ) ;
#93460 = CARTESIAN_POINT ( 'NONE',  ( -71.04922905380782083, -299.4629144823082925, -204.2056963206571254 ) ) ;
#93461 = ADVANCED_FACE ( 'NONE', ( #46495 ), #35576, .F. ) ;
#93462 = CARTESIAN_POINT ( 'NONE',  ( -23.67716697703319539, -290.1891895229061333, -342.6248294923580602 ) ) ;
#93463 = CARTESIAN_POINT ( 'NONE',  ( -28.08087035673225884, -293.2519975431939088, -197.5883353551120649 ) ) ;
#93464 = ORIENTED_EDGE ( 'NONE', *, *, #62997, .F. ) ;
#93465 = CARTESIAN_POINT ( 'NONE',  ( -95.40103107510299196, -298.1745132989731815, -220.0629045682121330 ) ) ;
#93466 = CARTESIAN_POINT ( 'NONE',  ( -44.03625157419021718, -286.4575748318908950, -197.6069330679039808 ) ) ;
#93467 = CARTESIAN_POINT ( 'NONE',  ( 34.30462442122028222, -294.7074852069557664, -298.1273384436191805 ) ) ;
#93468 = CARTESIAN_POINT ( 'NONE',  ( -32.01050979066527447, -295.4789650893886801, -347.1278980988841454 ) ) ;
#93469 = CARTESIAN_POINT ( 'NONE',  ( 35.70799734060722130, -293.7240662909975981, -270.7578046560553844 ) ) ;
#93470 = EDGE_LOOP ( 'NONE', ( #68909, #4601, #3435 ) ) ;
#93471 = CARTESIAN_POINT ( 'NONE',  ( -49.51186359494247569, -275.8184430987686824, -195.7348543296051560 ) ) ;
#93472 = ORIENTED_EDGE ( 'NONE', *, *, #67295, .T. ) ;
#93473 = CARTESIAN_POINT ( 'NONE',  ( -113.0062548877486819, -277.8843872511916402, -284.3763473865262199 ) ) ;
#93474 = AXIS2_PLACEMENT_3D ( 'NONE', #84536, #48552, #20637 ) ;
#93475 = CARTESIAN_POINT ( 'NONE',  ( -24.43672847221546363, -272.6193369866017520, -197.6460266796819667 ) ) ;
#93476 = CARTESIAN_POINT ( 'NONE',  ( -34.47575232296714631, -299.2938913470392208, -196.9634389370661438 ) ) ;
#93477 = CARTESIAN_POINT ( 'NONE',  ( 20.86125389797872387, -275.8700475353944626, -225.8902316055917368 ) ) ;
#93478 = CARTESIAN_POINT ( 'NONE',  ( 1.875567058276114585, -276.3294536600010360, -205.2767114963382085 ) ) ;
#93479 = CARTESIAN_POINT ( 'NONE',  ( 4.927374798749446505, -274.5041390199899070, -332.7448667114337582 ) ) ;
#93480 = CARTESIAN_POINT ( 'NONE',  ( -23.49140382440393182, -295.5219606246382682, -342.1906606054416216 ) ) ;
#93481 = CARTESIAN_POINT ( 'NONE',  ( 10.66227604733319900, -292.9479622675751784, -326.1373959769626936 ) ) ;
#93482 = CARTESIAN_POINT ( 'NONE',  ( 209.7513585654922679, 305.7026273589066818, -40.00000000000000711 ) ) ;
#93483 = CARTESIAN_POINT ( 'NONE',  ( -113.9831947762480411, -279.1363068300817645, -263.0260339418780973 ) ) ;
#93484 = CARTESIAN_POINT ( 'NONE',  ( -27.01941584524472617, -277.0839261023417635, -342.6276417101828997 ) ) ;
#93485 = CARTESIAN_POINT ( 'NONE',  ( -52.06188809211826651, -284.5524896018435470, -195.2296895823323268 ) ) ;
#93486 = CARTESIAN_POINT ( 'NONE',  ( -95.93368542694700807, -299.1986782260334508, -223.2760068522333938 ) ) ;
#93487 = CARTESIAN_POINT ( 'NONE',  ( 82.63238957975535470, -300.8510545236958365, -197.5047496147394668 ) ) ;
#93488 = CARTESIAN_POINT ( 'NONE',  ( 18.79221964301244796, -286.0846147172247811, -223.4205486067389472 ) ) ;
#93489 = CARTESIAN_POINT ( 'NONE',  ( -30.14180374065835721, -278.3842034294286805, -196.6477564345687483 ) ) ;
#93490 = CARTESIAN_POINT ( 'NONE',  ( -108.1806289176360139, -277.3887685684745179, -250.3840498241575858 ) ) ;
#93491 = CARTESIAN_POINT ( 'NONE',  ( -101.3259944083016251, -286.0264186511553248, -309.5874242818709376 ) ) ;
#93492 = CARTESIAN_POINT ( 'NONE',  ( -16.25217542377819058, -277.9785904355476305, -340.7163565289692428 ) ) ;
#93493 = DIRECTION ( 'NONE',  ( 1.000000000000000000, 0.000000000000000000, -0.000000000000000000 ) ) ;
#93494 = CARTESIAN_POINT ( 'NONE',  ( 19.45336154821961117, -273.2551532189198156, -219.4823559655316387 ) ) ;
#93495 = CARTESIAN_POINT ( 'NONE',  ( 19.07223262217143400, -275.5456024874844161, -223.8706796087952284 ) ) ;
#93496 = CARTESIAN_POINT ( 'NONE',  ( 24.43838321705250394, -284.1319473700785920, -313.2002312222252272 ) ) ;
#93497 = LINE ( 'NONE', #64207, #42897 ) ;
#93498 = CARTESIAN_POINT ( 'NONE',  ( 36.60903307437060761, -289.2738158650947753, -254.7871740450747780 ) ) ;
#93499 = CARTESIAN_POINT ( 'NONE',  ( 31.14616550503944481, -291.9540899036791757, -301.0551009103980391 ) ) ;
#93500 = CARTESIAN_POINT ( 'NONE',  ( 15.81498358983247243, -273.5091739102238080, -219.5369595236599025 ) ) ;
#93501 = CARTESIAN_POINT ( 'NONE',  ( 7.439904419314146367, -290.8098961646625753, -211.1540797886869427 ) ) ;
#93502 = CARTESIAN_POINT ( 'NONE',  ( 9.093980818847771985, -59.61193948127866094, -357.4272672779520121 ) ) ;
#93503 = CARTESIAN_POINT ( 'NONE',  ( 197.8479349096537874, 68.18631839859101262, -11.29146348611214812 ) ) ;
#93504 = CARTESIAN_POINT ( 'NONE',  ( -89.03612589067078886, -288.2433002536640743, -326.4894895635828220 ) ) ;
#93505 = CARTESIAN_POINT ( 'NONE',  ( 37.11086761422676261, -285.9845440276463364, -285.5528648548295223 ) ) ;
#93506 = CARTESIAN_POINT ( 'NONE',  ( -33.44703475892746525, -284.4274772773545692, -343.8598892607020616 ) ) ;
#93507 = CARTESIAN_POINT ( 'NONE',  ( -70.27848341858285153, -284.3005485007004722, -335.7032985130510951 ) ) ;
#93508 = CARTESIAN_POINT ( 'NONE',  ( -111.5565891034642618, -292.6989374988067993, -257.3013684094283349 ) ) ;
#93509 = CARTESIAN_POINT ( 'NONE',  ( -13.07317647120376236, -274.6923430022641810, -197.3078288643833673 ) ) ;
#93510 = CARTESIAN_POINT ( 'NONE',  ( -111.7202454524117599, -288.4614405482430470, -283.7439582797645699 ) ) ;
#93511 = CARTESIAN_POINT ( 'NONE',  ( -65.09507202992548969, -277.4047905908148550, -342.2418452433019525 ) ) ;
#93512 = CARTESIAN_POINT ( 'NONE',  ( 36.09695971889733102, -295.3587144492655057, -256.9256658754217710 ) ) ;
#93513 = DIRECTION ( 'NONE',  ( -1.224646799147353207E-16, 1.000000000000000000, 0.000000000000000000 ) ) ;
#93514 = CARTESIAN_POINT ( 'NONE',  ( -37.37352853689063892, -300.5519495502701943, -195.3611179825600175 ) ) ;
#93515 = CARTESIAN_POINT ( 'NONE',  ( -108.5019930357738929, -283.4778503710252267, -251.9911372384626702 ) ) ;
#93516 = CARTESIAN_POINT ( 'NONE',  ( -83.32021553195014008, -277.4224509290582432, -211.0419171283040498 ) ) ;
#93517 = CARTESIAN_POINT ( 'NONE',  ( -20.70664710831266575, -296.6570049833844109, -194.1655527349372790 ) ) ;
#93518 = CARTESIAN_POINT ( 'NONE',  ( 32.61152168340876045, -275.1818891360526322, -291.6280526748131479 ) ) ;
#93519 = CARTESIAN_POINT ( 'NONE',  ( 34.62271883042186715, -294.8641433517653354, -254.4336790149428964 ) ) ;
#93520 = CARTESIAN_POINT ( 'NONE',  ( 19.52092451065522738, -293.8422999169034711, -224.1888196464184091 ) ) ;
#93521 = CARTESIAN_POINT ( 'NONE',  ( -79.19310707031579000, -296.9194207817747611, -334.4060866286340001 ) ) ;
#93522 = CARTESIAN_POINT ( 'NONE',  ( -102.5313784318425547, -296.8327218276427857, -237.3957819845661845 ) ) ;
#93523 = CARTESIAN_POINT ( 'NONE',  ( -104.6288388657776096, -292.1153715057439513, -303.4887741950014970 ) ) ;
#93524 = CARTESIAN_POINT ( 'NONE',  ( -35.89706682933255877, -283.2012159406257297, -347.3606820246671987 ) ) ;
#93525 = CARTESIAN_POINT ( 'NONE',  ( -24.34776320107464542, -272.3557753154875058, -195.6655839070433842 ) ) ;
#93526 = CARTESIAN_POINT ( 'NONE',  ( -23.78381967985747281, -286.0539782724353017, -194.5099096889770749 ) ) ;
#93527 = CARTESIAN_POINT ( 'NONE',  ( -13.23078674303616786, -278.7174624458370431, -341.0590070258358537 ) ) ;
#93528 = CARTESIAN_POINT ( 'NONE',  ( -60.04021353905203995, -284.8093570205584228, -200.7322020304045793 ) ) ;
#93529 = CIRCLE ( 'NONE', #90457, 4.999999999999993783 ) ;
#93530 = CARTESIAN_POINT ( 'NONE',  ( -69.79726493871461912, -287.4792636347085590, -337.9891108120561967 ) ) ;
#93531 = CARTESIAN_POINT ( 'NONE',  ( -96.00709874043252512, -235.9016261432062720, -336.2420922186948928 ) ) ;
#93532 = CARTESIAN_POINT ( 'NONE',  ( -44.02376733478919135, -285.4730392650935187, -197.6057853978923902 ) ) ;
#93533 = CARTESIAN_POINT ( 'NONE',  ( 38.39974831866283012, -282.6088882822317032, -258.5614584936393499 ) ) ;
#93534 = CARTESIAN_POINT ( 'NONE',  ( -46.01114062161299501, -288.2181544786747622, -346.6876758869118476 ) ) ;
#93535 = CARTESIAN_POINT ( 'NONE',  ( -111.3142789937868287, -280.3840882004795390, -252.0182382870230811 ) ) ;
#93536 = CARTESIAN_POINT ( 'NONE',  ( -107.1194078006392090, -279.4625646259284508, -301.8646329476553092 ) ) ;
#93537 = CARTESIAN_POINT ( 'NONE',  ( -97.99242448250743109, -278.9508199391234484, -229.6451445622688823 ) ) ;
#93538 = CARTESIAN_POINT ( 'NONE',  ( -86.40994850451242826, -275.3472863608535590, -214.0413950332018089 ) ) ;
#93539 = CARTESIAN_POINT ( 'NONE',  ( 29.57466943630001310, -294.0480726856487195, -308.5634403922383626 ) ) ;
#93540 = CARTESIAN_POINT ( 'NONE',  ( -26.25494551295901147, -286.9305839336622057, -344.2301885035767555 ) ) ;
#93541 = CARTESIAN_POINT ( 'NONE',  ( -11.44450386862733815, -293.9839521229195043, -198.6413428907675041 ) ) ;
#93542 = CARTESIAN_POINT ( 'NONE',  ( -110.1130621978689987, -295.3507015472331432, -279.6313503302699814 ) ) ;
#93543 = CARTESIAN_POINT ( 'NONE',  ( 32.71801444650724733, -283.8026522964962624, -295.6721755190951058 ) ) ;
#93544 = CARTESIAN_POINT ( 'NONE',  ( -90.42552444425373892, -295.4961676496943710, -320.5756916301675687 ) ) ;
#93545 = CARTESIAN_POINT ( 'NONE',  ( -30.73764706975871519, -293.2133162436821863, -193.9025573788531744 ) ) ;
#93546 = CARTESIAN_POINT ( 'NONE',  ( -14.28458138705839353, -281.0104726537849729, -200.9371374457803654 ) ) ;
#93547 = EDGE_CURVE ( 'NONE', #21018, #4210, #10647, .T. ) ;
#93548 = CARTESIAN_POINT ( 'NONE',  ( 38.69277641733815187, -274.4783923215439927, -259.7980412844152056 ) ) ;
#93549 = CARTESIAN_POINT ( 'NONE',  ( -109.7667428805340819, -290.8751381530061053, -296.3631973658353331 ) ) ;
#93550 = CARTESIAN_POINT ( 'NONE',  ( -73.70433059592032521, -281.6687339992516286, -336.8881869333473560 ) ) ;
#93551 = CARTESIAN_POINT ( 'NONE',  ( -102.2811402926141682, -290.3423449120315922, -311.7945792808152419 ) ) ;
#93552 = CARTESIAN_POINT ( 'NONE',  ( -10.71243403179295939, -289.0284593315242887, -338.4077746162614631 ) ) ;
#93553 = DIRECTION ( 'NONE',  ( -0.000000000000000000, 1.000000000000000000, -0.000000000000000000 ) ) ;
#93554 = CARTESIAN_POINT ( 'NONE',  ( 183.3530210459282443, 262.9716507355972226, -152.1700128130211453 ) ) ;
#93555 = CARTESIAN_POINT ( 'NONE',  ( 184.7455544834175498, 260.4446745686637996, -151.0159784568642181 ) ) ;
#93556 = CARTESIAN_POINT ( 'NONE',  ( 35.78497577281001440, -272.8380690714490129, -253.7030783399848985 ) ) ;
#93557 = CARTESIAN_POINT ( 'NONE',  ( -108.9248828707205945, -277.5503714635711390, -285.4756697762999238 ) ) ;
#93558 = ORIENTED_EDGE ( 'NONE', *, *, #18309, .T. ) ;
#93559 = CARTESIAN_POINT ( 'NONE',  ( -32.93073481843851624, -279.0293548781060622, -197.1848277031661212 ) ) ;
#93560 = CARTESIAN_POINT ( 'NONE',  ( 1.188515487324648179, -274.2186665256807032, -203.7037570244632150 ) ) ;
#93561 = CARTESIAN_POINT ( 'NONE',  ( 181.1745638653161166, 251.2302727232378459, -164.9768912459212231 ) ) ;
#93562 = EDGE_CURVE ( 'NONE', #71446, #26935, #69226, .T. ) ;
#93563 = CARTESIAN_POINT ( 'NONE',  ( -61.84139018168271917, -278.3147013432948143, -197.9287258956971698 ) ) ;
#93564 = CARTESIAN_POINT ( 'NONE',  ( -94.70183077768534474, -281.9094567301834218, -318.1278660185766398 ) ) ;
#93565 = CARTESIAN_POINT ( 'NONE',  ( -102.2383502863162335, -297.7892401747529902, -309.8883087576965636 ) ) ;
#93566 = CARTESIAN_POINT ( 'NONE',  ( -44.31231391334680580, -292.4541006233025655, -197.5820026341282585 ) ) ;
#93567 = CARTESIAN_POINT ( 'NONE',  ( -73.80408897849801519, -288.2319407430913998, -334.1857974708884171 ) ) ;
#93568 = CARTESIAN_POINT ( 'NONE',  ( -52.53361257456068500, -274.5140145890978260, -194.9242658959265384 ) ) ;
#93569 = CARTESIAN_POINT ( 'NONE',  ( -110.1887733950832740, -272.6240159247767565, -264.9134524955282473 ) ) ;
#93570 = ORIENTED_EDGE ( 'NONE', *, *, #29763, .T. ) ;
#93571 = DIRECTION ( 'NONE',  ( 0.000000000000000000, 0.000000000000000000, -1.000000000000000000 ) ) ;
#93572 = DIRECTION ( 'NONE',  ( 0.000000000000000000, 1.000000000000000000, 0.000000000000000000 ) ) ;
#93573 = CARTESIAN_POINT ( 'NONE',  ( -76.76251448157525203, -281.4493582783108536, -205.8388142303484472 ) ) ;
#93574 = CARTESIAN_POINT ( 'NONE',  ( 113.5000000000000568, -298.0521521680024080, -540.3336712212508246 ) ) ;
#93575 = CARTESIAN_POINT ( 'NONE',  ( 0.5479901314351166564, -281.6493363018157652, -207.5441151669947146 ) ) ;
#93576 = CARTESIAN_POINT ( 'NONE',  ( -68.28073092407900901, -281.4114967859224521, -200.9441068037826881 ) ) ;
#93577 = CARTESIAN_POINT ( 'NONE',  ( -107.6210902219983012, -283.3387477574189006, -291.0024175355258649 ) ) ;
#93578 = CARTESIAN_POINT ( 'NONE',  ( -92.22573883598570887, -281.1173658121962262, -220.3750421590519579 ) ) ;
#93579 = CARTESIAN_POINT ( 'NONE',  ( 13.99337936448623765, -273.2685805253104263, -217.4894113236656494 ) ) ;
#93580 = CARTESIAN_POINT ( 'NONE',  ( 208.6515845757822092, 29.54020560868483614, 14.79569954156320755 ) ) ;
#93581 = DIRECTION ( 'NONE',  ( 0.000000000000000000, 0.000000000000000000, -1.000000000000000000 ) ) ;
#93582 = CARTESIAN_POINT ( 'NONE',  ( -80.12776709747809889, -278.4178555617960455, -334.2492284253174262 ) ) ;
#93583 = DIRECTION ( 'NONE',  ( 0.000000000000000000, 0.000000000000000000, 1.000000000000000000 ) ) ;
#93584 = CARTESIAN_POINT ( 'NONE',  ( -101.6112971142877228, -276.5793788903895347, -311.7859623163165566 ) ) ;
#93585 = VERTEX_POINT ( 'NONE', #75854 ) ;
#93586 = LINE ( 'NONE', #86471, #15669 ) ;
#93587 = CARTESIAN_POINT ( 'NONE',  ( -112.7089963026202213, -286.5006084235405979, -272.8212396622769802 ) ) ;
#93588 = CARTESIAN_POINT ( 'NONE',  ( 19.47765081189507796, -292.0984976963708846, -224.2526565087588040 ) ) ;
#93589 = CARTESIAN_POINT ( 'NONE',  ( -41.76299922752258453, -288.4550388337621030, -347.1451823561020547 ) ) ;
#93590 = CARTESIAN_POINT ( 'NONE',  ( -75.21971805218852580, -283.7796658139261012, -206.7747218624123491 ) ) ;
#93592 = CARTESIAN_POINT ( 'NONE',  ( -10.37550522456752589, -286.9353747170914630, -339.3421142969108928 ) ) ;
#93591 = CARTESIAN_POINT ( 'NONE',  ( -107.0849701354215853, -283.4381525016597720, -246.7229376067209046 ) ) ;
#93593 = CIRCLE ( 'NONE', #72467, 0.4999999999999989453 ) ;
#93594 = CARTESIAN_POINT ( 'NONE',  ( 17.91385157906054459, -283.4427727952519263, -318.6721365095476131 ) ) ;
#93595 = CARTESIAN_POINT ( 'NONE',  ( -31.39262931469024309, -272.1270991631888023, -195.5844924281386454 ) ) ;
#93596 = CARTESIAN_POINT ( 'NONE',  ( -108.5625833425994671, -282.6038184874507238, -297.6011734199836383 ) ) ;
#93597 = CARTESIAN_POINT ( 'NONE',  ( -60.93753984951238323, -297.3584137191123773, -341.6069532050947259 ) ) ;
#93598 = CARTESIAN_POINT ( 'NONE',  ( -75.16171495335872521, -283.5496724862859423, -205.3421655673130601 ) ) ;
#93599 = CARTESIAN_POINT ( 'NONE',  ( -110.6273434298098266, -279.4895994765356022, -270.6509087954026427 ) ) ;
#93600 = CARTESIAN_POINT ( 'NONE',  ( 1.764922937458136332, -288.5741197336049026, -206.1684357019360334 ) ) ;
#93601 = CARTESIAN_POINT ( 'NONE',  ( 201.2104617360081704, 41.21457449016151031, 10.50000000000000000 ) ) ;
#93602 = DIRECTION ( 'NONE',  ( -0.000000000000000000, -1.000000000000000000, -0.000000000000000000 ) ) ;
#93603 = CARTESIAN_POINT ( 'NONE',  ( 36.64677586122595443, -295.2761136007291043, -254.9674509712834833 ) ) ;
#93604 = CARTESIAN_POINT ( 'NONE',  ( -90.52144297317749988, -275.8047274809828195, -323.3207650710338612 ) ) ;
#93605 = CARTESIAN_POINT ( 'NONE',  ( -111.3891023459625131, -289.4916786962212427, -290.8828392937712692 ) ) ;
#93606 = CARTESIAN_POINT ( 'NONE',  ( 19.43566057468966335, -292.6134984156360019, -317.5073980996139653 ) ) ;
#93607 = CARTESIAN_POINT ( 'NONE',  ( -11.55452602452397315, -279.0798611649137229, -201.4867654609975887 ) ) ;
#93608 = CARTESIAN_POINT ( 'NONE',  ( -52.87073974470489190, -295.9907456324371537, -197.7155592323510973 ) ) ;
#93609 = CARTESIAN_POINT ( 'NONE',  ( -36.21525922393722396, -293.3817071330117869, -196.8640374757170832 ) ) ;
#93610 = CARTESIAN_POINT ( 'NONE',  ( -112.3452863284742875, -275.1604526064900824, -261.9424758988611188 ) ) ;
#93611 = CARTESIAN_POINT ( 'NONE',  ( -69.25574402688238251, -293.9442954969541120, -339.6877709368006890 ) ) ;
#93612 = CARTESIAN_POINT ( 'NONE',  ( -70.31173089497112016, -291.0942414483819789, -336.4010115599982669 ) ) ;
#93613 = CARTESIAN_POINT ( 'NONE',  ( -19.60130737881473806, -290.5169698961747713, -196.4202586060822000 ) ) ;
#93614 = CARTESIAN_POINT ( 'NONE',  ( 12.56865776422130843, -289.7657184070116045, -324.5074625283646128 ) ) ;
#93615 = CARTESIAN_POINT ( 'NONE',  ( 152.2746432211103809, 129.8137309627706202, -12.50000000000000178 ) ) ;
#93616 = CARTESIAN_POINT ( 'NONE',  ( -48.07459332465964508, -289.9948883152570147, -342.7821819764636757 ) ) ;
#93617 = CARTESIAN_POINT ( 'NONE',  ( 196.2438553357862077, 20.66497315817206015, 13.54628071421389102 ) ) ;
#93618 = CARTESIAN_POINT ( 'NONE',  ( -111.8727705987133305, -291.5340632731458754, -288.1126271521189892 ) ) ;
#93620 = CARTESIAN_POINT ( 'NONE',  ( -66.56407526866374269, -291.6584072887602588, -203.4652826028963091 ) ) ;
#93619 = CARTESIAN_POINT ( 'NONE',  ( 24.56438554161436372, -280.1525372114587640, -313.3494081264094007 ) ) ;
#93621 = CARTESIAN_POINT ( 'NONE',  ( -108.4947299461938002, -279.2589026792759910, -240.9844156633944010 ) ) ;
#93622 = CARTESIAN_POINT ( 'NONE',  ( -5.468148163555649255, -282.3109057271302618, -340.4312327019550253 ) ) ;
#93623 = CARTESIAN_POINT ( 'NONE',  ( 31.24396662788716128, -285.9510332028983726, -300.8379671649554439 ) ) ;
#93624 = CARTESIAN_POINT ( 'NONE',  ( 140.6539576904058606, 250.0000000000000568, 10.50000000000000000 ) ) ;
#93625 = CARTESIAN_POINT ( 'NONE',  ( 36.79836970385022710, -279.7404666801557482, -274.1181810831028542 ) ) ;
#93626 = CARTESIAN_POINT ( 'NONE',  ( -112.2135809361196408, -282.4853212611050139, -275.5532702530693996 ) ) ;
#93627 = CARTESIAN_POINT ( 'NONE',  ( 205.7381008070598227, 1.000000000000000888, 7.000000000000000000 ) ) ;
#93628 = CARTESIAN_POINT ( 'NONE',  ( -97.14137382993139624, -277.6721113180604448, -222.9616793681421711 ) ) ;
#93629 = CARTESIAN_POINT ( 'NONE',  ( -113.9007273961496196, -283.4056621478234206, -275.6825780289768772 ) ) ;
#93630 = CARTESIAN_POINT ( 'NONE',  ( -36.49195868421676892, -299.0043000310293451, -197.1256818783582787 ) ) ;
#93631 = CARTESIAN_POINT ( 'NONE',  ( 152.4536156746142410, 130.6065089285656313, -11.50000000000000000 ) ) ;
#93632 = CARTESIAN_POINT ( 'NONE',  ( -75.40954654446625227, -293.1359241787627639, -207.0774047863886551 ) ) ;
#93633 = CARTESIAN_POINT ( 'NONE',  ( 35.16503031913268273, -276.6696522843807884, -246.0826214834766006 ) ) ;
#93634 = CARTESIAN_POINT ( 'NONE',  ( 11.75878309051212511, -276.0147291737525848, -324.4781314715482381 ) ) ;
#93635 = CARTESIAN_POINT ( 'NONE',  ( 20.38844535829213811, -296.2132047940258985, -318.2383668027111980 ) ) ;
#93636 = CARTESIAN_POINT ( 'NONE',  ( -62.76164968260442123, -289.5406294146090431, -343.1005545414096787 ) ) ;
#93637 = CARTESIAN_POINT ( 'NONE',  ( 38.26960366667024260, -279.6269186979536698, -269.9627309050462713 ) ) ;
#93638 = CARTESIAN_POINT ( 'NONE',  ( -30.69515346537066591, -291.9671658303655022, -193.5957569260099262 ) ) ;
#93639 = CARTESIAN_POINT ( 'NONE',  ( -92.72661084203879511, -290.2914888084347353, -222.4453573829819391 ) ) ;
#93640 = CARTESIAN_POINT ( 'NONE',  ( -6.640318923675122775, -292.6488985916901129, -338.7893712419186727 ) ) ;
#93641 = ORIENTED_EDGE ( 'NONE', *, *, #8048, .F. ) ;
#93642 = DIRECTION ( 'NONE',  ( 0.000000000000000000, 1.000000000000000000, 0.000000000000000000 ) ) ;
#93643 = CARTESIAN_POINT ( 'NONE',  ( -4.800041469428300012, -292.0003163988286019, -204.9328945002685316 ) ) ;
#93644 = CARTESIAN_POINT ( 'NONE',  ( 189.9243309297870610, 275.0000000000000568, 20.22542485937349355 ) ) ;
#93645 = CARTESIAN_POINT ( 'NONE',  ( -82.08285599513421005, -270.9094976428775681, -214.2051214447836571 ) ) ;
#93646 = CARTESIAN_POINT ( 'NONE',  ( -85.06075887379175526, -296.4703360628379301, -210.2303301555177768 ) ) ;
#93647 = CARTESIAN_POINT ( 'NONE',  ( -111.7356591822077974, -285.6418680510804506, -288.2725368821278380 ) ) ;
#93648 = CARTESIAN_POINT ( 'NONE',  ( -4.592658239440970291, -286.3294855494381750, -205.1192582611393789 ) ) ;
#93649 = CARTESIAN_POINT ( 'NONE',  ( 8.022286106713780285, -277.9396609681482460, -328.5021096233390949 ) ) ;
#93650 = CARTESIAN_POINT ( 'NONE',  ( -42.52863166926879046, -293.1380147688722104, -344.8254889573555033 ) ) ;
#93651 = CARTESIAN_POINT ( 'NONE',  ( 36.54474554761870309, -295.2454610408362328, -265.2239831728599597 ) ) ;
#93652 = CARTESIAN_POINT ( 'NONE',  ( 33.27571837895451523, -274.6106959456377012, -290.4148429090494687 ) ) ;
#93653 = ORIENTED_EDGE ( 'NONE', *, *, #66553, .T. ) ;
#93654 = CARTESIAN_POINT ( 'NONE',  ( 195.4548275740021666, 39.96818058921539318, 13.92024756609993119 ) ) ;
#93655 = CARTESIAN_POINT ( 'NONE',  ( -97.39361016638247293, -295.5731925589939806, -318.5432969909085159 ) ) ;
#93656 = CARTESIAN_POINT ( 'NONE',  ( -34.49899005536793339, -290.9364441214599992, -344.7973821129947964 ) ) ;
#93657 = CARTESIAN_POINT ( 'NONE',  ( 201.3832976022252694, 295.1831209208456244, -54.00000000002625455 ) ) ;
#93658 = CARTESIAN_POINT ( 'NONE',  ( -60.06965241856088511, -298.8441150545593814, -197.0601143195720795 ) ) ;
#93659 = CARTESIAN_POINT ( 'NONE',  ( 16.96078226772647568, -287.5035835097140762, -221.4023360966625091 ) ) ;
#93661 = ORIENTED_EDGE ( 'NONE', *, *, #20271, .T. ) ;
#93660 = ADVANCED_FACE ( 'NONE', ( #69691 ), #20356, .T. ) ;
#93662 = CARTESIAN_POINT ( 'NONE',  ( -25.42027612801576808, -279.2593031002447219, -194.5277489276803919 ) ) ;
#93663 = CARTESIAN_POINT ( 'NONE',  ( 36.27452867675225434, -294.4849394841311891, -292.7668586998679530 ) ) ;
#93664 = CARTESIAN_POINT ( 'NONE',  ( -92.70664402750746547, -287.9743013490632393, -322.1574334306898777 ) ) ;
#93665 = CIRCLE ( 'NONE', #52826, 4.499999999999986677 ) ;
#93666 = CARTESIAN_POINT ( 'NONE',  ( -114.3449454533130734, -296.8590078222697457, -272.4734489240429980 ) ) ;
#93667 = CARTESIAN_POINT ( 'NONE',  ( 33.96953537580622395, -293.6774947106861759, -254.5935994513203866 ) ) ;
#93668 = CARTESIAN_POINT ( 'NONE',  ( 85.55100297371598117, -298.0521521680024080, -421.1172536214571096 ) ) ;
#93669 = DIRECTION ( 'NONE',  ( 8.659560562355067211E-17, -0.7071067811865364705, 0.7071067811865584529 ) ) ;
#93670 = CARTESIAN_POINT ( 'NONE',  ( 138.6539576904058606, 132.0000000000000568, -10.49999999999999822 ) ) ;
#93671 = AXIS2_PLACEMENT_3D ( 'NONE', #52272, #14910, #16295 ) ;
#93672 = CARTESIAN_POINT ( 'NONE',  ( 37.03940563166408850, -288.8566384710205170, -253.2691433512485730 ) ) ;
#93673 = CARTESIAN_POINT ( 'NONE',  ( 36.60358173371529489, -284.6237833571632905, -234.7871824221999191 ) ) ;
#93674 = CARTESIAN_POINT ( 'NONE',  ( -35.33037011089251678, -279.4253352337865408, -193.4762396088509888 ) ) ;
#93675 = CARTESIAN_POINT ( 'NONE',  ( -34.75836376808485539, -285.0198105545406975, -345.1626010497900552 ) ) ;
#93676 = CARTESIAN_POINT ( 'NONE',  ( -105.2687266526521341, -282.6710946624464214, -305.4698356563340553 ) ) ;
#93677 = CARTESIAN_POINT ( 'NONE',  ( 31.81407040063420055, -285.9950772939433818, -298.0462333479432004 ) ) ;
#93678 = CARTESIAN_POINT ( 'NONE',  ( -9.641004424644274096, -278.5544740503940488, -340.8804553185084956 ) ) ;
#93679 = CARTESIAN_POINT ( 'NONE',  ( -90.21484266159087895, -273.6116868797454913, -219.9789643280970495 ) ) ;
#93680 = VERTEX_POINT ( 'NONE', #53626 ) ;
#93681 = CARTESIAN_POINT ( 'NONE',  ( 10.60064419608459119, -293.0580428276577436, -326.0636771462835100 ) ) ;
#93683 = CARTESIAN_POINT ( 'NONE',  ( -76.87000942377420643, -278.8563283414132457, -208.8076459835046137 ) ) ;
#93682 = CARTESIAN_POINT ( 'NONE',  ( -108.8872461603217374, -278.7442524177691325, -255.7988692541840408 ) ) ;
#93684 = CARTESIAN_POINT ( 'NONE',  ( -13.17298574084568941, -275.4386129624982118, -197.5781134136069852 ) ) ;
#93685 = CARTESIAN_POINT ( 'NONE',  ( -113.6847796836970446, -277.2601015759275924, -277.2798653054476290 ) ) ;
#93686 = CARTESIAN_POINT ( 'NONE',  ( -113.6754805203053849, -271.0251410464779838, -270.3416754731575224 ) ) ;
#93687 = ADVANCED_FACE ( 'NONE', ( #46952 ), #3898, .F. ) ;
#93688 = CARTESIAN_POINT ( 'NONE',  ( -111.7279744946049931, -297.7565017923008099, -287.8901620553351108 ) ) ;
#93689 = DIRECTION ( 'NONE',  ( 1.000000000000000000, 0.000000000000000000, 0.000000000000000000 ) ) ;
#93690 = ORIENTED_EDGE ( 'NONE', *, *, #92757, .T. ) ;
#93691 = CARTESIAN_POINT ( 'NONE',  ( 157.4851178187871312, 69.18068689461284748, 7.000000000000000000 ) ) ;
#93692 = CARTESIAN_POINT ( 'NONE',  ( -102.5194722319832437, -286.0860743657551666, -236.8039414588454292 ) ) ;
#93693 = CARTESIAN_POINT ( 'NONE',  ( -107.0062009307126516, -286.7057907450686116, -239.8842628368695955 ) ) ;
#93694 = CARTESIAN_POINT ( 'NONE',  ( 35.65497047700259969, -286.8378613571862843, -265.5883020783349480 ) ) ;
#93695 = CARTESIAN_POINT ( 'NONE',  ( -101.3714150919689843, -283.4968292794517879, -313.1149287536795782 ) ) ;
#93696 = CARTESIAN_POINT ( 'NONE',  ( 33.89105063424882758, -279.6993192773426244, -251.0167181872071183 ) ) ;
#93697 = CARTESIAN_POINT ( 'NONE',  ( -27.69917805843504510, -288.0363375717602139, -196.7548190202378748 ) ) ;
#93698 = CARTESIAN_POINT ( 'NONE',  ( -8.962625000209827775, -278.9100997851881516, -202.3512962782413922 ) ) ;
#93699 = CARTESIAN_POINT ( 'NONE',  ( -91.31873723241153584, -279.1550691300693074, -320.3122010175063679 ) ) ;
#93700 = CARTESIAN_POINT ( 'NONE',  ( 17.32743406173155876, -275.3517884738028556, -221.8168489556452698 ) ) ;
#93701 = CARTESIAN_POINT ( 'NONE',  ( -31.87053940794593743, -287.7796243996576777, -346.8207006490806634 ) ) ;
#93702 = CARTESIAN_POINT ( 'NONE',  ( -37.30404601501494000, -283.8544837284365485, -347.2126711055896067 ) ) ;
#93703 = CARTESIAN_POINT ( 'NONE',  ( 24.20964569095865215, -282.6593706397758297, -316.5234265393917212 ) ) ;
#93704 = VERTEX_POINT ( 'NONE', #68296 ) ;
#93705 = VERTEX_POINT ( 'NONE', #39846 ) ;
#93706 = FACE_OUTER_BOUND ( 'NONE', #11452, .T. ) ;
#93707 = CARTESIAN_POINT ( 'NONE',  ( -8.678122513834807705, -290.5414901964716137, -340.5086359251633326 ) ) ;
#93708 = CARTESIAN_POINT ( 'NONE',  ( -111.7867486921140312, -289.0142218403041738, -288.0590210152830650 ) ) ;
#93709 = CARTESIAN_POINT ( 'NONE',  ( -76.68055102402266243, -272.5700539449761663, -208.5884439425717574 ) ) ;
#93710 = CARTESIAN_POINT ( 'NONE',  ( 33.23413576049146911, -292.5111270925425515, -239.8264790471268100 ) ) ;
#93711 = CARTESIAN_POINT ( 'NONE',  ( -97.92987621354390626, -288.4528223111061607, -312.3330354371690873 ) ) ;
#93712 = CARTESIAN_POINT ( 'NONE',  ( 28.04290555140037355, -292.2593024281230782, -305.1523755245782468 ) ) ;
#93713 = CARTESIAN_POINT ( 'NONE',  ( 35.94814091805673684, -288.6940514394966613, -265.5454418533481658 ) ) ;
#93714 = CARTESIAN_POINT ( 'NONE',  ( -95.99890600148557951, -299.6948066931273615, -223.6242672951989618 ) ) ;
#93715 = CARTESIAN_POINT ( 'NONE',  ( -18.25046875795010948, -280.8060991788453862, -342.9444327182633288 ) ) ;
#93716 = NEXT_ASSEMBLY_USAGE_OCCURRENCE ( 'NAUO1', ' ', ' ', #21587, #12282, $ ) ;
#93717 = NEXT_ASSEMBLY_USAGE_OCCURRENCE ( 'NAUO2', ' ', ' ', #21587, #45828, $ ) ;
#93718 = NEXT_ASSEMBLY_USAGE_OCCURRENCE ( 'NAUO3', ' ', ' ', #21587, #91591, $ ) ;
#93719 = NEXT_ASSEMBLY_USAGE_OCCURRENCE ( 'NAUO4', ' ', ' ', #21587, #79429, $ ) ;
#93720 = NEXT_ASSEMBLY_USAGE_OCCURRENCE ( 'NAUO5', ' ', ' ', #21587, #19232, $ ) ;
#93721 = NEXT_ASSEMBLY_USAGE_OCCURRENCE ( 'NAUO6', ' ', ' ', #21587, #74824, $ ) ;
#93722 = NEXT_ASSEMBLY_USAGE_OCCURRENCE ( 'NAUO7', ' ', ' ', #21587, #69577, $ ) ;
#93723 = NEXT_ASSEMBLY_USAGE_OCCURRENCE ( 'NAUO8', ' ', ' ', #21587, #9377, $ ) ;
#93724 = NEXT_ASSEMBLY_USAGE_OCCURRENCE ( 'NAUO9', ' ', ' ', #21587, #79429, $ ) ;
#93725=COLOUR_RGB('Dark Blue',0.08,0.2,0.34);
#93726=FILL_AREA_STYLE_COLOUR('',#93725);
#93727=FILL_AREA_STYLE('',(#93726));
#93728=SURFACE_STYLE_FILL_AREA(#93727);
#93729=SURFACE_SIDE_STYLE('',(#93728));
#93730=SURFACE_STYLE_USAGE(.BOTH.,#93729);
#93731=PRESENTATION_STYLE_ASSIGNMENT((#93730));
#93732=COLOUR_RGB('Light Blue',0.38,0.62,0.78);
#93733=FILL_AREA_STYLE_COLOUR('',#93732);
#93734=FILL_AREA_STYLE('',(#93733));
#93735=SURFACE_STYLE_FILL_AREA(#93734);
#93736=SURFACE_SIDE_STYLE('',(#93735));
#93737=SURFACE_STYLE_USAGE(.BOTH.,#93736);
#93738=PRESENTATION_STYLE_ASSIGNMENT((#93737));
#93739=COLOUR_RGB('Sky Blue',0.24,0.69,0.87);
#93740=FILL_AREA_STYLE_COLOUR('',#93739);
#93741=FILL_AREA_STYLE('',(#93740));
#93742=SURFACE_STYLE_FILL_AREA(#93741);
#93743=SURFACE_SIDE_STYLE('',(#93742));
#93744=SURFACE_STYLE_USAGE(.BOTH.,#93743);
#93745=PRESENTATION_STYLE_ASSIGNMENT((#93744));
#93746=COLOUR_RGB('Grey',0.48,0.52,0.57);
#93747=FILL_AREA_STYLE_COLOUR('',#93746);
#93748=FILL_AREA_STYLE('',(#93747));
#93749=SURFACE_STYLE_FILL_AREA(#93748);
#93750=SURFACE_SIDE_STYLE('',(#93749));
#93751=SURFACE_STYLE_USAGE(.BOTH.,#93750);
#93752=PRESENTATION_STYLE_ASSIGNMENT((#93751));
#93753=COLOUR_RGB('Black',0.12,0.14,0.17);
#93754=FILL_AREA_STYLE_COLOUR('',#93753);
#93755=FILL_AREA_STYLE('',(#93754));
#93756=SURFACE_STYLE_FILL_AREA(#93755);
#93757=SURFACE_SIDE_STYLE('',(#93756));
#93758=SURFACE_STYLE_USAGE(.BOTH.,#93757);
#93759=PRESENTATION_STYLE_ASSIGNMENT((#93758));
#93760=COLOUR_RGB('Off White',0.89,0.88,0.83);
#93761=FILL_AREA_STYLE_COLOUR('',#93760);
#93762=FILL_AREA_STYLE('',(#93761));
#93763=SURFACE_STYLE_FILL_AREA(#93762);
#93764=SURFACE_SIDE_STYLE('',(#93763));
#93765=SURFACE_STYLE_USAGE(.BOTH.,#93764);
#93766=PRESENTATION_STYLE_ASSIGNMENT((#93765));
ENDSEC;
END-ISO-10303-21;
